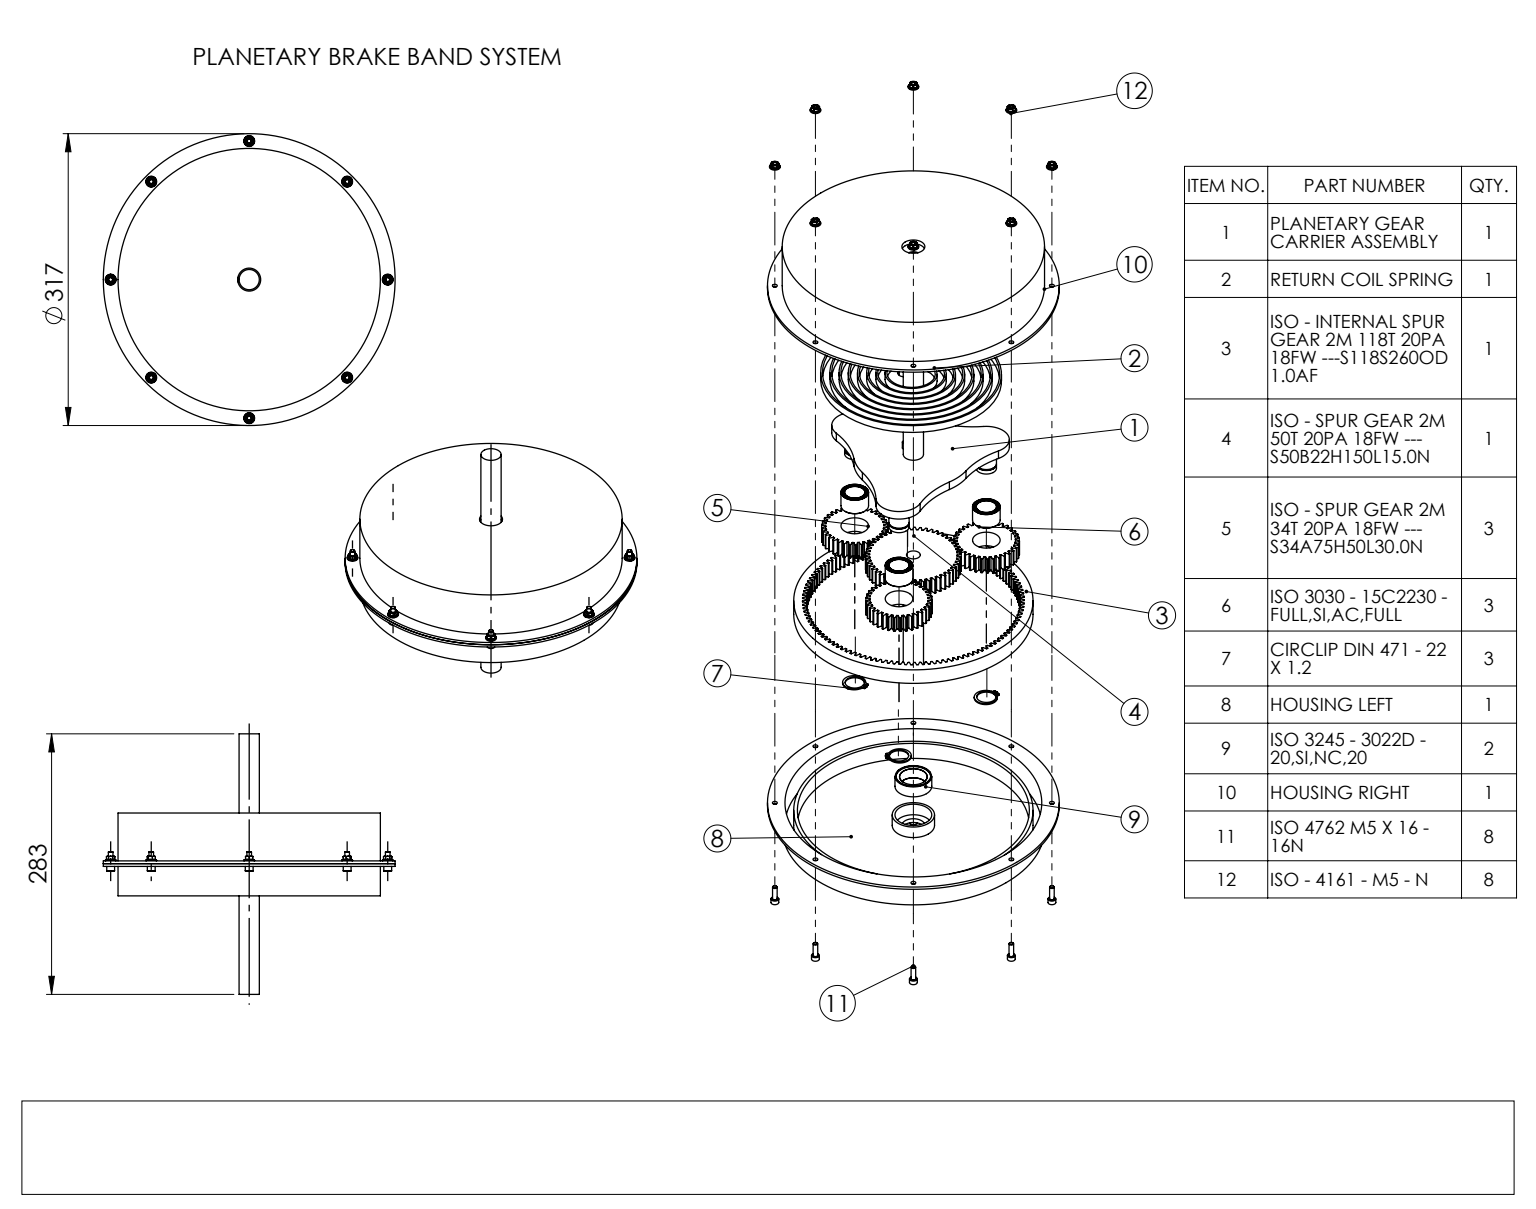
ISO-10303-21;
HEADER;
FILE_DESCRIPTION (('STEP AP214'),
    '1' );
FILE_NAME ('BR-544',
    '2026-10-08T11:45:07',
    ( '' ),
    ( '' ),
    'SwSTEP 2.0',
    'SolidWorks 2026',
    '' );
FILE_SCHEMA (( 'AUTOMOTIVE_DESIGN' ));
ENDSEC;

DATA;
#1 = TOROIDAL_SURFACE ( 'NONE', #14678, 14.91999999999999815, 0.08000000000000020983 ) ;
#2 = EDGE_CURVE ( 'NONE', #17487, #8430, #16356, .T. ) ;
#3 = AXIS2_PLACEMENT_3D ( 'NONE', #17893, #37479, #17456 ) ;
#4 = CYLINDRICAL_SURFACE ( 'NONE', #27715, 12.55910585664918422 ) ;
#5 = ORIENTED_EDGE ( 'NONE', *, *, #3352, .T. ) ;
#6 = CIRCLE ( 'NONE', #19608, 51.99999999999999289 ) ;
#7 = DIRECTION ( 'NONE',  ( 0.000000000000000000, 0.000000000000000000, 1.000000000000000000 ) ) ;
#8 = CARTESIAN_POINT ( 'NONE',  ( -38.31599561464027914, 40.00000000000000000, 10.26995502114586678 ) ) ;
#9 = CARTESIAN_POINT ( 'NONE',  ( -48.87578956996785706, 40.00000000000000000, 16.50293044077288940 ) ) ;
#10 = ORIENTED_EDGE ( 'NONE', *, *, #28549, .F. ) ;
#11 = ORIENTED_EDGE ( 'NONE', *, *, #25156, .T. ) ;
#12 = CARTESIAN_POINT ( 'NONE',  ( 18.00000000000000355, 45.78515115856060191, -12.64416602183617577 ) ) ;
#13 = DIRECTION ( 'NONE',  ( -1.000000000000000000, -0.000000000000000000, 0.000000000000000000 ) ) ;
#14 = CARTESIAN_POINT ( 'NONE',  ( 0.000000000000000000, -47.32430374665948136, 21.55018039121509688 ) ) ;
#15 = DIRECTION ( 'NONE',  ( 0.000000000000000000, -0.8443279255020199603, 0.5358267949789887741 ) ) ;
#16 = VERTEX_POINT ( 'NONE', #31754 ) ;
#17 = DIRECTION ( 'NONE',  ( -1.000000000000000000, -0.000000000000000000, -0.000000000000000000 ) ) ;
#18 = VERTEX_POINT ( 'NONE', #18483 ) ;
#19 = CARTESIAN_POINT ( 'NONE',  ( -15.99999999999997691, 17.11489954122026447, -2.499999999999994671 ) ) ;
#20 = EDGE_CURVE ( 'NONE', #11424, #24676, #28236, .T. ) ;
#21 = CARTESIAN_POINT ( 'NONE',  ( 0.000000000000000000, -2.357898499370432166, 3.035766082959412415E-15 ) ) ;
#22 = AXIS2_PLACEMENT_3D ( 'NONE', #1481, #10457, #24659 ) ;
#23 = ORIENTED_EDGE ( 'NONE', *, *, #27542, .T. ) ;
#24 = CARTESIAN_POINT ( 'NONE',  ( 17.99999999999999645, 110.3490479609632615, -20.28201389785435182 ) ) ;
#25 = CARTESIAN_POINT ( 'NONE',  ( 0.000000000000000000, 87.74575819880270444, -75.87280091124384285 ) ) ;
#26 = ORIENTED_EDGE ( 'NONE', *, *, #36883, .F. ) ;
#27 = DIRECTION ( 'NONE',  ( 0.000000000000000000, 0.000000000000000000, 1.000000000000000000 ) ) ;
#28 = EDGE_LOOP ( 'NONE', ( #968, #9890, #25897, #21708 ) ) ;
#29 = AXIS2_PLACEMENT_3D ( 'NONE', #16710, #27155, #33463 ) ;
#30 = DIRECTION ( 'NONE',  ( -1.000000000000000000, 0.000000000000000000, 0.000000000000000000 ) ) ;
#31 = AXIS2_PLACEMENT_3D ( 'NONE', #21762, #8191, #21965 ) ;
#32 = ORIENTED_EDGE ( 'NONE', *, *, #36401, .F. ) ;
#34 = EDGE_LOOP ( 'NONE', ( #7797, #14411, #2119, #1925 ) ) ;
#33 = DIRECTION ( 'NONE',  ( -1.000000000000000000, -0.000000000000000000, -0.000000000000000000 ) ) ;
#35 = CIRCLE ( 'NONE', #41130, 12.49999999999993427 ) ;
#36 = CARTESIAN_POINT ( 'NONE',  ( -50.06114249714176623, 31.00000000000000355, -38.53249520213265811 ) ) ;
#37 = ORIENTED_EDGE ( 'NONE', *, *, #41403, .T. ) ;
#38 = DIRECTION ( 'NONE',  ( 0.000000000000000000, 0.6382441836448160544, 0.7698339834299096074 ) ) ;
#39 = AXIS2_PLACEMENT_3D ( 'NONE', #35001, #14966, #41543 ) ;
#40 = EDGE_CURVE ( 'NONE', #21663, #37965, #25471, .T. ) ;
#41 = EDGE_LOOP ( 'NONE', ( #1865, #17158, #11037, #34239 ) ) ;
#42 = CARTESIAN_POINT ( 'NONE',  ( 17.99999999999999645, 101.1249659627849269, 48.60055280209592610 ) ) ;
#43 = ORIENTED_EDGE ( 'NONE', *, *, #17545, .T. ) ;
#44 = CARTESIAN_POINT ( 'NONE',  ( 25.34170449640226508, 40.00000000000000000, 74.97748276543396173 ) ) ;
#45 = CIRCLE ( 'NONE', #32135, 59.00000000000000000 ) ;
#47 = DIRECTION ( 'NONE',  ( 0.000000000000000000, 0.8183027759081663577, 0.5747874102144109321 ) ) ;
#46 = DIRECTION ( 'NONE',  ( 0.000000000000000000, 0.000000000000000000, 1.000000000000000000 ) ) ;
#48 = DIRECTION ( 'NONE',  ( 3.892440008040322386E-16, -2.658563593772947863E-15, -1.000000000000000000 ) ) ;
#49 = EDGE_LOOP ( 'NONE', ( #22549, #9625, #3734, #25351, #25610, #29887 ) ) ;
#50 = DIRECTION ( 'NONE',  ( 0.000000000000000000, -0.4610925014493325591, 0.8873520750565681015 ) ) ;
#51 = VERTEX_POINT ( 'NONE', #28063 ) ;
#52 = EDGE_CURVE ( 'NONE', #2224, #13079, #24812, .T. ) ;
#53 = SURFACE_SIDE_STYLE ('',( #30002 ) ) ;
#54 = VECTOR ( 'NONE', #12478, 1000.000000000000000 ) ;
#55 = DIRECTION ( 'NONE',  ( 1.000000000000000000, -0.000000000000000000, -0.000000000000000000 ) ) ;
#56 = CARTESIAN_POINT ( 'NONE',  ( 73.00591898829820536, 31.00000000000000000, 19.54754034098114701 ) ) ;
#58 = CARTESIAN_POINT ( 'NONE',  ( -6.076000000000004952, 19.11697999999999809, 0.000000000000000000 ) ) ;
#57 = CARTESIAN_POINT ( 'NONE',  ( -10.00000000000000000, 0.000000000000000000, 0.000000000000000000 ) ) ;
#59 = EDGE_LOOP ( 'NONE', ( #27677, #9320, #7424, #19818 ) ) ;
#60 = DIRECTION ( 'NONE',  ( 1.000000000000000000, 0.000000000000000000, 0.000000000000000000 ) ) ;
#61 = AXIS2_PLACEMENT_3D ( 'NONE', #7256, #13853, #27356 ) ;
#62 = AXIS2_PLACEMENT_3D ( 'NONE', #40135, #23391, #36432 ) ;
#63 = ORIENTED_EDGE ( 'NONE', *, *, #22832, .T. ) ;
#64 = CARTESIAN_POINT ( 'NONE',  ( 17.99999999999999645, 52.88069566989454273, 103.2454939717370905 ) ) ;
#65 = LINE ( 'NONE', #43070, #7397 ) ;
#66 = FILL_AREA_STYLE ('',( #17591 ) ) ;
#67 = AXIS2_PLACEMENT_3D ( 'NONE', #34351, #28055, #11038 ) ;
#68 = DIRECTION ( 'NONE',  ( 0.000000000000000000, 0.000000000000000000, -1.000000000000000000 ) ) ;
#69 = VERTEX_POINT ( 'NONE', #8400 ) ;
#70 = DIRECTION ( 'NONE',  ( -1.000000000000000000, 0.000000000000000000, 0.000000000000000000 ) ) ;
#71 = ORIENTED_EDGE ( 'NONE', *, *, #29230, .F. ) ;
#72 = EDGE_CURVE ( 'NONE', #28961, #19587, #1411, .T. ) ;
#73 = CONICAL_SURFACE ( 'NONE', #24545, 4.000000000000000000, 0.8911886515913786111 ) ;
#74 = CARTESIAN_POINT ( 'NONE',  ( -3.996523416598931009E-15, 2.658563593772952281E-14, 10.00000000000000178 ) ) ;
#75 = EDGE_CURVE ( 'NONE', #34974, #23352, #8192, .T. ) ;
#76 = DIRECTION ( 'NONE',  ( 0.000000000000000000, 0.000000000000000000, -1.000000000000000000 ) ) ;
#77 = CARTESIAN_POINT ( 'NONE',  ( 17.99999999999999645, -107.2703412112692689, -32.88383143828572486 ) ) ;
#78 = ORIENTED_EDGE ( 'NONE', *, *, #40490, .F. ) ;
#79 = ORIENTED_EDGE ( 'NONE', *, *, #11091, .T. ) ;
#80 = DIRECTION ( 'NONE',  ( 1.000000000000000000, 0.000000000000000000, 0.000000000000000000 ) ) ;
#81 = DIRECTION ( 'NONE',  ( 0.000000000000000000, 1.000000000000000000, -1.060184893785364939E-15 ) ) ;
#82 = DIRECTION ( 'NONE',  ( 0.000000000000000000, -1.000000000000000000, 1.287488025362403787E-15 ) ) ;
#84 = ORIENTED_EDGE ( 'NONE', *, *, #2078, .T. ) ;
#83 = DIRECTION ( 'NONE',  ( -1.000000000000000000, 0.000000000000000000, 0.000000000000000000 ) ) ;
#85 = CARTESIAN_POINT ( 'NONE',  ( 15.66220904948440662, 31.00000000000000355, -31.63873590539992264 ) ) ;
#86 = FACE_OUTER_BOUND ( 'NONE', #37742, .T. ) ;
#87 = EDGE_CURVE ( 'NONE', #8500, #34172, #3097, .T. ) ;
#89 = ORIENTED_EDGE ( 'NONE', *, *, #24562, .T. ) ;
#88 = DIRECTION ( 'NONE',  ( 0.000000000000000000, -0.3641605752528294659, 0.9313361774523355452 ) ) ;
#90 = ORIENTED_EDGE ( 'NONE', *, *, #30632, .T. ) ;
#91 = LINE ( 'NONE', #6449, #40012 ) ;
#92 = CIRCLE ( 'NONE', #23863, 2.500000000000000888 ) ;
#93 = DIRECTION ( 'NONE',  ( 0.000000000000000000, -0.3681245526846853022, 0.9297764858882484607 ) ) ;
#94 = CARTESIAN_POINT ( 'NONE',  ( 55.55275676651330485, 40.00000000000000000, 14.97830846782891712 ) ) ;
#95 = B_SPLINE_CURVE_WITH_KNOTS ( 'NONE', 3,
 ( #42025, #12179, #25497, #38758, #5606, #41162, #34637, #4752 ),
 .UNSPECIFIED., .F., .F.,
 ( 4, 2, 2, 4 ),
 ( 2.465131517071352357E-07, 0.001183067374689843057, 0.001774477805458910071, 0.002365888236227977302 ),
 .UNSPECIFIED. ) ;
#96 = DIRECTION ( 'NONE',  ( -1.000000000000000000, -0.000000000000000000, -0.000000000000000000 ) ) ;
#97 = AXIS2_PLACEMENT_3D ( 'NONE', #25295, #22018, #38332 ) ;
#98 = CARTESIAN_POINT ( 'NONE',  ( 17.99999999999999645, -63.24564713401724703, -102.5693868539701299 ) ) ;
#99 = AXIS2_PLACEMENT_3D ( 'NONE', #5218, #41425, #18366 ) ;
#100 = CARTESIAN_POINT ( 'NONE',  ( 17.99999999999999645, 103.1672962317651496, 44.09967643725903486 ) ) ;
#101 = EDGE_LOOP ( 'NONE', ( #3389, #16998, #1175, #14979 ) ) ;
#102 = CARTESIAN_POINT ( 'NONE',  ( 17.99999999999999645, 83.49789599728782719, 86.88263557826796557 ) ) ;
#103 = ORIENTED_EDGE ( 'NONE', *, *, #29129, .T. ) ;
#104 = EDGE_CURVE ( 'NONE', #19737, #29429, #22699, .T. ) ;
#105 = AXIS2_PLACEMENT_3D ( 'NONE', #12289, #32756, #5713 ) ;
#106 = DIRECTION ( 'NONE',  ( -1.000000000000000000, -0.000000000000000000, -0.000000000000000000 ) ) ;
#107 = DIRECTION ( 'NONE',  ( 0.000000000000000000, 0.000000000000000000, 1.000000000000000000 ) ) ;
#108 = ADVANCED_FACE ( 'NONE', ( #34802 ), #31105, .T. ) ;
#109 = CARTESIAN_POINT ( 'NONE',  ( 33.03432996520027132, 31.00000000000000355, -28.98482729919588863 ) ) ;
#110 = FACE_OUTER_BOUND ( 'NONE', #19769, .T. ) ;
#111 = EDGE_LOOP ( 'NONE', ( #9631, #34860, #21695, #15312 ) ) ;
#112 = MANIFOLD_SOLID_BREP ( 'Hex', #10772 ) ;
#113 = PRODUCT ( 'needle roller bearing_nm_iso_ISO 3030 - 15C2230 - Full,SI,AC,Full', 'needle roller bearing_nm_iso_ISO 3030 - 15C2230 - Full,SI,AC,Full', '', ( #9801 ) ) ;
#114 = CARTESIAN_POINT ( 'NONE',  ( 0.000000000000000000, 0.000000000000000000, 0.000000000000000000 ) ) ;
#115 = ORIENTED_EDGE ( 'NONE', *, *, #13945, .F. ) ;
#116 = CARTESIAN_POINT ( 'NONE',  ( -78.67873774631718220, 31.00000000000000711, 60.36924185307643143 ) ) ;
#117 = EDGE_LOOP ( 'NONE', ( #1029, #31405, #36009, #13275 ) ) ;
#118 = LINE ( 'NONE', #13486, #30404 ) ;
#119 = CARTESIAN_POINT ( 'NONE',  ( -67.85934734803990409, 31.00000000000000711, 22.92939687791763248 ) ) ;
#120 = CARTESIAN_POINT ( 'NONE',  ( 33.43413415811954792, 40.00000000000000000, -67.56680175473154293 ) ) ;
#121 = DIRECTION ( 'NONE',  ( -1.000000000000000000, -0.000000000000000000, -0.000000000000000000 ) ) ;
#122 = ORIENTED_EDGE ( 'NONE', *, *, #28926, .T. ) ;
#123 = EDGE_LOOP ( 'NONE', ( #24537, #25112, #5248, #36147 ) ) ;
#124 = CARTESIAN_POINT ( 'NONE',  ( 0.000000000000000000, 0.000000000000000000, 0.000000000000000000 ) ) ;
#125 = AXIS2_PLACEMENT_3D ( 'NONE', #20168, #39735, #23218 ) ;
#126 = ADVANCED_FACE ( 'NONE', ( #11053 ), #35784, .T. ) ;
#127 = CARTESIAN_POINT ( 'NONE',  ( 17.99999999999999645, -69.90696807222417419, -98.15042952503588936 ) ) ;
#128 = DIRECTION ( 'NONE',  ( -0.8660254037844377084, -0.5000000000000015543, 0.000000000000000000 ) ) ;
#129 = EDGE_CURVE ( 'NONE', #6394, #7217, #14300, .T. ) ;
#130 = EDGE_CURVE ( 'NONE', #29194, #21952, #31734, .T. ) ;
#131 = ADVANCED_FACE ( 'NONE', ( #11260 ), #25041, .T. ) ;
#133 = EDGE_CURVE ( 'NONE', #32336, #24871, #39498, .T. ) ;
#132 = CIRCLE ( 'NONE', #17653, 142.4999999999992610 ) ;
#135 = ORIENTED_EDGE ( 'NONE', *, *, #35134, .T. ) ;
#134 = DIRECTION ( 'NONE',  ( 3.009274222672345096E-17, 1.000000000000000000, -2.455023325076455345E-18 ) ) ;
#136 = CARTESIAN_POINT ( 'NONE',  ( 17.99999999999999645, 41.60679253225764285, 108.2814610871947423 ) ) ;
#137 = EDGE_LOOP ( 'NONE', ( #388, #32106, #23613, #3341 ) ) ;
#138 = CARTESIAN_POINT ( 'NONE',  ( 17.99999999999999645, 107.2885202478266251, 54.86040852957351888 ) ) ;
#139 = CARTESIAN_POINT ( 'NONE',  ( -5.399612364985466151, 40.00000000000000000, -82.39583333413678190 ) ) ;
#140 = CARTESIAN_POINT ( 'NONE',  ( -2.688821387764050996E-14, -4.618802153517012954, -0.4999999999999995559 ) ) ;
#141 = ORIENTED_EDGE ( 'NONE', *, *, #25701, .T. ) ;
#142 = DIRECTION ( 'NONE',  ( 1.000000000000000000, 0.000000000000000000, -0.000000000000000000 ) ) ;
#143 = CARTESIAN_POINT ( 'NONE',  ( 0.000000000000000000, 101.1249659627849269, 48.60055280209592610 ) ) ;
#144 = ORIENTED_EDGE ( 'NONE', *, *, #10315, .T. ) ;
#145 = ORIENTED_EDGE ( 'NONE', *, *, #19754, .F. ) ;
#146 = FACE_OUTER_BOUND ( 'NONE', #5091, .T. ) ;
#147 = ORIENTED_EDGE ( 'NONE', *, *, #18446, .T. ) ;
#148 = FACE_OUTER_BOUND ( 'NONE', #24269, .T. ) ;
#149 = DIRECTION ( 'NONE',  ( 0.000000000000000000, 0.000000000000000000, 1.000000000000000000 ) ) ;
#150 = CARTESIAN_POINT ( 'NONE',  ( 17.99999999999999645, 69.90696807222620635, -98.15042952503443985 ) ) ;
#151 = DIRECTION ( 'NONE',  ( 0.000000000000000000, 0.000000000000000000, -1.000000000000000000 ) ) ;
#152 = CARTESIAN_POINT ( 'NONE',  ( 17.99999999999999645, -53.40478689619660457, -108.0204598100370816 ) ) ;
#153 = ORIENTED_EDGE ( 'NONE', *, *, #32598, .F. ) ;
#155 = DIRECTION ( 'NONE',  ( 1.000000000000000000, 0.000000000000000000, 0.000000000000000000 ) ) ;
#154 = CARTESIAN_POINT ( 'NONE',  ( 17.99999999999999645, 120.2856157092986678, 7.201503623197233139 ) ) ;
#156 = EDGE_LOOP ( 'NONE', ( #41702, #6494, #6185, #41274 ) ) ;
#157 = ADVANCED_FACE ( 'NONE', ( #19485 ), #6553, .F. ) ;
#158 = AXIS2_PLACEMENT_3D ( 'NONE', #4980, #24654, #21174 ) ;
#159 =( LENGTH_UNIT ( ) NAMED_UNIT ( * ) SI_UNIT ( .MILLI., .METRE. ) );
#160 = CARTESIAN_POINT ( 'NONE',  ( 9.000000000000001776, -13.00789606333550097, 115.2683592318614672 ) ) ;
#161 = ADVANCED_FACE ( 'NONE', ( #9836 ), #29711, .F. ) ;
#162 = DIRECTION ( 'NONE',  ( 0.000000000000000000, 0.1062934856473588541, 0.9943348002101377592 ) ) ;
#163 = ORIENTED_EDGE ( 'NONE', *, *, #20925, .F. ) ;
#164 = CARTESIAN_POINT ( 'NONE',  ( 17.99999999999999645, -97.89532456239533076, 54.81585448086167389 ) ) ;
#165 = CIRCLE ( 'NONE', #25315, 58.99999999999999289 ) ;
#166 = DIRECTION ( 'NONE',  ( 1.000000000000000000, 0.000000000000000000, 0.000000000000000000 ) ) ;
#167 = DIRECTION ( 'NONE',  ( 0.000000000000000000, 0.000000000000000000, 1.000000000000000000 ) ) ;
#168 = CARTESIAN_POINT ( 'NONE',  ( -23.19911330973958030, 31.00000000000000355, -68.30030121463531145 ) ) ;
#169 = AXIS2_PLACEMENT_3D ( 'NONE', #24006, #33787, #20520 ) ;
#170 = VERTEX_POINT ( 'NONE', #16346 ) ;
#171 = CARTESIAN_POINT ( 'NONE',  ( 32.80084743084299248, 31.00000000000000355, 19.01436317119123842 ) ) ;
#172 = CARTESIAN_POINT ( 'NONE',  ( -21.28946418274055929, 40.00000000000000000, -79.45670318283352174 ) ) ;
#173 = DIRECTION ( 'NONE',  ( 1.000000000000000000, 0.000000000000000000, 0.000000000000000000 ) ) ;
#174 = EDGE_CURVE ( 'NONE', #31622, #37862, #2414, .T. ) ;
#175 = EDGE_CURVE ( 'NONE', #28450, #28268, #33086, .T. ) ;
#176 = ADVANCED_FACE ( 'NONE', ( #26221 ), #23396, .F. ) ;
#177 = ORIENTED_EDGE ( 'NONE', *, *, #6345, .F. ) ;
#178 = CARTESIAN_POINT ( 'NONE',  ( 18.00000000000000355, 20.99948489194481738, -42.60488980472760545 ) ) ;
#179 = DIRECTION ( 'NONE',  ( -1.000000000000000000, 0.000000000000000000, 0.000000000000000000 ) ) ;
#180 = ADVANCED_FACE ( 'NONE', ( #36225 ), #26652, .F. ) ;
#181 = AXIS2_PLACEMENT_3D ( 'NONE', #33308, #3602, #40474 ) ;
#182 = ORIENTED_EDGE ( 'NONE', *, *, #35349, .F. ) ;
#183 = CARTESIAN_POINT ( 'NONE',  ( 50.09382087749727930, 40.00000000000000000, 24.69014870349942825 ) ) ;
#184 = DIRECTION ( 'NONE',  ( -0.2140725878556641593, -0.9768177553304296934, 0.000000000000000000 ) ) ;
#185 = CARTESIAN_POINT ( 'NONE',  ( 53.30287614962722387, -35.35525454449572180, 69.29271901957299917 ) ) ;
#186 = ORIENTED_EDGE ( 'NONE', *, *, #2030, .F. ) ;
#187 = CARTESIAN_POINT ( 'NONE',  ( 0.000000000000000000, 82.63181128086846172, -81.41243003646886223 ) ) ;
#188 = CARTESIAN_POINT ( 'NONE',  ( -36.79328511490363240, -2.055254544495723756, -55.66638716446937707 ) ) ;
#189 = VERTEX_POINT ( 'NONE', #6781 ) ;
#190 = CARTESIAN_POINT ( 'NONE',  ( 17.99999999999999645, -31.80866420683992857, 2.997093558041182160 ) ) ;
#191 = EDGE_CURVE ( 'NONE', #37998, #17546, #11534, .T. ) ;
#192 = VERTEX_POINT ( 'NONE', #36012 ) ;
#193 = COLOUR_RGB ( '', 0.72549020, 0.75294118, 0.79215686) ;
#194 = AXIS2_PLACEMENT_3D ( 'NONE', #18783, #32450, #2540 ) ;
#195 = ORIENTED_EDGE ( 'NONE', *, *, #39418, .T. ) ;
#196 = DIRECTION ( 'NONE',  ( -3.996523416598930318E-16, 2.658563593772947863E-15, 1.000000000000000000 ) ) ;
#197 = CARTESIAN_POINT ( 'NONE',  ( 96.56285295106283684, 31.00000000000000000, 12.84127866191736977 ) ) ;
#198 = ORIENTED_EDGE ( 'NONE', *, *, #13590, .F. ) ;
#199 = CARTESIAN_POINT ( 'NONE',  ( 9.000000000000001776, -30.03615769709704608, -42.44795908869020451 ) ) ;
#200 = DIRECTION ( 'NONE',  ( -0.000000000000000000, -0.000000000000000000, 1.000000000000000000 ) ) ;
#201 = DIRECTION ( 'NONE',  ( 1.000000000000000000, -0.000000000000000000, 0.000000000000000000 ) ) ;
#202 = ORIENTED_EDGE ( 'NONE', *, *, #13580, .T. ) ;
#203 = CARTESIAN_POINT ( 'NONE',  ( 0.000000000000000000, -112.8457601792517124, 26.86697618949339272 ) ) ;
#204 = LINE ( 'NONE', #34053, #4600 ) ;
#205 = AXIS2_PLACEMENT_3D ( 'NONE', #38248, #21520, #38029 ) ;
#207 = CYLINDRICAL_SURFACE ( 'NONE', #17131, 20.00000000000000355 ) ;
#206 = DIRECTION ( 'NONE',  ( 0.000000000000000000, -0.9407002666710364558, 0.3392388661180213427 ) ) ;
#208 = AXIS2_PLACEMENT_3D ( 'NONE', #11929, #8841, #8617 ) ;
#209 = CARTESIAN_POINT ( 'NONE',  ( 17.99999999999999645, -110.0562500189201955, 49.07252625220073838 ) ) ;
#210 = ORIENTED_EDGE ( 'NONE', *, *, #16995, .T. ) ;
#211 =( LENGTH_UNIT ( ) NAMED_UNIT ( * ) SI_UNIT ( .MILLI., .METRE. ) );
#212 = AXIS2_PLACEMENT_3D ( 'NONE', #31464, #8530, #17983 ) ;
#213 = CARTESIAN_POINT ( 'NONE',  ( -25.29482881991252086, 31.00000000000000355, -32.96004927633274662 ) ) ;
#214 = VERTEX_POINT ( 'NONE', #29493 ) ;
#215 = DIRECTION ( 'NONE',  ( 1.000000000000000000, 0.000000000000000000, -3.273063162220425331E-16 ) ) ;
#216 = DIRECTION ( 'NONE',  ( -1.000000000000000000, 0.000000000000000000, 0.000000000000000000 ) ) ;
#217 = ORIENTED_EDGE ( 'NONE', *, *, #22395, .F. ) ;
#218 = LINE ( 'NONE', #26245, #34087 ) ;
#219 = CARTESIAN_POINT ( 'NONE',  ( 32.11716166826300167, 40.00000000000000000, 15.82712457579038912 ) ) ;
#220 = STYLED_ITEM ( 'NONE', ( #39718 ), #29693 ) ;
#221 = CARTESIAN_POINT ( 'NONE',  ( 42.86166521172830102, 40.00000000000000000, 21.22462828019262204 ) ) ;
#222 = AXIS2_PLACEMENT_3D ( 'NONE', #57, #6628, #19990 ) ;
#223 = ORIENTED_EDGE ( 'NONE', *, *, #13346, .T. ) ;
#224 = CARTESIAN_POINT ( 'NONE',  ( 17.99999999999999645, -23.87611429743648017, -20.54551452399645939 ) ) ;
#225 = DIRECTION ( 'NONE',  ( -1.000000000000000000, 0.000000000000000000, 0.000000000000000000 ) ) ;
#226 = EDGE_CURVE ( 'NONE', #9576, #14223, #10277, .T. ) ;
#227 = AXIS2_PLACEMENT_3D ( 'NONE', #26910, #27140, #24089 ) ;
#228 = CARTESIAN_POINT ( 'NONE',  ( -102.9608013043458072, -35.35525454449571470, 14.45886780445738218 ) ) ;
#229 = ORIENTED_EDGE ( 'NONE', *, *, #13847, .F. ) ;
#230 = CARTESIAN_POINT ( 'NONE',  ( 7.028922914820973311, 40.00000000000000000, 26.21578750688660264 ) ) ;
#231 = ORIENTED_EDGE ( 'NONE', *, *, #17154, .T. ) ;
#232 = LINE ( 'NONE', #33434, #6211 ) ;
#233 = CARTESIAN_POINT ( 'NONE',  ( 0.000000000000000000, 12.42760411676038146, 33.78690065568429191 ) ) ;
#234 =( REPRESENTATION_RELATIONSHIP ('NONE','NONE', #330, #37437 ) REPRESENTATION_RELATIONSHIP_WITH_TRANSFORMATION ( #8267 )SHAPE_REPRESENTATION_RELATIONSHIP( ) );
#235 = VERTEX_POINT ( 'NONE', #20345 ) ;
#236 = DIRECTION ( 'NONE',  ( 0.000000000000000000, 0.3140767120219495334, -0.9493976084683810601 ) ) ;
#237 = VECTOR ( 'NONE', #15107, 1000.000000000000000 ) ;
#238 = FACE_OUTER_BOUND ( 'NONE', #26879, .T. ) ;
#239 = VERTEX_POINT ( 'NONE', #9633 ) ;
#240 = CYLINDRICAL_SURFACE ( 'NONE', #4769, 20.00000000000000355 ) ;
#241 = EDGE_LOOP ( 'NONE', ( #31770, #30351, #32768, #20385 ) ) ;
#242 = DIRECTION ( 'NONE',  ( -1.000000000000000000, -0.000000000000000000, -0.000000000000000000 ) ) ;
#243 = EDGE_CURVE ( 'NONE', #7044, #26460, #16384, .T. ) ;
#244 = CIRCLE ( 'NONE', #9337, 59.00000000000001421 ) ;
#245 = ORIENTED_EDGE ( 'NONE', *, *, #22971, .F. ) ;
#247 = ORIENTED_EDGE ( 'NONE', *, *, #11286, .T. ) ;
#246 = CARTESIAN_POINT ( 'NONE',  ( 150.4999999999986926, 1.388241670201576064E-12, 6.999999999999959144 ) ) ;
#248 = EDGE_CURVE ( 'NONE', #1617, #22493, #17123, .T. ) ;
#249 = CARTESIAN_POINT ( 'NONE',  ( -20.51812799676685373, 31.00000000000000355, -60.74091093256831897 ) ) ;
#250 = EDGE_LOOP ( 'NONE', ( #8958, #20095, #42612, #31165 ) ) ;
#251 = DIRECTION ( 'NONE',  ( -1.000000000000000000, -0.000000000000000000, 0.000000000000000000 ) ) ;
#252 = VERTEX_POINT ( 'NONE', #20289 ) ;
#253 = ORIENTED_EDGE ( 'NONE', *, *, #22562, .T. ) ;
#254 = DIRECTION ( 'NONE',  ( 0.000000000000000000, -6.938893903907226011E-15, 1.000000000000000000 ) ) ;
#255 = VERTEX_POINT ( 'NONE', #36433 ) ;
#257 = CARTESIAN_POINT ( 'NONE',  ( -10.54315780146311532, 40.00000000000000000, 79.17709703063971460 ) ) ;
#256 = MECHANICAL_DESIGN_GEOMETRIC_PRESENTATION_REPRESENTATION (  '', ( #37909 ), #12862 ) ;
#259 = LINE ( 'NONE', #7052, #31169 ) ;
#258 = DIRECTION ( 'NONE',  ( 1.000000000000000000, 0.000000000000000000, 0.000000000000000000 ) ) ;
#260 = FACE_OUTER_BOUND ( 'NONE', #10790, .T. ) ;
#261 = ORIENTED_EDGE ( 'NONE', *, *, #7947, .F. ) ;
#262 = DIRECTION ( 'NONE',  ( 0.000000000000000000, -0.9980267284282708928, -0.06279051952932436509 ) ) ;
#263 = AXIS2_PLACEMENT_3D ( 'NONE', #41212, #8072, #27508 ) ;
#264 = ORIENTED_EDGE ( 'NONE', *, *, #41206, .T. ) ;
#265 = FILL_AREA_STYLE_COLOUR ( '', #39229 ) ;
#266 = CIRCLE ( 'NONE', #34432, 20.00000000000000711 ) ;
#267 = VERTEX_POINT ( 'NONE', #42555 ) ;
#268 = VECTOR ( 'NONE', #36102, 1000.000000000000000 ) ;
#269 = DIRECTION ( 'NONE',  ( 0.000000000000000000, 0.000000000000000000, 1.000000000000000000 ) ) ;
#270 = CARTESIAN_POINT ( 'NONE',  ( -45.94448050778635917, 31.00000000000000355, -79.54744219826071117 ) ) ;
#271 = CARTESIAN_POINT ( 'NONE',  ( 3.453038570460273071, 2.625189405340834448, -3.535263753543585352 ) ) ;
#272 = EDGE_LOOP ( 'NONE', ( #37199, #32601, #38048, #42708 ) ) ;
#273 = AXIS2_PLACEMENT_3D ( 'NONE', #24892, #15283, #24662 ) ;
#274 = CARTESIAN_POINT ( 'NONE',  ( 0.000000000000000000, -47.58001226230612701, 110.7096808509482031 ) ) ;
#275 = AXIS2_PLACEMENT_3D ( 'NONE', #8438, #38320, #31571 ) ;
#276 = VERTEX_POINT ( 'NONE', #12704 ) ;
#277 = FACE_OUTER_BOUND ( 'NONE', #26968, .T. ) ;
#278 = DIRECTION ( 'NONE',  ( 1.000000000000000000, 0.000000000000000000, 0.000000000000000000 ) ) ;
#279 = DIRECTION ( 'NONE',  ( 0.000000000000000000, 2.587384167558627638E-15, -1.000000000000000000 ) ) ;
#280 = EDGE_CURVE ( 'NONE', #25913, #26598, #17814, .T. ) ;
#281 = CARTESIAN_POINT ( 'NONE',  ( 106.9999999999993179, -2.318365118890836037E-13, -32.00000000000000000 ) ) ;
#282 = AXIS2_PLACEMENT_3D ( 'NONE', #26118, #29184, #16298 ) ;
#283 = ADVANCED_FACE ( 'NONE', ( #13571 ), #32962, .T. ) ;
#284 = AXIS2_PLACEMENT_3D ( 'NONE', #17141, #30851, #4209 ) ;
#285 = EDGE_LOOP ( 'NONE', ( #5183, #4420, #32510, #24970 ) ) ;
#286 = CARTESIAN_POINT ( 'NONE',  ( -10.00000000000000000, 0.000000000000000000, 0.000000000000000000 ) ) ;
#287 = VERTEX_POINT ( 'NONE', #19913 ) ;
#288 = DIRECTION ( 'NONE',  ( 1.000000000000000000, -0.000000000000000000, 0.000000000000000000 ) ) ;
#289 = DIRECTION ( 'NONE',  ( -1.000000000000000000, -0.000000000000000000, -0.000000000000000000 ) ) ;
#290 = DIRECTION ( 'NONE',  ( -1.000000000000000000, -0.000000000000000000, 0.000000000000000000 ) ) ;
#291 = VERTEX_POINT ( 'NONE', #33181 ) ;
#292 = ORIENTED_EDGE ( 'NONE', *, *, #9832, .T. ) ;
#293 = DIRECTION ( 'NONE',  ( -1.000000000000000000, -0.000000000000000000, -0.000000000000000000 ) ) ;
#294 = VECTOR ( 'NONE', #25496, 1000.000000000000000 ) ;
#295 = CARTESIAN_POINT ( 'NONE',  ( 0.000000000000000000, -58.30069736313732420, 100.2847380560565256 ) ) ;
#296 = EDGE_CURVE ( 'NONE', #640, #8463, #3270, .T. ) ;
#297 = CARTESIAN_POINT ( 'NONE',  ( 4.197478902586992966, -0.8524102783748346290, -3.505063281295504041 ) ) ;
#298 = AXIS2_PLACEMENT_3D ( 'NONE', #37715, #19724, #6582 ) ;
#300 = VERTEX_POINT ( 'NONE', #27299 ) ;
#299 = DIRECTION ( 'NONE',  ( 0.000000000000000000, 0.000000000000000000, 1.000000000000000000 ) ) ;
#301 = EDGE_CURVE ( 'NONE', #6489, #17266, #7326, .T. ) ;
#302 = CARTESIAN_POINT ( 'NONE',  ( -29.39530816626169241, 31.00000000000000355, -14.54745122861254814 ) ) ;
#303 = CIRCLE ( 'NONE', #42788, 24.99999999999998934 ) ;
#304 = CYLINDRICAL_SURFACE ( 'NONE', #9787, 116.0000000000000000 ) ;
#305 = AXIS2_PLACEMENT_3D ( 'NONE', #35239, #21983, #28308 ) ;
#306 = ADVANCED_FACE ( 'NONE', ( #37955 ), #862, .F. ) ;
#308 = ORIENTED_EDGE ( 'NONE', *, *, #23205, .T. ) ;
#307 = CARTESIAN_POINT ( 'NONE',  ( 0.000000000000000000, -18.53613841426822972, 48.58406706613896375 ) ) ;
#309 = UNCERTAINTY_MEASURE_WITH_UNIT (LENGTH_MEASURE( 1.000000000000000082E-05 ), #5379, 'distance_accuracy_value', 'NONE');
#310 = AXIS2_PLACEMENT_3D ( 'NONE', #8177, #1395, #28267 ) ;
#311 = ORIENTED_EDGE ( 'NONE', *, *, #38978, .F. ) ;
#312 = CARTESIAN_POINT ( 'NONE',  ( -130.0000000000000284, 4.615443851143735910E-16, -20.00000000000000000 ) ) ;
#313 = CARTESIAN_POINT ( 'NONE',  ( 0.000000000000000000, -69.72480978690109055, 92.70626138605992139 ) ) ;
#314 = CARTESIAN_POINT ( 'NONE',  ( -17.30549157494238344, 40.00000000000000000, -51.24895740946764988 ) ) ;
#315 = DIRECTION ( 'NONE',  ( -1.000000000000000000, 0.000000000000000000, -0.000000000000000000 ) ) ;
#316 = DIRECTION ( 'NONE',  ( 0.000000000000000000, 0.000000000000000000, -1.000000000000000000 ) ) ;
#317 = EDGE_LOOP ( 'NONE', ( #16591, #23774, #39955, #12184 ) ) ;
#318 = CARTESIAN_POINT ( 'NONE',  ( -6.004904395537136175, 0.000000000000000000, 0.000000000000000000 ) ) ;
#319 = EDGE_CURVE ( 'NONE', #36754, #15839, #12891, .T. ) ;
#320 = CIRCLE ( 'NONE', #19206, 15.08402000000000065 ) ;
#321 = ORIENTED_EDGE ( 'NONE', *, *, #37167, .T. ) ;
#322 = EDGE_CURVE ( 'NONE', #29751, #6854, #14213, .T. ) ;
#323 = LINE ( 'NONE', #26764, #22557 ) ;
#324 = CARTESIAN_POINT ( 'NONE',  ( -105.9879088449591933, 17.11489954122026447, -4.880719929157669945 ) ) ;
#326 = EDGE_CURVE ( 'NONE', #40378, #9051, #40786, .T. ) ;
#325 = CARTESIAN_POINT ( 'NONE',  ( 3.108867721649529958, 31.00000000000000355, 47.39583333474234905 ) ) ;
#327 = DIRECTION ( 'NONE',  ( 0.000000000000000000, 0.7980172272802363853, 0.6026346363792605132 ) ) ;
#328 = ORIENTED_EDGE ( 'NONE', *, *, #42015, .T. ) ;
#329 = AXIS2_PLACEMENT_3D ( 'NONE', #17951, #33827, #8078 ) ;
#330 = SHAPE_REPRESENTATION ( 'BR-544', ( #39970, #29548, #18472, #10727, #11463, #9346, #30946, #39281, #26770, #15640, #19143, #4447, #33013, #7253, #17047, #35107, #30261, #40659, #33731, #14235, #3017, #6528, #42769, #10026, #3741, #24722, #13548, #28191, #14967, #38586, #22632, #19820, #27462, #32334 ), #21922 ) ;
#331 = AXIS2_PLACEMENT_3D ( 'NONE', #35354, #42727, #6106 ) ;
#332 = AXIS2_PLACEMENT_3D ( 'NONE', #8992, #29286, #42557 ) ;
#333 = CARTESIAN_POINT ( 'NONE',  ( -20.64238946400878305, 31.00000000000000355, 3.177240882809045708 ) ) ;
#334 = ORIENTED_EDGE ( 'NONE', *, *, #29415, .T. ) ;
#335 = CARTESIAN_POINT ( 'NONE',  ( 58.84426737335365232, 31.00000000000000355, 76.69096868241209108 ) ) ;
#336 = VECTOR ( 'NONE', #7785, 1000.000000000000000 ) ;
#337 = ORIENTED_EDGE ( 'NONE', *, *, #41838, .F. ) ;
#338 = AXIS2_PLACEMENT_3D ( 'NONE', #11324, #23403, #24655 ) ;
#339 = CARTESIAN_POINT ( 'NONE',  ( 17.99999999999999645, -10.40101730206447961, 120.0512800434970728 ) ) ;
#340 = CARTESIAN_POINT ( 'NONE',  ( -25.88810397299713628, 31.00000000000000355, 75.89534075019484760 ) ) ;
#342 = AXIS2_PLACEMENT_3D ( 'NONE', #2271, #15629, #28936 ) ;
#341 = CARTESIAN_POINT ( 'NONE',  ( -79.00001692107187523, 40.00000000000000711, 21.04436337234429999 ) ) ;
#343 = FACE_OUTER_BOUND ( 'NONE', #19727, .T. ) ;
#344 = EDGE_CURVE ( 'NONE', #2343, #1360, #19212, .T. ) ;
#345 = AXIS2_PLACEMENT_3D ( 'NONE', #9675, #6388, #43032 ) ;
#346 = ORIENTED_EDGE ( 'NONE', *, *, #31412, .T. ) ;
#347 = DIRECTION ( 'NONE',  ( -1.000000000000000000, -0.000000000000000000, -0.000000000000000000 ) ) ;
#348 = ORIENTED_EDGE ( 'NONE', *, *, #42438, .F. ) ;
#349 = DIRECTION ( 'NONE',  ( -1.000000000000000000, -0.000000000000000000, -0.000000000000000000 ) ) ;
#350 = FACE_OUTER_BOUND ( 'NONE', #25908, .T. ) ;
#352 = ORIENTED_EDGE ( 'NONE', *, *, #296, .F. ) ;
#351 = CYLINDRICAL_SURFACE ( 'NONE', #6056, 18.77999999999999403 ) ;
#353 = LINE ( 'NONE', #36584, #16374 ) ;
#354 = ORIENTED_EDGE ( 'NONE', *, *, #6008, .F. ) ;
#355 = DIRECTION ( 'NONE',  ( 0.000000000000000000, 0.7705132427757904745, -0.6374239897486881912 ) ) ;
#356 = EDGE_CURVE ( 'NONE', #26178, #21757, #8740, .T. ) ;
#357 = CARTESIAN_POINT ( 'NONE',  ( 36.87680687886029318, 40.00000000000000000, -74.81172728975037955 ) ) ;
#358 = DIRECTION ( 'NONE',  ( -1.000000000000000000, -0.000000000000000000, -0.000000000000000000 ) ) ;
#359 = ORIENTED_EDGE ( 'NONE', *, *, #32192, .T. ) ;
#360 = CARTESIAN_POINT ( 'NONE',  ( 17.99999999999999645, -103.5682682299991342, 43.14958040911493242 ) ) ;
#361 = EDGE_CURVE ( 'NONE', #10268, #41981, #3126, .T. ) ;
#362 = DIRECTION ( 'NONE',  ( 0.000000000000000000, 0.000000000000000000, 1.000000000000000000 ) ) ;
#363 = VECTOR ( 'NONE', #4205, 1000.000000000000000 ) ;
#364 = ADVANCED_FACE ( 'NONE', ( #3690, #17069 ), #21009, .F. ) ;
#365 = EDGE_LOOP ( 'NONE', ( #40363, #21648, #12484, #22363 ) ) ;
#366 = AXIS2_PLACEMENT_3D ( 'NONE', #25494, #18321, #32020 ) ;
#367 = VECTOR ( 'NONE', #17531, 1000.000000000000000 ) ;
#368 = ORIENTED_EDGE ( 'NONE', *, *, #3508, .T. ) ;
#369 = LINE ( 'NONE', #17453, #16327 ) ;
#370 = ORIENTED_EDGE ( 'NONE', *, *, #15483, .F. ) ;
#371 = CARTESIAN_POINT ( 'NONE',  ( -4.000000000000000000, -2.309401076758512694, -5.000000000000000000 ) ) ;
#372 = CIRCLE ( 'NONE', #37296, 58.99999999999999289 ) ;
#373 = CARTESIAN_POINT ( 'NONE',  ( 18.00000000000000355, -36.34385289850569478, -29.77717097092114429 ) ) ;
#374 = DIRECTION ( 'NONE',  ( 0.000000000000000000, 0.000000000000000000, -1.000000000000000000 ) ) ;
#375 = AXIS2_PLACEMENT_3D ( 'NONE', #42673, #13475, #23302 ) ;
#376 = AXIS2_PLACEMENT_3D ( 'NONE', #13765, #3889, #24670 ) ;
#377 = FACE_OUTER_BOUND ( 'NONE', #25940, .T. ) ;
#378 = AXIS2_PLACEMENT_3D ( 'NONE', #10736, #14239, #7672 ) ;
#379 = CARTESIAN_POINT ( 'NONE',  ( 17.99999999999999645, 0.000000000000000000, 0.000000000000000000 ) ) ;
#380 = ORIENTED_EDGE ( 'NONE', *, *, #4869, .F. ) ;
#382 = DIRECTION ( 'NONE',  ( 1.000000000000000000, -0.000000000000000000, -0.000000000000000000 ) ) ;
#381 = DIRECTION ( 'NONE',  ( 0.000000000000000000, 0.000000000000000000, 1.000000000000000000 ) ) ;
#384 = VERTEX_POINT ( 'NONE', #3914 ) ;
#383 = AXIS2_PLACEMENT_3D ( 'NONE', #12644, #12853, #30723 ) ;
#385 = DIRECTION ( 'NONE',  ( 1.000000000000000000, 0.000000000000000000, 0.000000000000000000 ) ) ;
#387 = ADVANCED_FACE ( 'NONE', ( #37740 ), #10941, .T. ) ;
#386 = CARTESIAN_POINT ( 'NONE',  ( -20.07939870814534089, 31.00000000000000355, -2.638545259751242877 ) ) ;
#388 = ORIENTED_EDGE ( 'NONE', *, *, #3051, .T. ) ;
#389 = DIRECTION ( 'NONE',  ( -1.000000000000000000, 0.000000000000000000, 0.000000000000000000 ) ) ;
#390 = ADVANCED_FACE ( 'NONE', ( #24276 ), #4353, .F. ) ;
#391 = CARTESIAN_POINT ( 'NONE',  ( 0.000000000000000000, 0.7408941433508176022, -1.199999999999999956 ) ) ;
#392 = CARTESIAN_POINT ( 'NONE',  ( 17.99999999999999645, 0.000000000000000000, 0.000000000000000000 ) ) ;
#393 = CARTESIAN_POINT ( 'NONE',  ( -9.469526743414824921, 31.00000000000000355, -71.82433816204535049 ) ) ;
#395 = ORIENTED_EDGE ( 'NONE', *, *, #18780, .F. ) ;
#394 = AXIS2_PLACEMENT_3D ( 'NONE', #20858, #497, #13633 ) ;
#396 = CARTESIAN_POINT ( 'NONE',  ( 31.88898475263450649, 31.00000000000000355, 36.48290236124523744 ) ) ;
#397 = CARTESIAN_POINT ( 'NONE',  ( 63.16980243745005907, 39.99999999999999289, -55.41789732285823078 ) ) ;
#398 = AXIS2_PLACEMENT_3D ( 'NONE', #38815, #39023, #34911 ) ;
#399 = CIRCLE ( 'NONE', #24866, 2.649999999999985700 ) ;
#400 = EDGE_CURVE ( 'NONE', #17108, #12372, #25504, .T. ) ;
#401 = EDGE_CURVE ( 'NONE', #35963, #19047, #6638, .T. ) ;
#402 = CARTESIAN_POINT ( 'NONE',  ( 0.000000000000000000, 0.000000000000000000, 0.000000000000000000 ) ) ;
#403 = AXIS2_PLACEMENT_3D ( 'NONE', #31124, #18726, #31983 ) ;
#404 = DIRECTION ( 'NONE',  ( 0.000000000000000000, 0.9911528310040075285, -0.1327255272837188915 ) ) ;
#405 = AXIS2_PLACEMENT_3D ( 'NONE', #124, #9763, #3187 ) ;
#406 = CIRCLE ( 'NONE', #17897, 20.00000000000001066 ) ;
#407 = EDGE_LOOP ( 'NONE', ( #6794, #8753, #34477, #34634 ) ) ;
#408 = CARTESIAN_POINT ( 'NONE',  ( 0.000000000000000000, 31.80866420683990725, 16.59709355804141495 ) ) ;
#409 = CYLINDRICAL_SURFACE ( 'NONE', #39727, 116.0000000000000000 ) ;
#410 = CIRCLE ( 'NONE', #16542, 120.5010000000000474 ) ;
#411 = EDGE_CURVE ( 'NONE', #1566, #6181, #12925, .T. ) ;
#412 = ORIENTED_EDGE ( 'NONE', *, *, #27431, .T. ) ;
#413 = CARTESIAN_POINT ( 'NONE',  ( 51.69409438402072965, 40.00000000000000000, -17.56033928829605273 ) ) ;
#414 = DIRECTION ( 'NONE',  ( 0.000000000000000000, 0.000000000000000000, -1.000000000000000000 ) ) ;
#415 = CARTESIAN_POINT ( 'NONE',  ( 17.99999999999999645, 92.25992191227497585, -77.51514567967304004 ) ) ;
#416 = VERTEX_POINT ( 'NONE', #20792 ) ;
#417 = ADVANCED_FACE ( 'NONE', ( #17508 ), #30784, .F. ) ;
#418 = DIRECTION ( 'NONE',  ( 1.000000000000000000, 0.000000000000000000, 0.000000000000000000 ) ) ;
#419 = DIRECTION ( 'NONE',  ( 0.000000000000000000, 0.000000000000000000, 1.000000000000000000 ) ) ;
#420 = ORIENTED_EDGE ( 'NONE', *, *, #41596, .F. ) ;
#421 = DIRECTION ( 'NONE',  ( -1.000000000000000000, -0.000000000000000000, 0.000000000000000000 ) ) ;
#422 = ORIENTED_EDGE ( 'NONE', *, *, #41036, .F. ) ;
#423 = CARTESIAN_POINT ( 'NONE',  ( 9.000000000000001776, -112.5220807139882311, -28.19186676675956704 ) ) ;
#424 = ORIENTED_EDGE ( 'NONE', *, *, #31392, .T. ) ;
#425 = DIRECTION ( 'NONE',  ( 0.000000000000000000, 0.000000000000000000, 1.000000000000000000 ) ) ;
#426 = CARTESIAN_POINT ( 'NONE',  ( -73.90312034494817794, 31.00000000000000711, -56.84521418461152109 ) ) ;
#427 = ORIENTED_EDGE ( 'NONE', *, *, #25866, .T. ) ;
#428 = DIRECTION ( 'NONE',  ( 0.000000000000000000, 0.000000000000000000, 1.000000000000000000 ) ) ;
#429 = AXIS2_PLACEMENT_3D ( 'NONE', #36616, #10454, #9000 ) ;
#430 = DIRECTION ( 'NONE',  ( -1.000000000000000000, -0.000000000000000000, 0.000000000000000000 ) ) ;
#431 = AXIS2_PLACEMENT_3D ( 'NONE', #12045, #31659, #11830 ) ;
#432 = CARTESIAN_POINT ( 'NONE',  ( 17.99999999999999645, 104.2166695095712470, 60.49278301857841456 ) ) ;
#433 = VERTEX_POINT ( 'NONE', #7858 ) ;
#434 = VECTOR ( 'NONE', #34383, 1000.000000000000000 ) ;
#435 = CARTESIAN_POINT ( 'NONE',  ( 17.99999999999999645, 105.3681574666269256, -38.54638589714782881 ) ) ;
#436 = CIRCLE ( 'NONE', #24900, 59.00000000000000000 ) ;
#437 = DIRECTION ( 'NONE',  ( 0.000000000000000000, -0.9822872507286903865, 0.1873813145857150253 ) ) ;
#438 = ADVANCED_FACE ( 'NONE', ( #21215 ), #30995, .F. ) ;
#439 = ADVANCED_FACE ( 'NONE', ( #21867 ), #29028, .F. ) ;
#441 = CARTESIAN_POINT ( 'NONE',  ( 18.00000000000000355, 46.19362259308835661, 8.585149169758654608 ) ) ;
#440 = CARTESIAN_POINT ( 'NONE',  ( -101.9145453900124068, 31.00000000000000355, -1.407535261550473704 ) ) ;
#442 = STYLED_ITEM ( 'NONE', ( #20930 ), #28802 ) ;
#443 = ADVANCED_FACE ( 'NONE', ( #12453 ), #25139, .F. ) ;
#444 = EDGE_CURVE ( 'NONE', #11655, #6621, #32347, .T. ) ;
#445 = CARTESIAN_POINT ( 'NONE',  ( 0.000000000000000000, 69.90696807222620635, -98.15042952503443985 ) ) ;
#446 = ORIENTED_EDGE ( 'NONE', *, *, #31372, .T. ) ;
#447 = DIRECTION ( 'NONE',  ( 0.1004768330516124658, 1.354163300868569232E-16, -0.9949393981644903961 ) ) ;
#448 = AXIS2_PLACEMENT_3D ( 'NONE', #41556, #21331, #31328 ) ;
#449 = CARTESIAN_POINT ( 'NONE',  ( -10.00000000000000000, 0.000000000000000000, 0.000000000000000000 ) ) ;
#450 = CARTESIAN_POINT ( 'NONE',  ( -39.89583333501392559, 31.00000000000000355, 2.617993869485681468 ) ) ;
#451 = ORIENTED_EDGE ( 'NONE', *, *, #9647, .F. ) ;
#452 = CARTESIAN_POINT ( 'NONE',  ( 17.99999999999999645, 0.000000000000000000, 0.000000000000000000 ) ) ;
#453 = AXIS2_PLACEMENT_3D ( 'NONE', #35646, #23040, #19334 ) ;
#454 = CARTESIAN_POINT ( 'NONE',  ( 17.99999999999999645, -46.12538073176424547, 111.3235835452210267 ) ) ;
#455 = ORIENTED_EDGE ( 'NONE', *, *, #22771, .T. ) ;
#456 = CARTESIAN_POINT ( 'NONE',  ( 17.99999999999999645, 0.000000000000000000, 0.000000000000000000 ) ) ;
#457 = CARTESIAN_POINT ( 'NONE',  ( -16.75480014238754478, 40.00000000000000000, -49.32177912249007790 ) ) ;
#458 = CARTESIAN_POINT ( 'NONE',  ( -37.13421060599359436, 40.00000000000000000, -21.52932707635456211 ) ) ;
#459 = EDGE_LOOP ( 'NONE', ( #38424, #13249, #34753, #39465 ) ) ;
#460 = FACE_OUTER_BOUND ( 'NONE', #18537, .T. ) ;
#461 = DIRECTION ( 'NONE',  ( -1.000000000000000000, -0.000000000000000000, -0.000000000000000000 ) ) ;
#462 = CIRCLE ( 'NONE', #22115, 13.60000000000000142 ) ;
#463 = CYLINDRICAL_SURFACE ( 'NONE', #7099, 20.00000000000000711 ) ;
#464 = CIRCLE ( 'NONE', #39460, 59.00000000000000000 ) ;
#465 = ORIENTED_EDGE ( 'NONE', *, *, #10281, .F. ) ;
#466 = CARTESIAN_POINT ( 'NONE',  ( -12.50349052776452297, 40.00000000000000000, 25.37591446456323041 ) ) ;
#467 = ORIENTED_EDGE ( 'NONE', *, *, #36751, .F. ) ;
#468 = DIRECTION ( 'NONE',  ( 0.000000000000000000, 1.000000000000000000, 0.000000000000000000 ) ) ;
#469 = CARTESIAN_POINT ( 'NONE',  ( 4.121423858225410797, -12.61643262889541006, -1.199999999999999956 ) ) ;
#470 = CIRCLE ( 'NONE', #10341, 20.00000000000001421 ) ;
#471 = ORIENTED_EDGE ( 'NONE', *, *, #11051, .F. ) ;
#472 = DIRECTION ( 'NONE',  ( 0.000000000000000000, 0.000000000000000000, 1.000000000000000000 ) ) ;
#473 = LINE ( 'NONE', #3521, #19907 ) ;
#474 = ORIENTED_EDGE ( 'NONE', *, *, #37927, .T. ) ;
#475 = DIRECTION ( 'NONE',  ( -1.000000000000000000, -0.000000000000000000, 0.000000000000000000 ) ) ;
#476 = CIRCLE ( 'NONE', #10987, 20.00000000000000355 ) ;
#477 = ORIENTED_EDGE ( 'NONE', *, *, #12046, .F. ) ;
#478 = DIRECTION ( 'NONE',  ( -1.000000000000000000, -0.000000000000000000, -0.000000000000000000 ) ) ;
#479 = AXIS2_PLACEMENT_3D ( 'NONE', #32329, #9842, #19919 ) ;
#480 = ORIENTED_EDGE ( 'NONE', *, *, #30811, .T. ) ;
#482 = EDGE_LOOP ( 'NONE', ( #35569, #28830, #27446, #17028 ) ) ;
#481 = DIRECTION ( 'NONE',  ( 1.000000000000000000, 0.000000000000000000, 0.000000000000000000 ) ) ;
#483 = CIRCLE ( 'NONE', #29083, 47.49899999999998812 ) ;
#484 = CARTESIAN_POINT ( 'NONE',  ( -59.63693792270941429, 31.00000000000000711, 15.87187584493272929 ) ) ;
#485 = ORIENTED_EDGE ( 'NONE', *, *, #20784, .T. ) ;
#486 = DIRECTION ( 'NONE',  ( 1.000000000000000000, 0.000000000000000000, 0.000000000000000000 ) ) ;
#487 = ORIENTED_EDGE ( 'NONE', *, *, #21055, .T. ) ;
#488 = FACE_OUTER_BOUND ( 'NONE', #34162, .T. ) ;
#489 = PRODUCT_DEFINITION_SHAPE ( 'NONE', 'NONE',  #43188 ) ;
#490 = ORIENTED_EDGE ( 'NONE', *, *, #30914, .T. ) ;
#491 = CARTESIAN_POINT ( 'NONE',  ( -82.09281090897877675, 40.00000000000000711, -5.486092462564050365 ) ) ;
#492 = CIRCLE ( 'NONE', #22825, 59.00000000000000000 ) ;
#494 = CARTESIAN_POINT ( 'NONE',  ( 9.000000000000001776, 47.32430374665931794, 21.55018039121544504 ) ) ;
#493 = DIRECTION ( 'NONE',  ( 0.000000000000000000, -0.1062934856473723849, 0.9943348002101364269 ) ) ;
#495 = ADVANCED_FACE ( 'NONE', ( #34696 ), #4808, .T. ) ;
#496 = EDGE_CURVE ( 'NONE', #16818, #9730, #22290, .T. ) ;
#497 = DIRECTION ( 'NONE',  ( -1.000000000000000000, -0.000000000000000000, -0.000000000000000000 ) ) ;
#498 = EDGE_LOOP ( 'NONE', ( #22590, #14533, #15559, #34141 ) ) ;
#499 = DIRECTION ( 'NONE',  ( 1.000000000000000000, 0.000000000000000000, 0.000000000000000000 ) ) ;
#500 = AXIS2_PLACEMENT_3D ( 'NONE', #1335, #20821, #14680 ) ;
#501 = VERTEX_POINT ( 'NONE', #18171 ) ;
#502 = AXIS2_PLACEMENT_3D ( 'NONE', #28642, #35156, #28215 ) ;
#503 = PRESENTATION_STYLE_ASSIGNMENT (( #8148 ) ) ;
#504 = ADVANCED_FACE ( 'NONE', ( #22074 ), #11814, .F. ) ;
#505 = VECTOR ( 'NONE', #4362, 1000.000000000000000 ) ;
#506 = CARTESIAN_POINT ( 'NONE',  ( 8.999999999999998224, -97.97378550988267421, 62.10585602713726416 ) ) ;
#507 = AXIS2_PLACEMENT_3D ( 'NONE', #19360, #40003, #6868 ) ;
#508 = VERTEX_POINT ( 'NONE', #34910 ) ;
#509 = CARTESIAN_POINT ( 'NONE',  ( 17.99999999999999645, 21.55123232222474172, 118.5581519187672654 ) ) ;
#510 = VECTOR ( 'NONE', #27183, 1000.000000000000000 ) ;
#511 = CARTESIAN_POINT ( 'NONE',  ( -60.37409795221152109, 31.00000000000000711, -68.82020352599361956 ) ) ;
#512 = CARTESIAN_POINT ( 'NONE',  ( -0.1756481739660520902, 4.720212674038980261, -3.469390959564065291 ) ) ;
#513 = ORIENTED_EDGE ( 'NONE', *, *, #20207, .F. ) ;
#514 = CARTESIAN_POINT ( 'NONE',  ( 17.99999999999999645, 51.98489025774451733, -108.7109110710156159 ) ) ;
#515 =( REPRESENTATION_RELATIONSHIP ('NONE','NONE', #330, #40225 ) REPRESENTATION_RELATIONSHIP_WITH_TRANSFORMATION ( #6103 )SHAPE_REPRESENTATION_RELATIONSHIP( ) );
#516 = AXIS2_PLACEMENT_3D ( 'NONE', #26547, #20038, #33303 ) ;
#517 = EDGE_CURVE ( 'NONE', #5078, #15357, #24037, .T. ) ;
#518 = ORIENTED_EDGE ( 'NONE', *, *, #39998, .F. ) ;
#519 = FACE_OUTER_BOUND ( 'NONE', #1708, .T. ) ;
#520 = DIRECTION ( 'NONE',  ( -1.000000000000000000, 0.000000000000000000, 0.000000000000000000 ) ) ;
#521 = SURFACE_STYLE_USAGE ( .BOTH. , #20426 ) ;
#522 = CARTESIAN_POINT ( 'NONE',  ( 0.000000000000000000, -11.90021268425586953, 45.45261810511210143 ) ) ;
#523 = ORIENTED_EDGE ( 'NONE', *, *, #10844, .T. ) ;
#524 = CARTESIAN_POINT ( 'NONE',  ( 8.999999999999998224, -86.84764344322910290, -76.89919913989835720 ) ) ;
#525 = ORIENTED_EDGE ( 'NONE', *, *, #4876, .F. ) ;
#526 = DIRECTION ( 'NONE',  ( 0.000000000000000000, 0.000000000000000000, 1.000000000000000000 ) ) ;
#527 = AXIS2_PLACEMENT_3D ( 'NONE', #22171, #5544, #35427 ) ;
#528 = DIRECTION ( 'NONE',  ( 0.000000000000000000, -0.9996456111234528485, 0.02662052143776447166 ) ) ;
#529 = DIRECTION ( 'NONE',  ( 1.000000000000000000, 0.000000000000000000, 0.000000000000000000 ) ) ;
#530 = ORIENTED_EDGE ( 'NONE', *, *, #40112, .T. ) ;
#531 = ADVANCED_FACE ( 'NONE', ( #5457 ), #18378, .T. ) ;
#532 = EDGE_LOOP ( 'NONE', ( #15360, #37430, #26856, #20407 ) ) ;
#533 = CARTESIAN_POINT ( 'NONE',  ( 18.00000000000000355, -46.77034588191318676, 22.72740077717213580 ) ) ;
#534 = LINE ( 'NONE', #37619, #35342 ) ;
#535 = VECTOR ( 'NONE', #20780, 1000.000000000000000 ) ;
#536 = DIRECTION ( 'NONE',  ( 0.000000000000000000, 0.000000000000000000, 1.000000000000000000 ) ) ;
#537 = CIRCLE ( 'NONE', #20124, 58.99999999999999289 ) ;
#538 = AXIS2_PLACEMENT_3D ( 'NONE', #40650, #40443, #37179 ) ;
#540 = ORIENTED_EDGE ( 'NONE', *, *, #2625, .F. ) ;
#539 = DIRECTION ( 'NONE',  ( 0.000000000000000000, 0.000000000000000000, -1.000000000000000000 ) ) ;
#541 = CARTESIAN_POINT ( 'NONE',  ( 2.319640971205256363, 31.00000000000000355, -34.59922639972668179 ) ) ;
#542 = CARTESIAN_POINT ( 'NONE',  ( 0.000000000000000000, -119.7318547011702634, 13.59315897125686057 ) ) ;
#543 = AXIS2_PLACEMENT_3D ( 'NONE', #13775, #29697, #16847 ) ;
#545 = EDGE_LOOP ( 'NONE', ( #30373, #28462, #5069, #8099 ) ) ;
#544 = DIRECTION ( 'NONE',  ( -1.000000000000000000, 0.000000000000000000, -0.000000000000000000 ) ) ;
#546 = ORIENTED_EDGE ( 'NONE', *, *, #32103, .F. ) ;
#547 = FACE_BOUND ( 'NONE', #22047, .T. ) ;
#548 = CARTESIAN_POINT ( 'NONE',  ( -6.590854309045714565, 40.00000000000000000, 49.37518673228670707 ) ) ;
#549 = CIRCLE ( 'NONE', #35355, 47.49900000000000944 ) ;
#550 = CARTESIAN_POINT ( 'NONE',  ( 9.000000000000001776, 37.07968990261626629, -109.9140418541953750 ) ) ;
#551 = EDGE_CURVE ( 'NONE', #38409, #5751, #33026, .T. ) ;
#552 = CARTESIAN_POINT ( 'NONE',  ( 8.999999999999998224, -91.65951123222531294, 71.09524597798055368 ) ) ;
#553 = VERTEX_POINT ( 'NONE', #42298 ) ;
#554 = CARTESIAN_POINT ( 'NONE',  ( 0.000000000000000000, -42.03146605346771025, -22.12489237027361000 ) ) ;
#555 = ORIENTED_EDGE ( 'NONE', *, *, #25691, .F. ) ;
#556 = DIRECTION ( 'NONE',  ( 0.000000000000000000, 0.000000000000000000, 1.000000000000000000 ) ) ;
#557 = CARTESIAN_POINT ( 'NONE',  ( 0.000000000000000000, 104.0201923570382405, -51.34003878070953419 ) ) ;
#558 = CARTESIAN_POINT ( 'NONE',  ( 40.56819808336118882, 31.00000000000000355, -35.59309480518532354 ) ) ;
#559 = VECTOR ( 'NONE', #25999, 1000.000000000000000 ) ;
#560 = CARTESIAN_POINT ( 'NONE',  ( -10.00000000000000000, 0.000000000000000000, 0.000000000000000000 ) ) ;
#561 = CIRCLE ( 'NONE', #25023, 12.49999999999993427 ) ;
#562 = ORIENTED_EDGE ( 'NONE', *, *, #6863, .F. ) ;
#563 = ADVANCED_FACE ( 'NONE', ( #31437 ), #1736, .T. ) ;
#564 = EDGE_CURVE ( 'NONE', #21757, #23443, #22642, .T. ) ;
#565 = CARTESIAN_POINT ( 'NONE',  ( 8.999999999999998224, 104.0201923570375300, 51.34003878071097660 ) ) ;
#566 = VERTEX_POINT ( 'NONE', #8945 ) ;
#567 = CARTESIAN_POINT ( 'NONE',  ( 5.935205493550105516, 40.00000000000000000, -22.18504493031268865 ) ) ;
#568 = CIRCLE ( 'NONE', #31967, 59.00000000000000711 ) ;
#569 = EDGE_CURVE ( 'NONE', #10925, #32031, #2158, .T. ) ;
#570 = ORIENTED_EDGE ( 'NONE', *, *, #29147, .T. ) ;
#571 = LINE ( 'NONE', #20474, #42329 ) ;
#572 = DIRECTION ( 'NONE',  ( 1.000000000000000000, 0.000000000000000000, 0.000000000000000000 ) ) ;
#573 = CARTESIAN_POINT ( 'NONE',  ( 61.98103557012429121, 31.00000000000000000, 47.69015029125303329 ) ) ;
#574 = CARTESIAN_POINT ( 'NONE',  ( 73.52353481979008620, 39.99999999999999289, 25.08131146963209090 ) ) ;
#575 = DIRECTION ( 'NONE',  ( -1.000000000000000000, 0.000000000000000000, -0.000000000000000000 ) ) ;
#576 = ORIENTED_EDGE ( 'NONE', *, *, #13519, .F. ) ;
#577 = DIRECTION ( 'NONE',  ( 0.000000000000000000, 0.000000000000000000, 1.000000000000000000 ) ) ;
#578 = ORIENTED_EDGE ( 'NONE', *, *, #683, .T. ) ;
#579 = CYLINDRICAL_SURFACE ( 'NONE', #23483, 58.99999999999999289 ) ;
#580 = CARTESIAN_POINT ( 'NONE',  ( 0.000000000000000000, -71.21168426767167148, 86.70160608319299911 ) ) ;
#582 = ORIENTED_EDGE ( 'NONE', *, *, #18176, .T. ) ;
#581 = DIRECTION ( 'NONE',  ( 0.000000000000000000, 1.000000000000000000, 0.000000000000000000 ) ) ;
#583 = CYLINDRICAL_SURFACE ( 'NONE', #5170, 120.5010000000000190 ) ;
#584 = ORIENTED_EDGE ( 'NONE', *, *, #31908, .F. ) ;
#585 = FACE_OUTER_BOUND ( 'NONE', #22797, .T. ) ;
#586 = CARTESIAN_POINT ( 'NONE',  ( 84.89583333414414312, 39.99999999999999289, -5.563236982362012029 ) ) ;
#587 = DIRECTION ( 'NONE',  ( -1.000000000000000000, 0.000000000000000000, 0.000000000000000000 ) ) ;
#588 = EDGE_CURVE ( 'NONE', #36837, #2925, #6541, .T. ) ;
#589 = ORIENTED_EDGE ( 'NONE', *, *, #18866, .T. ) ;
#590 = DIRECTION ( 'NONE',  ( 1.000000000000000000, 1.836909530733573776E-16, 0.000000000000000000 ) ) ;
#591 = CARTESIAN_POINT ( 'NONE',  ( -105.9879088449591933, 31.00000000000000355, -0.3807199291576673361 ) ) ;
#592 = ORIENTED_EDGE ( 'NONE', *, *, #38847, .F. ) ;
#593 = AXIS2_PLACEMENT_3D ( 'NONE', #42590, #9443, #2867 ) ;
#594 = EDGE_LOOP ( 'NONE', ( #9108, #20591, #34334, #3466 ) ) ;
#595 = DIRECTION ( 'NONE',  ( -1.000000000000000000, 0.000000000000000000, -0.000000000000000000 ) ) ;
#596 = VERTEX_POINT ( 'NONE', #38814 ) ;
#597 = CYLINDRICAL_SURFACE ( 'NONE', #2515, 51.99999999999999289 ) ;
#598 = LINE ( 'NONE', #13951, #7008 ) ;
#599 = DIRECTION ( 'NONE',  ( -1.000000000000000000, 0.000000000000000000, 0.000000000000000000 ) ) ;
#600 = DIRECTION ( 'NONE',  ( 0.000000000000000000, 1.000000000000000000, -1.060184893785364939E-15 ) ) ;
#601 = CARTESIAN_POINT ( 'NONE',  ( 0.000000000000000000, 0.000000000000000000, 0.000000000000000000 ) ) ;
#602 = ORIENTED_EDGE ( 'NONE', *, *, #42111, .T. ) ;
#604 = DIRECTION ( 'NONE',  ( -0.000000000000000000, -0.000000000000000000, -1.000000000000000000 ) ) ;
#603 = CARTESIAN_POINT ( 'NONE',  ( -10.00000000000000000, 0.000000000000000000, 0.000000000000000000 ) ) ;
#605 = EDGE_CURVE ( 'NONE', #28014, #24263, #266, .T. ) ;
#606 = VERTEX_POINT ( 'NONE', #25767 ) ;
#607 = CARTESIAN_POINT ( 'NONE',  ( 17.99999999999999645, 110.3490479609632615, 38.71798610214565173 ) ) ;
#608 = CARTESIAN_POINT ( 'NONE',  ( -10.31048697494744815, 31.00000000000000355, -30.34325702988586215 ) ) ;
#609 = ORIENTED_EDGE ( 'NONE', *, *, #444, .T. ) ;
#610 = PLANE ( 'NONE',  #16963 ) ;
#611 = CARTESIAN_POINT ( 'NONE',  ( 0.000000000000000000, 62.45178862086345362, -93.20969140437443912 ) ) ;
#612 = EDGE_CURVE ( 'NONE', #31034, #38131, #30956, .T. ) ;
#613 = CARTESIAN_POINT ( 'NONE',  ( 0.000000000000000000, 0.000000000000000000, 0.000000000000000000 ) ) ;
#614 = CARTESIAN_POINT ( 'NONE',  ( -68.16583574478268304, 31.00000000000000711, -18.25112749842637427 ) ) ;
#615 = ORIENTED_EDGE ( 'NONE', *, *, #5876, .F. ) ;
#616 = AXIS2_PLACEMENT_3D ( 'NONE', #33760, #3842, #17229 ) ;
#617 = CARTESIAN_POINT ( 'NONE',  ( -13.02511903071888355, 31.00000000000000355, 48.29538318457647961 ) ) ;
#618 = CARTESIAN_POINT ( 'NONE',  ( -79.89583333417640176, 40.00000000000000711, 5.235987747608064957 ) ) ;
#619 = FACE_OUTER_BOUND ( 'NONE', #3367, .T. ) ;
#620 = DIRECTION ( 'NONE',  ( -1.000000000000000000, -0.000000000000000000, 0.000000000000000000 ) ) ;
#621 = CYLINDRICAL_SURFACE ( 'NONE', #22645, 25.00000000000000000 ) ;
#623 = ORIENTED_EDGE ( 'NONE', *, *, #22304, .T. ) ;
#622 = B_SPLINE_CURVE_WITH_KNOTS ( 'NONE', 3,
 ( #39665, #43157, #13743, #26398, #40087 ),
 .UNSPECIFIED., .F., .F.,
 ( 4, 1, 4 ),
 ( 0.000000000000000000, 0.002309401076758505790, 0.004618802153517011580 ),
 .UNSPECIFIED. ) ;
#624 = DIRECTION ( 'NONE',  ( 1.000000000000000000, 0.000000000000000000, 0.000000000000000000 ) ) ;
#625 = CARTESIAN_POINT ( 'NONE',  ( -10.00000000000000000, 0.000000000000000000, 0.000000000000000000 ) ) ;
#626 = ORIENTED_EDGE ( 'NONE', *, *, #10787, .F. ) ;
#627 = CARTESIAN_POINT ( 'NONE',  ( 35.44578089419255917, 40.00000000000000000, -40.42088417236866604 ) ) ;
#628 = DIRECTION ( 'NONE',  ( -1.000000000000000000, 0.000000000000000000, 0.000000000000000000 ) ) ;
#630 = EDGE_CURVE ( 'NONE', #32233, #22705, #22711, .T. ) ;
#629 = CARTESIAN_POINT ( 'NONE',  ( 17.99999999999999645, 3.996885678774600326, -120.4346956066681713 ) ) ;
#631 = VERTEX_POINT ( 'NONE', #9583 ) ;
#632 = EDGE_CURVE ( 'NONE', #15962, #12068, #5869, .T. ) ;
#633 = CARTESIAN_POINT ( 'NONE',  ( 17.99999999999999645, 0.000000000000000000, 0.000000000000000000 ) ) ;
#634 = DIRECTION ( 'NONE',  ( 0.000000000000000000, 0.000000000000000000, 1.000000000000000000 ) ) ;
#635 = ORIENTED_EDGE ( 'NONE', *, *, #17742, .T. ) ;
#636 = CARTESIAN_POINT ( 'NONE',  ( 0.000000000000000000, -53.40478689619801145, 108.0204598100363711 ) ) ;
#637 = VERTEX_POINT ( 'NONE', #6729 ) ;
#638 = DIRECTION ( 'NONE',  ( 0.000000000000000000, 0.000000000000000000, 1.000000000000000000 ) ) ;
#640 = VERTEX_POINT ( 'NONE', #32493 ) ;
#639 = CIRCLE ( 'NONE', #2719, 36.00000000000000000 ) ;
#641 = FACE_OUTER_BOUND ( 'NONE', #29128, .T. ) ;
#642 = LINE ( 'NONE', #17948, #38766 ) ;
#643 = ORIENTED_EDGE ( 'NONE', *, *, #1416, .F. ) ;
#644 = VECTOR ( 'NONE', #35434, 1000.000000000000000 ) ;
#645 = DIRECTION ( 'NONE',  ( -1.000000000000000000, 0.000000000000000000, -0.000000000000000000 ) ) ;
#646 = DIRECTION ( 'NONE',  ( 1.000000000000000000, -3.009274222672345096E-17, 0.000000000000000000 ) ) ;
#647 = CIRCLE ( 'NONE', #38965, 59.00000000000000711 ) ;
#648 = ORIENTED_EDGE ( 'NONE', *, *, #24910, .T. ) ;
#649 = DIRECTION ( 'NONE',  ( 0.000000000000000000, 0.000000000000000000, 1.000000000000000000 ) ) ;
#650 = EDGE_CURVE ( 'NONE', #9771, #35135, #17755, .T. ) ;
#651 = ADVANCED_FACE ( 'NONE', ( #42509 ), #30274, .T. ) ;
#652 = CARTESIAN_POINT ( 'NONE',  ( 17.99999999999999645, -2.007101075700182591, 31.43498920425968279 ) ) ;
#653 = CYLINDRICAL_SURFACE ( 'NONE', #7831, 20.00000000000000355 ) ;
#654 = DIRECTION ( 'NONE',  ( -1.000000000000000000, 0.000000000000000000, 0.000000000000000000 ) ) ;
#655 = ORIENTED_EDGE ( 'NONE', *, *, #12968, .T. ) ;
#656 = CARTESIAN_POINT ( 'NONE',  ( -2.250288493433258742E-15, 1.999999999999996669, -150.5000000000000284 ) ) ;
#657 = EDGE_CURVE ( 'NONE', #1834, #41377, #28882, .T. ) ;
#658 = DIRECTION ( 'NONE',  ( 1.000000000000000000, -0.000000000000000000, -0.000000000000000000 ) ) ;
#659 = CARTESIAN_POINT ( 'NONE',  ( -19.20510714644778361, 31.00000000000000355, 33.27066566623395261 ) ) ;
#660 = ORIENTED_EDGE ( 'NONE', *, *, #6365, .T. ) ;
#661 = CARTESIAN_POINT ( 'NONE',  ( 17.99999999999999645, 110.3490479609632615, -20.28201389785435182 ) ) ;
#662 = EDGE_CURVE ( 'NONE', #4953, #16239, #15652, .T. ) ;
#663 = DIRECTION ( 'NONE',  ( -1.000000000000000000, -0.000000000000000000, -0.000000000000000000 ) ) ;
#664 = ORIENTED_EDGE ( 'NONE', *, *, #26225, .F. ) ;
#665 = CARTESIAN_POINT ( 'NONE',  ( 0.000000000000000000, 112.5220807139887853, -28.19186676675730752 ) ) ;
#666 = CARTESIAN_POINT ( 'NONE',  ( -29.60425243605831724, 40.00000000000000000, 38.59963703562669934 ) ) ;
#667 = CARTESIAN_POINT ( 'NONE',  ( 40.10317558969867946, 40.00000000000000000, -23.06553963618951286 ) ) ;
#668 = AXIS2_PLACEMENT_3D ( 'NONE', #2033, #36049, #15804 ) ;
#669 = AXIS2_PLACEMENT_3D ( 'NONE', #24618, #14789, #11734 ) ;
#670 = ORIENTED_EDGE ( 'NONE', *, *, #7404, .F. ) ;
#671 = DIRECTION ( 'NONE',  ( 3.009274222672345096E-17, 1.000000000000000000, -2.455023325076455345E-18 ) ) ;
#672 = DIRECTION ( 'NONE',  ( -1.000000000000000000, 0.000000000000000000, 0.000000000000000000 ) ) ;
#673 = AXIS2_PLACEMENT_3D ( 'NONE', #23183, #40131, #40354 ) ;
#674 = CARTESIAN_POINT ( 'NONE',  ( -132.0000507999999968, 0.000000000000000000, 0.000000000000000000 ) ) ;
#675 = DIRECTION ( 'NONE',  ( 0.000000000000000000, 0.000000000000000000, 1.000000000000000000 ) ) ;
#676 = ORIENTED_EDGE ( 'NONE', *, *, #42452, .F. ) ;
#677 = CARTESIAN_POINT ( 'NONE',  ( 15.62097837807030842, 40.00000000000000000, -17.81927981957692353 ) ) ;
#678 = ORIENTED_EDGE ( 'NONE', *, *, #20185, .T. ) ;
#679 = DIRECTION ( 'NONE',  ( 0.000000000000000000, 0.000000000000000000, -1.000000000000000000 ) ) ;
#680 = CARTESIAN_POINT ( 'NONE',  ( 18.00000000000000355, 46.87740477351712798, 3.172455868806036694 ) ) ;
#681 = EDGE_CURVE ( 'NONE', #10180, #38227, #28202, .T. ) ;
#682 = ORIENTED_EDGE ( 'NONE', *, *, #5364, .T. ) ;
#683 = EDGE_CURVE ( 'NONE', #23201, #41689, #21250, .T. ) ;
#684 = DIRECTION ( 'NONE',  ( 0.000000000000000000, -0.8993121301712229121, 0.4373073204588476259 ) ) ;
#685 = EDGE_CURVE ( 'NONE', #596, #26693, #23143, .T. ) ;
#686 = EDGE_CURVE ( 'NONE', #51, #7956, #33742, .T. ) ;
#687 = DIRECTION ( 'NONE',  ( -3.009274222672345096E-17, -1.000000000000000000, 2.455023325076454960E-18 ) ) ;
#688 = EDGE_LOOP ( 'NONE', ( #1604, #9388, #4620, #28390 ) ) ;
#689 = CARTESIAN_POINT ( 'NONE',  ( 6.199999999999997513, 18.78000000000008285, 0.000000000000000000 ) ) ;
#690 = ORIENTED_EDGE ( 'NONE', *, *, #18292, .T. ) ;
#691 = DIRECTION ( 'NONE',  ( 0.000000000000000000, 0.000000000000000000, 1.000000000000000000 ) ) ;
#692 = ORIENTED_EDGE ( 'NONE', *, *, #322, .F. ) ;
#694 = ORIENTED_EDGE ( 'NONE', *, *, #24852, .F. ) ;
#693 = FACE_OUTER_BOUND ( 'NONE', #20264, .T. ) ;
#696 = CIRCLE ( 'NONE', #4186, 58.99999999999999289 ) ;
#695 = CARTESIAN_POINT ( 'NONE',  ( 4.437437895627577511, 31.00000000000000355, 69.40004907510417809 ) ) ;
#697 = ORIENTED_EDGE ( 'NONE', *, *, #24466, .T. ) ;
#698 = CARTESIAN_POINT ( 'NONE',  ( 17.99999999999999645, 87.92975456462900752, 69.68953103478187927 ) ) ;
#699 = ORIENTED_EDGE ( 'NONE', *, *, #10056, .T. ) ;
#700 = DIRECTION ( 'NONE',  ( 0.000000000000000000, 0.000000000000000000, 1.000000000000000000 ) ) ;
#701 = ORIENTED_EDGE ( 'NONE', *, *, #14583, .F. ) ;
#702 = CARTESIAN_POINT ( 'NONE',  ( -6.060882879309179572, 40.00000000000000000, -94.40013096063921694 ) ) ;
#703 = CIRCLE ( 'NONE', #5586, 120.5010000000000332 ) ;
#704 = AXIS2_PLACEMENT_3D ( 'NONE', #17398, #27400, #24586 ) ;
#705 = TOROIDAL_SURFACE ( 'NONE', #25164, 11.08000000000000007, 0.07999999999999934941 ) ;
#707 = DIRECTION ( 'NONE',  ( 0.000000000000000000, 0.000000000000000000, -1.000000000000000000 ) ) ;
#706 = DIRECTION ( 'NONE',  ( -1.000000000000000000, -0.000000000000000000, -0.000000000000000000 ) ) ;
#708 = DIRECTION ( 'NONE',  ( -1.000000000000000000, -0.000000000000000000, -0.000000000000000000 ) ) ;
#709 = CARTESIAN_POINT ( 'NONE',  ( 17.99999999999999645, 0.000000000000000000, 0.000000000000000000 ) ) ;
#710 = VERTEX_POINT ( 'NONE', #16148 ) ;
#711 =( NAMED_UNIT ( * ) SI_UNIT ( $, .STERADIAN. ) SOLID_ANGLE_UNIT ( ) );
#712 = EDGE_CURVE ( 'NONE', #40198, #14972, #29447, .T. ) ;
#713 = DIRECTION ( 'NONE',  ( 1.000000000000000000, 0.000000000000000000, 0.000000000000000000 ) ) ;
#714 = VERTEX_POINT ( 'NONE', #33356 ) ;
#715 = CARTESIAN_POINT ( 'NONE',  ( 17.99999999999999645, -98.39501399267994941, 53.91376164787647696 ) ) ;
#716 = CARTESIAN_POINT ( 'NONE',  ( -72.39171112334068425, 31.00000000000000711, -55.52881859171880308 ) ) ;
#717 = EDGE_CURVE ( 'NONE', #31117, #17266, #28240, .T. ) ;
#718 = CARTESIAN_POINT ( 'NONE',  ( 17.99999999999999645, -96.25468616236712194, 72.49500943364458294 ) ) ;
#719 = VERTEX_POINT ( 'NONE', #32704 ) ;
#720 = FACE_OUTER_BOUND ( 'NONE', #18484, .T. ) ;
#721 = ORIENTED_EDGE ( 'NONE', *, *, #30636, .F. ) ;
#722 = CIRCLE ( 'NONE', #25184, 59.00000000000000000 ) ;
#723 = ORIENTED_EDGE ( 'NONE', *, *, #248, .T. ) ;
#724 = DIRECTION ( 'NONE',  ( -1.000000000000000000, 0.000000000000000000, 0.000000000000000000 ) ) ;
#725 = CARTESIAN_POINT ( 'NONE',  ( 17.99999999999999645, -111.2721026680459602, -14.38025178762732104 ) ) ;
#726 = SURFACE_STYLE_FILL_AREA ( #66 ) ;
#727 = CARTESIAN_POINT ( 'NONE',  ( 17.99999999999999645, 106.5605152861902951, 56.26142179985861702 ) ) ;
#728 = CIRCLE ( 'NONE', #30018, 116.0000000000000000 ) ;
#729 = ORIENTED_EDGE ( 'NONE', *, *, #41298, .T. ) ;
#730 = LINE ( 'NONE', #25424, #7530 ) ;
#731 = ORIENTED_EDGE ( 'NONE', *, *, #31759, .T. ) ;
#732 = VECTOR ( 'NONE', #15027, 1000.000000000000000 ) ;
#733 = DIRECTION ( 'NONE',  ( -0.9470131699890044219, 0.000000000000000000, 0.3211947320043981868 ) ) ;
#734 = AXIS2_PLACEMENT_3D ( 'NONE', #32595, #16248, #28912 ) ;
#735 = CYLINDRICAL_SURFACE ( 'NONE', #36721, 59.00000000000000711 ) ;
#736 = EDGE_CURVE ( 'NONE', #17655, #25229, #13311, .T. ) ;
#737 = EDGE_CURVE ( 'NONE', #1458, #13372, #15945, .T. ) ;
#738 = DIRECTION ( 'NONE',  ( 0.000000000000000000, 0.000000000000000000, -1.000000000000000000 ) ) ;
#739 = ORIENTED_EDGE ( 'NONE', *, *, #1316, .F. ) ;
#740 = ORIENTED_EDGE ( 'NONE', *, *, #38677, .F. ) ;
#741 = CARTESIAN_POINT ( 'NONE',  ( 18.00000000000000355, -39.55064067543046491, -25.36340625197400200 ) ) ;
#742 = CARTESIAN_POINT ( 'NONE',  ( 0.000000000000000000, -49.25004636492399612, 16.68630974939742018 ) ) ;
#743 = EDGE_CURVE ( 'NONE', #6489, #1587, #4491, .T. ) ;
#744 = CARTESIAN_POINT ( 'NONE',  ( 4.204115023516791005, -1.660442669500199919, -3.602151381774560068 ) ) ;
#745 = VECTOR ( 'NONE', #33359, 1000.000000000000000 ) ;
#746 = ORIENTED_EDGE ( 'NONE', *, *, #4004, .T. ) ;
#748 = ORIENTED_EDGE ( 'NONE', *, *, #42765, .F. ) ;
#747 = DIRECTION ( 'NONE',  ( 0.000000000000000000, 0.000000000000000000, 1.000000000000000000 ) ) ;
#749 = CARTESIAN_POINT ( 'NONE',  ( -8.786317949316114095, 31.00000000000000355, -33.00646673688142840 ) ) ;
#750 = CYLINDRICAL_SURFACE ( 'NONE', #21678, 51.99999999999999289 ) ;
#751 = EDGE_CURVE ( 'NONE', #27172, #14763, #37265, .T. ) ;
#753 = EDGE_LOOP ( 'NONE', ( #6646, #13684, #10, #35379 ) ) ;
#752 = DIRECTION ( 'NONE',  ( 1.000000000000000000, 0.000000000000000000, 0.000000000000000000 ) ) ;
#754 = UNCERTAINTY_MEASURE_WITH_UNIT (LENGTH_MEASURE( 1.000000000000000082E-05 ), #18890, 'distance_accuracy_value', 'NONE');
#755 = VERTEX_POINT ( 'NONE', #6502 ) ;
#756 = DIRECTION ( 'NONE',  ( -1.000000000000000000, -0.000000000000000000, -0.000000000000000000 ) ) ;
#757 = CARTESIAN_POINT ( 'NONE',  ( 15.22596115864829969, 40.00000000000000000, 57.21640888977480444 ) ) ;
#758 = EDGE_CURVE ( 'NONE', #33221, #42002, #39448, .T. ) ;
#759 = DIRECTION ( 'NONE',  ( 0.000000000000000000, 0.000000000000000000, 1.000000000000000000 ) ) ;
#760 = PRODUCT_DEFINITION_CONTEXT ( 'detailed design', #10016, 'design' ) ;
#761 = FACE_OUTER_BOUND ( 'NONE', #34017, .T. ) ;
#762 = AXIS2_PLACEMENT_3D ( 'NONE', #975, #19125, #22610 ) ;
#763 = ORIENTED_EDGE ( 'NONE', *, *, #22251, .F. ) ;
#764 = DIRECTION ( 'NONE',  ( 0.000000000000000000, 0.000000000000000000, 1.000000000000000000 ) ) ;
#765 = ORIENTED_EDGE ( 'NONE', *, *, #22439, .T. ) ;
#766 = AXIS2_PLACEMENT_3D ( 'NONE', #15610, #16042, #9468 ) ;
#767 = APPLICATION_CONTEXT ( 'automotive_design' ) ;
#768 = DIRECTION ( 'NONE',  ( -1.000000000000000000, -0.000000000000000000, -0.000000000000000000 ) ) ;
#769 = CARTESIAN_POINT ( 'NONE',  ( 17.99999999999999645, 0.000000000000000000, 0.000000000000000000 ) ) ;
#770 = VECTOR ( 'NONE', #18859, 1000.000000000000000 ) ;
#771 = CARTESIAN_POINT ( 'NONE',  ( 52.68777711438346500, 31.00000000000000355, 17.88338314711659294 ) ) ;
#772 = DIRECTION ( 'NONE',  ( 1.000000000000000000, 0.000000000000000000, 0.000000000000000000 ) ) ;
#773 = ORIENTED_EDGE ( 'NONE', *, *, #5473, .F. ) ;
#774 = DIRECTION ( 'NONE',  ( 0.000000000000000000, 0.6382441836448161654, 0.7698339834299096074 ) ) ;
#775 = EDGE_LOOP ( 'NONE', ( #28851, #2876, #36408, #17562 ) ) ;
#776 = CARTESIAN_POINT ( 'NONE',  ( -16.73417733071809721, 40.00000000000000000, -12.82953315787133519 ) ) ;
#777 = VECTOR ( 'NONE', #3980, 1000.000000000000000 ) ;
#778 = ORIENTED_EDGE ( 'NONE', *, *, #36013, .T. ) ;
#779 = CARTESIAN_POINT ( 'NONE',  ( 17.99999999999999645, 17.33727698085324320, -110.8498592715971967 ) ) ;
#780 = CARTESIAN_POINT ( 'NONE',  ( 8.999999999999998224, -82.63181128086789329, 81.41243003646944487 ) ) ;
#781 = CARTESIAN_POINT ( 'NONE',  ( 68.60033760563639760, 31.00000000000000000, -33.70054013428169526 ) ) ;
#782 = CARTESIAN_POINT ( 'NONE',  ( 57.21690105882998267, 39.99999999999999289, -50.04162206025958426 ) ) ;
#783 = CARTESIAN_POINT ( 'NONE',  ( 0.000000000000000000, 44.75336757549799671, -14.30704879393557150 ) ) ;
#784 = ORIENTED_EDGE ( 'NONE', *, *, #32544, .F. ) ;
#785 = CARTESIAN_POINT ( 'NONE',  ( 17.99999999999999645, 0.000000000000000000, 0.000000000000000000 ) ) ;
#786 = ORIENTED_EDGE ( 'NONE', *, *, #29435, .T. ) ;
#787 = CARTESIAN_POINT ( 'NONE',  ( 17.99999999999999645, 95.31344542257821217, -66.11616384574354299 ) ) ;
#788 = EDGE_CURVE ( 'NONE', #6621, #11655, #5224, .T. ) ;
#789 = DIRECTION ( 'NONE',  ( 0.000000000000000000, 0.9213119778704139673, -0.3888241754733182676 ) ) ;
#791 = ORIENTED_EDGE ( 'NONE', *, *, #42785, .T. ) ;
#790 = FACE_OUTER_BOUND ( 'NONE', #38920, .T. ) ;
#792 = EDGE_CURVE ( 'NONE', #22999, #28679, #30309, .T. ) ;
#793 = DIRECTION ( 'NONE',  ( 0.000000000000000000, 0.8183027759081702435, -0.5747874102144051589 ) ) ;
#794 = ORIENTED_EDGE ( 'NONE', *, *, #5997, .T. ) ;
#795 = CARTESIAN_POINT ( 'NONE',  ( 0.000000000000000000, 0.6819280456829140968, 115.9979955608738749 ) ) ;
#796 = CARTESIAN_POINT ( 'NONE',  ( 21.49215960483416410, 40.00000000000000000, -80.26604385357094884 ) ) ;
#797 = DIRECTION ( 'NONE',  ( 0.000000000000000000, 0.000000000000000000, -1.000000000000000000 ) ) ;
#798 = CIRCLE ( 'NONE', #6381, 58.99999999999998579 ) ;
#799 = EDGE_LOOP ( 'NONE', ( #7058, #14371, #34397, #3950 ) ) ;
#800 = DIRECTION ( 'NONE',  ( 0.000000000000000000, 0.000000000000000000, 1.000000000000000000 ) ) ;
#801 = DIRECTION ( 'NONE',  ( -1.000000000000000000, -0.000000000000000000, -0.000000000000000000 ) ) ;
#802 = AXIS2_PLACEMENT_3D ( 'NONE', #24031, #418, #849 ) ;
#803 = ORIENTED_EDGE ( 'NONE', *, *, #3371, .T. ) ;
#804 = ADVANCED_FACE ( 'NONE', ( #17457 ), #4302, .T. ) ;
#805 = CARTESIAN_POINT ( 'NONE',  ( 0.000000000000000000, -17.77780072541773748, 114.6296200873375284 ) ) ;
#806 = ORIENTED_EDGE ( 'NONE', *, *, #39159, .T. ) ;
#807 = CARTESIAN_POINT ( 'NONE',  ( 17.99999999999999645, -100.8494052988166345, -65.95368414179013428 ) ) ;
#808 = ORIENTED_EDGE ( 'NONE', *, *, #27933, .T. ) ;
#810 = CARTESIAN_POINT ( 'NONE',  ( 17.99999999999999645, -68.61497464550522807, -99.05794392877676557 ) ) ;
#809 = CIRCLE ( 'NONE', #33583, 31.49899999999999878 ) ;
#811 = DIRECTION ( 'NONE',  ( -1.000000000000000000, -0.000000000000000000, -0.000000000000000000 ) ) ;
#812 = ADVANCED_FACE ( 'NONE', ( #40957 ), #1260, .T. ) ;
#813 = CARTESIAN_POINT ( 'NONE',  ( 6.896599878636567205, -12.98179148322719101, -1.199999999999999956 ) ) ;
#814 = DIRECTION ( 'NONE',  ( 0.000000000000000000, -0.8477344278896755680, 0.5304209081197349684 ) ) ;
#815 = VERTEX_POINT ( 'NONE', #10445 ) ;
#817 = CARTESIAN_POINT ( 'NONE',  ( 8.999999999999998224, 0.000000000000000000, 0.000000000000000000 ) ) ;
#816 = CARTESIAN_POINT ( 'NONE',  ( 17.99999999999999645, 114.6488492393084613, -37.09625815499892809 ) ) ;
#818 = ORIENTED_EDGE ( 'NONE', *, *, #20409, .F. ) ;
#819 = CARTESIAN_POINT ( 'NONE',  ( 9.000000000000001776, -40.47821179127690527, -32.64221760512803172 ) ) ;
#820 = CARTESIAN_POINT ( 'NONE',  ( -24.68525358734468611, 31.00000000000000355, -18.92943107747915832 ) ) ;
#821 = VERTEX_POINT ( 'NONE', #40521 ) ;
#822 = CARTESIAN_POINT ( 'NONE',  ( 17.99999999999999645, 0.000000000000000000, 0.000000000000000000 ) ) ;
#823 = DIRECTION ( 'NONE',  ( 0.000000000000000000, -0.4610925014493143514, -0.8873520750565775383 ) ) ;
#824 = ITEM_DEFINED_TRANSFORMATION ( 'NONE', 'NONE', #6528,  #13552 ) ;
#825 = CARTESIAN_POINT ( 'NONE',  ( 9.000000000000001776, 19.12429268481864142, -114.4126803693777248 ) ) ;
#826 = AXIS2_PLACEMENT_3D ( 'NONE', #21872, #28610, #21453 ) ;
#827 = CARTESIAN_POINT ( 'NONE',  ( -61.47519263390311295, 31.00000000000000711, -35.49250405583519807 ) ) ;
#829 = EDGE_CURVE ( 'NONE', #19014, #17523, #39330, .T. ) ;
#828 = AXIS2_PLACEMENT_3D ( 'NONE', #23833, #39922, #37099 ) ;
#830 = AXIS2_PLACEMENT_3D ( 'NONE', #30813, #14241, #7673 ) ;
#831 = ORIENTED_EDGE ( 'NONE', *, *, #7767, .F. ) ;
#832 = CARTESIAN_POINT ( 'NONE',  ( 22.78600399167716262, 31.00000000000000355, -39.30137845375363526 ) ) ;
#833 = AXIS2_PLACEMENT_3D ( 'NONE', #2147, #5444, #11574 ) ;
#834 = CARTESIAN_POINT ( 'NONE',  ( -68.69954721042445556, 40.00000000000000711, 39.68009708086182741 ) ) ;
#835 = CIRCLE ( 'NONE', #12740, 59.00000000000000000 ) ;
#836 = DIRECTION ( 'NONE',  ( -1.000000000000000000, -0.000000000000000000, -0.000000000000000000 ) ) ;
#837 = DIRECTION ( 'NONE',  ( 0.000000000000000000, 0.000000000000000000, 1.000000000000000000 ) ) ;
#838 = DIRECTION ( 'NONE',  ( -1.000000000000000000, 0.000000000000000000, -0.000000000000000000 ) ) ;
#840 = ORIENTED_EDGE ( 'NONE', *, *, #25056, .F. ) ;
#839 = LINE ( 'NONE', #24020, #21677 ) ;
#841 = CARTESIAN_POINT ( 'NONE',  ( 9.000000000000001776, 49.65209126885763169, 15.44894276735568006 ) ) ;
#842 = DIRECTION ( 'NONE',  ( -1.000000000000000000, -0.000000000000000000, 0.000000000000000000 ) ) ;
#843 = ADVANCED_FACE ( 'NONE', ( #377 ), #20735, .F. ) ;
#844 = VERTEX_POINT ( 'NONE', #37259 ) ;
#845 = CARTESIAN_POINT ( 'NONE',  ( -47.94314659152439617, 40.00000000000000000, -16.27230485535717719 ) ) ;
#846 = CARTESIAN_POINT ( 'NONE',  ( 0.000000000000000000, -19.74581912682875284, 48.10512059033386123 ) ) ;
#847 = FACE_BOUND ( 'NONE', #40043, .T. ) ;
#848 = VERTEX_POINT ( 'NONE', #27911 ) ;
#849 = DIRECTION ( 'NONE',  ( 0.000000000000000000, 0.9996456111234526265, -0.02662052143777148688 ) ) ;
#850 = DIRECTION ( 'NONE',  ( -1.000000000000000000, 0.000000000000000000, -0.000000000000000000 ) ) ;
#851 = ORIENTED_EDGE ( 'NONE', *, *, #31292, .F. ) ;
#852 = DIRECTION ( 'NONE',  ( -1.000000000000000000, -0.000000000000000000, -0.000000000000000000 ) ) ;
#853 = ORIENTED_EDGE ( 'NONE', *, *, #28742, .T. ) ;
#854 = EDGE_CURVE ( 'NONE', #30629, #15430, #13742, .T. ) ;
#855 = DIRECTION ( 'NONE',  ( -1.000000000000000000, 0.000000000000000000, -0.000000000000000000 ) ) ;
#856 = ORIENTED_EDGE ( 'NONE', *, *, #38823, .F. ) ;
#857 = DIRECTION ( 'NONE',  ( 1.000000000000000000, 0.000000000000000000, 0.000000000000000000 ) ) ;
#858 = CARTESIAN_POINT ( 'NONE',  ( -96.33078216555148288, 31.00000000000000711, 32.58251675337926656 ) ) ;
#859 = ADVANCED_FACE ( 'NONE', ( #7595 ), #30942, .T. ) ;
#860 = EDGE_LOOP ( 'NONE', ( #15062, #36163, #30682, #9307 ) ) ;
#861 = AXIS2_PLACEMENT_3D ( 'NONE', #29019, #9136, #25758 ) ;
#862 = CYLINDRICAL_SURFACE ( 'NONE', #8706, 59.00000000000000000 ) ;
#863 = DIRECTION ( 'NONE',  ( 0.000000000000000000, 0.000000000000000000, 1.000000000000000000 ) ) ;
#864 = ORIENTED_EDGE ( 'NONE', *, *, #13821, .F. ) ;
#865 = CARTESIAN_POINT ( 'NONE',  ( 18.00000000000000355, -19.44205635905511897, -43.33776004284629124 ) ) ;
#866 = AXIS2_PLACEMENT_3D ( 'NONE', #26406, #23791, #17470 ) ;
#867 = CARTESIAN_POINT ( 'NONE',  ( 0.000000000000000000, 0.000000000000000000, 0.000000000000000000 ) ) ;
#868 = DIRECTION ( 'NONE',  ( 0.000000000000000000, 0.000000000000000000, 1.000000000000000000 ) ) ;
#869 = DIRECTION ( 'NONE',  ( 0.000000000000000000, 0.000000000000000000, 1.000000000000000000 ) ) ;
#870 = ORIENTED_EDGE ( 'NONE', *, *, #13246, .F. ) ;
#871 = DIRECTION ( 'NONE',  ( -0.7135933283232640534, 2.775557561562891351E-17, -0.7005601771243683551 ) ) ;
#872 = FACE_OUTER_BOUND ( 'NONE', #36740, .T. ) ;
#873 = CARTESIAN_POINT ( 'NONE',  ( 21.71086051706764763, 31.00000000000000355, -37.60982366119799991 ) ) ;
#874 = EDGE_CURVE ( 'NONE', #13955, #7568, #32381, .T. ) ;
#875 = EDGE_LOOP ( 'NONE', ( #609, #11222 ) ) ;
#877 = CARTESIAN_POINT ( 'NONE',  ( 17.99999999999999645, 0.000000000000000000, 0.000000000000000000 ) ) ;
#876 = CARTESIAN_POINT ( 'NONE',  ( 0.000000000000000000, -20.99948489194451540, 42.60488980472774045 ) ) ;
#878 = EDGE_CURVE ( 'NONE', #38848, #5227, #1025, .T. ) ;
#879 = DIRECTION ( 'NONE',  ( -1.000000000000000000, -0.000000000000000000, 0.000000000000000000 ) ) ;
#880 = VERTEX_POINT ( 'NONE', #27042 ) ;
#881 = CARTESIAN_POINT ( 'NONE',  ( 18.00000000000000355, 11.46872990052381880, 45.56340405422447049 ) ) ;
#882 = CARTESIAN_POINT ( 'NONE',  ( 6.197074855318628117, 40.00000000000000000, 46.98549035852928313 ) ) ;
#883 = CARTESIAN_POINT ( 'NONE',  ( 56.43498182459031653, 40.00000000000000000, -7.339809665447900144 ) ) ;
#884 = CIRCLE ( 'NONE', #32268, 13.59999999999999964 ) ;
#885 = EDGE_CURVE ( 'NONE', #23736, #7766, #38626, .T. ) ;
#886 = DIRECTION ( 'NONE',  ( -1.000000000000000000, 0.000000000000000000, 0.000000000000000000 ) ) ;
#887 = DIRECTION ( 'NONE',  ( 0.000000000000000000, 0.000000000000000000, 1.000000000000000000 ) ) ;
#888 = DIRECTION ( 'NONE',  ( 1.000000000000000000, -1.373900992973641868E-15, -3.994789077170585140E-16 ) ) ;
#889 = DIRECTION ( 'NONE',  ( 1.000000000000000000, 0.000000000000000000, 0.000000000000000000 ) ) ;
#890 = MECHANICAL_DESIGN_GEOMETRIC_PRESENTATION_REPRESENTATION (  '', ( #26712 ), #21180 ) ;
#891 = EDGE_CURVE ( 'NONE', #14013, #31709, #31171, .T. ) ;
#892 = ORIENTED_EDGE ( 'NONE', *, *, #25986, .F. ) ;
#893 = CARTESIAN_POINT ( 'NONE',  ( 24.60508655230852781, 40.00000000000000000, 6.583411914924224284 ) ) ;
#894 = EDGE_LOOP ( 'NONE', ( #24102, #33769, #35658, #18050 ) ) ;
#895 = CARTESIAN_POINT ( 'NONE',  ( 17.99999999999999645, -28.62203781742993414, -14.19692359621484989 ) ) ;
#896 = CARTESIAN_POINT ( 'NONE',  ( 109.0695705685763244, -106.4195705685744855, 6.999999999999998224 ) ) ;
#897 = EDGE_LOOP ( 'NONE', ( #25009, #43120, #20954, #33292 ) ) ;
#898 = DIRECTION ( 'NONE',  ( 1.000000000000000000, 0.000000000000000000, 0.000000000000000000 ) ) ;
#899 = CARTESIAN_POINT ( 'NONE',  ( 17.99999999999999645, 107.5680526044915410, 31.89649718262280231 ) ) ;
#900 = ORIENTED_EDGE ( 'NONE', *, *, #42670, .F. ) ;
#901 = FACE_OUTER_BOUND ( 'NONE', #22484, .T. ) ;
#902 = EDGE_LOOP ( 'NONE', ( #20737, #30290, #24579, #39196 ) ) ;
#903 = FACE_OUTER_BOUND ( 'NONE', #27461, .T. ) ;
#904 = EDGE_CURVE ( 'NONE', #35878, #42716, #20582, .T. ) ;
#905 = ORIENTED_EDGE ( 'NONE', *, *, #39410, .T. ) ;
#906 = ORIENTED_EDGE ( 'NONE', *, *, #34748, .T. ) ;
#907 = CARTESIAN_POINT ( 'NONE',  ( 58.79931003850258975, 31.00000000000000355, 51.72161244499935151 ) ) ;
#908 = ADVANCED_FACE ( 'NONE', ( #10220 ), #3863, .T. ) ;
#909 = VERTEX_POINT ( 'NONE', #37689 ) ;
#910 = DIRECTION ( 'NONE',  ( -1.000000000000000000, -0.000000000000000000, -0.000000000000000000 ) ) ;
#911 = AXIS2_PLACEMENT_3D ( 'NONE', #21019, #9699, #10718 ) ;
#912 = ORIENTED_EDGE ( 'NONE', *, *, #3824, .F. ) ;
#913 = DIRECTION ( 'NONE',  ( 1.000000000000000000, 0.000000000000000000, 0.000000000000000000 ) ) ;
#914 = ORIENTED_EDGE ( 'NONE', *, *, #37764, .T. ) ;
#915 = VECTOR ( 'NONE', #26629, 1000.000000000000000 ) ;
#916 = CARTESIAN_POINT ( 'NONE',  ( 63.29164158768324455, 39.99999999999999289, -71.97807289018581400 ) ) ;
#918 = DIRECTION ( 'NONE',  ( 0.000000000000000000, 0.000000000000000000, 1.000000000000000000 ) ) ;
#917 = CYLINDRICAL_SURFACE ( 'NONE', #38439, 116.0000000000000000 ) ;
#919 = CARTESIAN_POINT ( 'NONE',  ( 0.000000000000000000, -44.47301969247456555, 16.68249143361894582 ) ) ;
#920 = FACE_BOUND ( 'NONE', #14156, .T. ) ;
#921 =( GEOMETRIC_REPRESENTATION_CONTEXT ( 3 ) GLOBAL_UNCERTAINTY_ASSIGNED_CONTEXT ( ( #23939 ) ) GLOBAL_UNIT_ASSIGNED_CONTEXT ( ( #36668, #19284, #23199 ) ) REPRESENTATION_CONTEXT ( 'NONE', 'WORKASPACE' ) );
#922 = ORIENTED_EDGE ( 'NONE', *, *, #27475, .T. ) ;
#923 = DIRECTION ( 'NONE',  ( -1.000000000000000000, 0.000000000000000000, -0.000000000000000000 ) ) ;
#924 = CIRCLE ( 'NONE', #15612, 116.0000000000000000 ) ;
#925 = CARTESIAN_POINT ( 'NONE',  ( -4.000000000000000000, -2.309401076758512694, -3.433295621305382461 ) ) ;
#926 = EDGE_CURVE ( 'NONE', #27914, #34568, #8609, .T. ) ;
#927 = CARTESIAN_POINT ( 'NONE',  ( -39.09256291070916944, 31.00000000000000355, 79.30589209199378331 ) ) ;
#928 = EDGE_CURVE ( 'NONE', #37599, #28601, #37468, .T. ) ;
#929 = CARTESIAN_POINT ( 'NONE',  ( 0.000000000000000000, 0.000000000000000000, 0.000000000000000000 ) ) ;
#930 = ORIENTED_EDGE ( 'NONE', *, *, #21468, .T. ) ;
#931 = EDGE_CURVE ( 'NONE', #37795, #12884, #15890, .T. ) ;
#932 = ADVANCED_FACE ( 'NONE', ( #32027 ), #38338, .F. ) ;
#933 = AXIS2_PLACEMENT_3D ( 'NONE', #39544, #9680, #23024 ) ;
#934 = CARTESIAN_POINT ( 'NONE',  ( -15.43003214871520434, 40.00000000000000000, -17.59684744742188300 ) ) ;
#935 = ORIENTED_EDGE ( 'NONE', *, *, #8134, .T. ) ;
#936 = ORIENTED_EDGE ( 'NONE', *, *, #3217, .T. ) ;
#937 = SURFACE_STYLE_USAGE ( .BOTH. , #27168 ) ;
#938 = CARTESIAN_POINT ( 'NONE',  ( 56.05503971749756431, -12.05525454449572464, 8.006123197671259462 ) ) ;
#939 = CARTESIAN_POINT ( 'NONE',  ( -153.1500000000000057, -5.251434100941175950E-13, 9.999999999999998224 ) ) ;
#940 = EDGE_CURVE ( 'NONE', #30306, #27122, #29838, .T. ) ;
#941 = AXIS2_PLACEMENT_3D ( 'NONE', #14396, #33790, #37498 ) ;
#942 = DIRECTION ( 'NONE',  ( -3.996523416598930318E-16, 2.658563593772947863E-15, 1.000000000000000000 ) ) ;
#943 = VECTOR ( 'NONE', #11137, 1000.000000000000000 ) ;
#944 = ORIENTED_EDGE ( 'NONE', *, *, #37002, .T. ) ;
#945 = CYLINDRICAL_SURFACE ( 'NONE', #19407, 126.0000000000000284 ) ;
#946 = ORIENTED_EDGE ( 'NONE', *, *, #39507, .T. ) ;
#947 = CARTESIAN_POINT ( 'NONE',  ( 17.99999999999999645, 112.1427988504408404, -3.502162136922268409 ) ) ;
#948 = DIRECTION ( 'NONE',  ( 0.000000000000000000, 0.1837495178165638177, 0.9829730996839030066 ) ) ;
#949 = DIRECTION ( 'NONE',  ( 1.000000000000000000, 0.000000000000000000, 0.000000000000000000 ) ) ;
#950 = DIRECTION ( 'NONE',  ( -1.000000000000000000, 0.000000000000000000, 0.000000000000000000 ) ) ;
#951 = EDGE_LOOP ( 'NONE', ( #22743, #10963, #794, #31874 ) ) ;
#952 = VERTEX_POINT ( 'NONE', #8894 ) ;
#953 = DIRECTION ( 'NONE',  ( -1.000000000000000000, -0.000000000000000000, 0.000000000000000000 ) ) ;
#954 = CARTESIAN_POINT ( 'NONE',  ( 25.04716826810500763, 31.00000000000000355, 3.293035637142270655 ) ) ;
#955 = CARTESIAN_POINT ( 'NONE',  ( -139.4999999999992610, 2.182448244575515701E-13, 10.00000000000005684 ) ) ;
#956 = EDGE_CURVE ( 'NONE', #20569, #39944, #24280, .T. ) ;
#957 = DIRECTION ( 'NONE',  ( -1.000000000000000000, 0.000000000000000000, 0.000000000000000000 ) ) ;
#958 = AXIS2_PLACEMENT_3D ( 'NONE', #18288, #37644, #21128 ) ;
#959 = VERTEX_POINT ( 'NONE', #25095 ) ;
#961 = ORIENTED_EDGE ( 'NONE', *, *, #23057, .T. ) ;
#960 = FACE_OUTER_BOUND ( 'NONE', #43029, .T. ) ;
#962 = CARTESIAN_POINT ( 'NONE',  ( -19.32876798325804302, 31.00000000000000355, -39.37500834189552279 ) ) ;
#963 = EDGE_CURVE ( 'NONE', #39350, #15922, #24979, .T. ) ;
#964 = CARTESIAN_POINT ( 'NONE',  ( 18.00000000000000355, 0.000000000000000000, 0.000000000000000000 ) ) ;
#965 = AXIS2_PLACEMENT_3D ( 'NONE', #8712, #15089, #35532 ) ;
#967 = VERTEX_POINT ( 'NONE', #5404 ) ;
#966 = CARTESIAN_POINT ( 'NONE',  ( 18.00000000000000355, 2.123073309835852296, -47.45152853935331905 ) ) ;
#968 = ORIENTED_EDGE ( 'NONE', *, *, #16720, .T. ) ;
#969 = CARTESIAN_POINT ( 'NONE',  ( 60.82800096160986669, 39.99999999999999289, 30.10617641797072963 ) ) ;
#970 = CIRCLE ( 'NONE', #29563, 11.00000000000000000 ) ;
#971 = CARTESIAN_POINT ( 'NONE',  ( -2.059999999999998721, 2.522772406243545965E-16, -0.3080913168122742518 ) ) ;
#972 = AXIS2_PLACEMENT_3D ( 'NONE', #2544, #29205, #40272 ) ;
#973 = FACE_OUTER_BOUND ( 'NONE', #23662, .T. ) ;
#974 = ORIENTED_EDGE ( 'NONE', *, *, #40589, .F. ) ;
#975 = CARTESIAN_POINT ( 'NONE',  ( 18.00000000000000355, 0.000000000000000000, 0.000000000000000000 ) ) ;
#976 = VERTEX_POINT ( 'NONE', #15272 ) ;
#977 = CIRCLE ( 'NONE', #4471, 10.50000000000000178 ) ;
#978 = DIRECTION ( 'NONE',  ( -1.000000000000000000, 0.000000000000000000, -0.000000000000000000 ) ) ;
#979 = CARTESIAN_POINT ( 'NONE',  ( 17.99999999999999645, 35.72777019205667415, 106.3569410558018404 ) ) ;
#980 = EDGE_CURVE ( 'NONE', #6774, #2440, #28766, .T. ) ;
#981 = CARTESIAN_POINT ( 'NONE',  ( 54.89583333452979730, 31.00000000000000355, -3.599741573803383332 ) ) ;
#982 = EDGE_CURVE ( 'NONE', #41341, #19395, #11317, .T. ) ;
#983 = FACE_OUTER_BOUND ( 'NONE', #36703, .T. ) ;
#984 = ORIENTED_EDGE ( 'NONE', *, *, #40319, .F. ) ;
#985 = ADVANCED_FACE ( 'NONE', ( #21393 ), #5177, .F. ) ;
#986 = EDGE_CURVE ( 'NONE', #1564, #14692, #18727, .T. ) ;
#987 = AXIS2_PLACEMENT_3D ( 'NONE', #7218, #20574, #3932 ) ;
#988 = EDGE_CURVE ( 'NONE', #38106, #24796, #34858, .T. ) ;
#989 = CARTESIAN_POINT ( 'NONE',  ( 2.000000000000008882, 3.464101615137749945, 0.000000000000000000 ) ) ;
#990 = VERTEX_POINT ( 'NONE', #24646 ) ;
#991 = CARTESIAN_POINT ( 'NONE',  ( -4.233603722440171246, 40.00000000000000000, -32.08218167604271542 ) ) ;
#992 = ORIENTED_EDGE ( 'NONE', *, *, #4759, .F. ) ;
#993 = DIRECTION ( 'NONE',  ( -1.000000000000000000, -0.000000000000000000, 0.000000000000000000 ) ) ;
#994 = DIRECTION ( 'NONE',  ( 1.000000000000000000, 0.000000000000000000, 0.000000000000000000 ) ) ;
#995 = CARTESIAN_POINT ( 'NONE',  ( 72.60479858918232310, 31.00000000000000000, -24.53750584076950503 ) ) ;
#996 = CARTESIAN_POINT ( 'NONE',  ( 60.45897909546184934, 39.99999999999999289, -46.24578392211154210 ) ) ;
#997 = DIRECTION ( 'NONE',  ( -1.000000000000000000, 0.000000000000000000, 0.000000000000000000 ) ) ;
#998 = AXIS2_PLACEMENT_3D ( 'NONE', #24641, #24427, #14162 ) ;
#999 = AXIS2_PLACEMENT_3D ( 'NONE', #30530, #600, #23567 ) ;
#1000 = ORIENTED_EDGE ( 'NONE', *, *, #14875, .T. ) ;
#1001 = DIRECTION ( 'NONE',  ( -1.000000000000000000, 0.000000000000000000, 0.000000000000000000 ) ) ;
#1002 = ORIENTED_EDGE ( 'NONE', *, *, #16383, .T. ) ;
#1003 = CARTESIAN_POINT ( 'NONE',  ( 32.30287614962725229, -35.35525454449572180, 69.29271901957299917 ) ) ;
#1004 = AXIS2_PLACEMENT_3D ( 'NONE', #40545, #838, #17927 ) ;
#1005 = LINE ( 'NONE', #30507, #336 ) ;
#1006 = VECTOR ( 'NONE', #32825, 1000.000000000000000 ) ;
#1008 = ORIENTED_EDGE ( 'NONE', *, *, #6860, .T. ) ;
#1007 = DIRECTION ( 'NONE',  ( 0.000000000000000000, 0.000000000000000000, 1.000000000000000000 ) ) ;
#1009 = FACE_OUTER_BOUND ( 'NONE', #21764, .T. ) ;
#1010 = ORIENTED_EDGE ( 'NONE', *, *, #30191, .T. ) ;
#1011 = DIRECTION ( 'NONE',  ( 0.000000000000000000, -0.5963673585385078635, 0.8027116379309588989 ) ) ;
#1012 = CARTESIAN_POINT ( 'NONE',  ( 76.36724925129128394, 39.99999999999999289, 58.57876755120444301 ) ) ;
#1013 = LINE ( 'NONE', #20939, #23659 ) ;
#1014 = ORIENTED_EDGE ( 'NONE', *, *, #35545, .F. ) ;
#1015 = DIRECTION ( 'NONE',  ( -1.000000000000000000, 0.000000000000000000, 0.000000000000000000 ) ) ;
#1016 = DIRECTION ( 'NONE',  ( -1.000000000000000000, -0.000000000000000000, -0.000000000000000000 ) ) ;
#1017 = EDGE_CURVE ( 'NONE', #26550, #30103, #18543, .T. ) ;
#1018 = CIRCLE ( 'NONE', #40724, 116.0000000000000000 ) ;
#1019 = FILL_AREA_STYLE ('',( #24212 ) ) ;
#1020 = VERTEX_POINT ( 'NONE', #41166 ) ;
#1021 = CARTESIAN_POINT ( 'NONE',  ( 0.000000000000000000, 45.78515115856060191, -12.64416602183617577 ) ) ;
#1022 = ORIENTED_EDGE ( 'NONE', *, *, #9532, .F. ) ;
#1023 = CARTESIAN_POINT ( 'NONE',  ( -18.66214908251097881, 40.00000000000000000, 24.25811346063289164 ) ) ;
#1024 = DIRECTION ( 'NONE',  ( -1.058513553088275437E-16, -1.000000000000000000, 8.813324511995299047E-17 ) ) ;
#1025 = LINE ( 'NONE', #34207, #33055 ) ;
#1026 = AXIS2_PLACEMENT_3D ( 'NONE', #28287, #21111, #7751 ) ;
#1027 = CARTESIAN_POINT ( 'NONE',  ( 17.99999999999999645, -111.1352304691228596, 15.40237066878559524 ) ) ;
#1029 = ORIENTED_EDGE ( 'NONE', *, *, #12507, .F. ) ;
#1028 = CIRCLE ( 'NONE', #32411, 31.49899999999999878 ) ;
#1031 = DIRECTION ( 'NONE',  ( 1.000000000000000000, 0.000000000000000000, 0.000000000000000000 ) ) ;
#1030 = CARTESIAN_POINT ( 'NONE',  ( -6.200000000000001066, 18.77999999999999758, 0.000000000000000000 ) ) ;
#1032 = ORIENTED_EDGE ( 'NONE', *, *, #22720, .T. ) ;
#1033 = AXIS2_PLACEMENT_3D ( 'NONE', #6274, #5845, #19201 ) ;
#1034 = FACE_OUTER_BOUND ( 'NONE', #27525, .T. ) ;
#1035 = AXIS2_PLACEMENT_3D ( 'NONE', #1477, #28568, #4981 ) ;
#1036 = CARTESIAN_POINT ( 'NONE',  ( 23.12883206328222130, 31.00000000000000355, 11.39561251172168355 ) ) ;
#1037 = ORIENTED_EDGE ( 'NONE', *, *, #36924, .F. ) ;
#1038 = CARTESIAN_POINT ( 'NONE',  ( 0.000000000000000000, 0.000000000000000000, 0.000000000000000000 ) ) ;
#1039 = CIRCLE ( 'NONE', #13632, 120.5010000000000190 ) ;
#1040 = ADVANCED_FACE ( 'NONE', ( #31818 ), #1685, .F. ) ;
#1041 = EDGE_CURVE ( 'NONE', #35404, #38913, #11022, .T. ) ;
#1042 = FACE_BOUND ( 'NONE', #4502, .T. ) ;
#1043 = CONTEXT_DEPENDENT_SHAPE_REPRESENTATION ( #29529, #32173 ) ;
#1044 = EDGE_CURVE ( 'NONE', #28956, #25474, #28562, .T. ) ;
#1046 = AXIS2_PLACEMENT_3D ( 'NONE', #16688, #39312, #36058 ) ;
#1045 = CARTESIAN_POINT ( 'NONE',  ( 17.99999999999999645, 23.10276247328101817, 118.2656051737070726 ) ) ;
#1047 = CARTESIAN_POINT ( 'NONE',  ( 40.54457361686378647, 31.00000000000000355, 52.83773991529862712 ) ) ;
#1048 = ORIENTED_EDGE ( 'NONE', *, *, #15189, .T. ) ;
#1049 = CARTESIAN_POINT ( 'NONE',  ( 38.14553738579559905, 31.00000000000000355, 29.36968266378863746 ) ) ;
#1050 = CARTESIAN_POINT ( 'NONE',  ( -76.41092972884307244, 40.00000000000000711, -25.93877460596726436 ) ) ;
#1051 = ADVANCED_FACE ( 'NONE', ( #41826 ), #22022, .F. ) ;
#1052 = CARTESIAN_POINT ( 'NONE',  ( 5.657435538624008755E-15, 4.615443851143735910E-16, -20.00000000000001776 ) ) ;
#1053 = EDGE_CURVE ( 'NONE', #10216, #990, #8208, .T. ) ;
#1054 = CARTESIAN_POINT ( 'NONE',  ( 26.85238513915532721, -2.055254544495723756, 88.54322126041917329 ) ) ;
#1055 = CARTESIAN_POINT ( 'NONE',  ( 42.80287614962790599, -14.05525454449571932, 69.29271901957253021 ) ) ;
#1056 = AXIS2_PLACEMENT_3D ( 'NONE', #38928, #28514, #25246 ) ;
#1057 = AXIS2_PLACEMENT_3D ( 'NONE', #31225, #645, #40360 ) ;
#1059 = VERTEX_POINT ( 'NONE', #1467 ) ;
#1058 = DIRECTION ( 'NONE',  ( -1.000000000000000000, -0.000000000000000000, -0.000000000000000000 ) ) ;
#1060 = CARTESIAN_POINT ( 'NONE',  ( 17.99999999999999645, 19.69434969228107946, -24.58291258574028504 ) ) ;
#1061 = AXIS2_PLACEMENT_3D ( 'NONE', #3485, #16649, #12857 ) ;
#1062 = LINE ( 'NONE', #10025, #39695 ) ;
#1063 = ORIENTED_EDGE ( 'NONE', *, *, #11889, .T. ) ;
#1064 = CARTESIAN_POINT ( 'NONE',  ( 47.00375723443311671, 40.00000000000000000, -27.15133022689256137 ) ) ;
#1065 = CARTESIAN_POINT ( 'NONE',  ( 17.99999999999999645, -119.7318547011700502, -13.59315897125848238 ) ) ;
#1066 = FACE_OUTER_BOUND ( 'NONE', #10074, .T. ) ;
#1067 = AXIS2_PLACEMENT_3D ( 'NONE', #24112, #32133, #25203 ) ;
#1068 = ORIENTED_EDGE ( 'NONE', *, *, #42063, .F. ) ;
#1069 = DIRECTION ( 'NONE',  ( 0.000000000000000000, 0.000000000000000000, -1.000000000000000000 ) ) ;
#1070 = CARTESIAN_POINT ( 'NONE',  ( -4.000000000000000000, -1.560351142792950618, -0.2242961665059814425 ) ) ;
#1071 = AXIS2_PLACEMENT_3D ( 'NONE', #15177, #27600, #8166 ) ;
#1072 = VERTEX_POINT ( 'NONE', #41383 ) ;
#1073 = DIRECTION ( 'NONE',  ( 0.000000000000000000, 0.5264321628773506179, 0.8502171357296174348 ) ) ;
#1074 = EDGE_LOOP ( 'NONE', ( #11891, #33108, #40829, #19012 ) ) ;
#1075 = ADVANCED_FACE ( 'NONE', ( #35492 ), #15037, .F. ) ;
#1076 = CARTESIAN_POINT ( 'NONE',  ( 17.99999999999999645, 108.8684555192050425, -27.12806418649509865 ) ) ;
#1077 = ORIENTED_EDGE ( 'NONE', *, *, #32254, .F. ) ;
#1078 = DIRECTION ( 'NONE',  ( -1.000000000000000000, 0.000000000000000000, -0.000000000000000000 ) ) ;
#1079 = LINE ( 'NONE', #1308, #38060 ) ;
#1080 = ORIENTED_EDGE ( 'NONE', *, *, #13414, .F. ) ;
#1081 = DIRECTION ( 'NONE',  ( 1.000000000000000000, 1.836909530733573776E-16, 0.000000000000000000 ) ) ;
#1082 = CARTESIAN_POINT ( 'NONE',  ( 17.99999999999999645, -75.72520367775034345, -82.78868281116056949 ) ) ;
#1083 = ORIENTED_EDGE ( 'NONE', *, *, #35669, .F. ) ;
#1084 = CARTESIAN_POINT ( 'NONE',  ( 0.000000000000000000, 0.000000000000000000, -20.00000000000000000 ) ) ;
#1085 = DIRECTION ( 'NONE',  ( 0.5000000000000022204, 0.8660254037844374864, -0.000000000000000000 ) ) ;
#1086 = VECTOR ( 'NONE', #19756, 1000.000000000000000 ) ;
#1087 = FACE_OUTER_BOUND ( 'NONE', #9984, .T. ) ;
#1088 = ADVANCED_FACE ( 'NONE', ( #42882 ), #16099, .T. ) ;
#1089 = DIRECTION ( 'NONE',  ( 1.000000000000000000, 0.000000000000000000, 0.000000000000000000 ) ) ;
#1090 = AXIS2_PLACEMENT_3D ( 'NONE', #18379, #25768, #18816 ) ;
#1091 = EDGE_CURVE ( 'NONE', #37611, #35369, #9602, .T. ) ;
#1092 = EDGE_LOOP ( 'NONE', ( #29241, #12983 ) ) ;
#1093 = AXIS2_PLACEMENT_3D ( 'NONE', #27876, #28528, #8219 ) ;
#1094 = DIRECTION ( 'NONE',  ( -1.836909530733573776E-16, -1.000000000000000000, 0.000000000000000000 ) ) ;
#1095 = CARTESIAN_POINT ( 'NONE',  ( 18.00000000000000355, 46.87740477351718482, 16.82754413119463166 ) ) ;
#1096 = CARTESIAN_POINT ( 'NONE',  ( 28.66079171547214699, 31.00000000000000355, 21.97938003711830035 ) ) ;
#1097 = ORIENTED_EDGE ( 'NONE', *, *, #35883, .F. ) ;
#1098 = VECTOR ( 'NONE', #1166, 1000.000000000000000 ) ;
#1100 = CARTESIAN_POINT ( 'NONE',  ( -5.639656061357299244, -10.48075544252182922, -1.199999999999999956 ) ) ;
#1099 = FACE_OUTER_BOUND ( 'NONE', #14245, .T. ) ;
#1101 = VECTOR ( 'NONE', #5570, 1000.000000000000000 ) ;
#1102 = CARTESIAN_POINT ( 'NONE',  ( 0.000000000000000000, 0.000000000000000000, 0.000000000000000000 ) ) ;
#1103 = VERTEX_POINT ( 'NONE', #43106 ) ;
#1104 = AXIS2_PLACEMENT_3D ( 'NONE', #21842, #32253, #22048 ) ;
#1105 = EDGE_CURVE ( 'NONE', #15611, #25329, #26347, .T. ) ;
#1106 = VECTOR ( 'NONE', #4814, 1000.000000000000000 ) ;
#1107 = FACE_OUTER_BOUND ( 'NONE', #41830, .T. ) ;
#1108 = CARTESIAN_POINT ( 'NONE',  ( 12.21457428495364006, 40.00000000000000000, 45.57612047952555656 ) ) ;
#1109 = CARTESIAN_POINT ( 'NONE',  ( -47.35250803175856049, 40.00000000000000000, -23.44639516808875257 ) ) ;
#1110 = EDGE_CURVE ( 'NONE', #26358, #42713, #39820, .T. ) ;
#1111 = AXIS2_PLACEMENT_3D ( 'NONE', #4135, #21442, #27296 ) ;
#1112 = FACE_OUTER_BOUND ( 'NONE', #23319, .T. ) ;
#1113 = EDGE_CURVE ( 'NONE', #25476, #1122, #22887, .T. ) ;
#1114 = DIRECTION ( 'NONE',  ( -1.000000000000000000, 0.000000000000000000, 0.000000000000000000 ) ) ;
#1115 = LINE ( 'NONE', #41249, #32972 ) ;
#1116 = CARTESIAN_POINT ( 'NONE',  ( 0.000000000000000000, 0.000000000000000000, 0.000000000000000000 ) ) ;
#1117 = ORIENTED_EDGE ( 'NONE', *, *, #14504, .F. ) ;
#1118 = CARTESIAN_POINT ( 'NONE',  ( 25.10416666396844576, 40.00000000000000000, 1.636246165087044124 ) ) ;
#1119 = ORIENTED_EDGE ( 'NONE', *, *, #1105, .F. ) ;
#1120 = CYLINDRICAL_SURFACE ( 'NONE', #4108, 120.5010000000000190 ) ;
#1121 = LINE ( 'NONE', #5270, #14511 ) ;
#1122 = VERTEX_POINT ( 'NONE', #9534 ) ;
#1123 = VECTOR ( 'NONE', #42915, 1000.000000000000000 ) ;
#1124 = DIRECTION ( 'NONE',  ( -1.000000000000000000, 0.000000000000000000, 0.000000000000000000 ) ) ;
#1125 = CARTESIAN_POINT ( 'NONE',  ( 18.00000000000000355, 0.6505223195683098592, 51.99593080916757515 ) ) ;
#1126 = ORIENTED_EDGE ( 'NONE', *, *, #36071, .T. ) ;
#1127 = CARTESIAN_POINT ( 'NONE',  ( 17.99999999999999645, 0.000000000000000000, 0.000000000000000000 ) ) ;
#1128 = VECTOR ( 'NONE', #24223, 1000.000000000000000 ) ;
#1129 = ORIENTED_EDGE ( 'NONE', *, *, #17307, .T. ) ;
#1130 = AXIS2_PLACEMENT_3D ( 'NONE', #36549, #35909, #36340 ) ;
#1131 = EDGE_CURVE ( 'NONE', #1479, #25103, #35694, .T. ) ;
#1132 = AXIS2_PLACEMENT_3D ( 'NONE', #26513, #40223, #10359 ) ;
#1133 = EDGE_CURVE ( 'NONE', #20337, #15352, #38862, .T. ) ;
#1134 = EDGE_LOOP ( 'NONE', ( #26701, #6464, #26573, #27044 ) ) ;
#1135 = CARTESIAN_POINT ( 'NONE',  ( 17.99999999999999645, 66.49630760163600485, 90.36876423296011751 ) ) ;
#1136 = CARTESIAN_POINT ( 'NONE',  ( 50.06853320191206791, 31.00000000000000000, -56.91684085115753078 ) ) ;
#1138 = ADVANCED_FACE ( 'NONE', ( #39392 ), #9094, .F. ) ;
#1137 = EDGE_LOOP ( 'NONE', ( #30207, #1126, #30886, #19679 ) ) ;
#1139 = DIRECTION ( 'NONE',  ( -1.000000000000000000, -0.000000000000000000, -0.000000000000000000 ) ) ;
#1140 = AXIS2_PLACEMENT_3D ( 'NONE', #22224, #25270, #35675 ) ;
#1141 = DIRECTION ( 'NONE',  ( 0.000000000000000000, 0.000000000000000000, 1.000000000000000000 ) ) ;
#1142 = ORIENTED_EDGE ( 'NONE', *, *, #23345, .T. ) ;
#1143 = CARTESIAN_POINT ( 'NONE',  ( 0.000000000000000000, -19.12429268481634281, -114.4126803693781085 ) ) ;
#1144 = AXIS2_PLACEMENT_3D ( 'NONE', #30578, #20557, #14211 ) ;
#1145 = ORIENTED_EDGE ( 'NONE', *, *, #9536, .T. ) ;
#1146 = CARTESIAN_POINT ( 'NONE',  ( 58.37089435906660384, 39.99999999999999289, -75.89027429297954086 ) ) ;
#1148 = CARTESIAN_POINT ( 'NONE',  ( 0.000000000000000000, -46.87740477351715640, -3.172455868805708956 ) ) ;
#1147 = CARTESIAN_POINT ( 'NONE',  ( 17.99999999999999645, 23.10276247328255650, -118.2656051737067600 ) ) ;
#1149 = AXIS2_PLACEMENT_3D ( 'NONE', #42196, #42420, #12567 ) ;
#1150 = DIRECTION ( 'NONE',  ( -1.000000000000000000, -0.000000000000000000, -0.000000000000000000 ) ) ;
#1151 = FACE_OUTER_BOUND ( 'NONE', #14974, .T. ) ;
#1152 = EDGE_CURVE ( 'NONE', #33231, #25294, #1928, .T. ) ;
#1153 = ORIENTED_EDGE ( 'NONE', *, *, #18819, .F. ) ;
#1154 = LINE ( 'NONE', #28469, #26160 ) ;
#1155 = CARTESIAN_POINT ( 'NONE',  ( 81.15556025174309696, 31.00000000000000000, 27.54985289775053658 ) ) ;
#1156 = CARTESIAN_POINT ( 'NONE',  ( 17.99999999999999645, 0.000000000000000000, 0.000000000000000000 ) ) ;
#1157 = CIRCLE ( 'NONE', #3913, 116.0000000000000000 ) ;
#1158 = ORIENTED_EDGE ( 'NONE', *, *, #7222, .F. ) ;
#1159 = AXIS2_PLACEMENT_3D ( 'NONE', #11232, #4885, #21301 ) ;
#1160 = CARTESIAN_POINT ( 'NONE',  ( -13.43146050690766735, 40.00000000000000000, 27.15249184974963015 ) ) ;
#1161 = ADVANCED_FACE ( 'NONE', ( #39182 ), #28973, .F. ) ;
#1162 = AXIS2_PLACEMENT_3D ( 'NONE', #1977, #1334, #17979 ) ;
#1163 = EDGE_LOOP ( 'NONE', ( #23182, #25027, #39890, #38508 ) ) ;
#1164 = AXIS2_PLACEMENT_3D ( 'NONE', #31098, #1183, #33928 ) ;
#1165 = ORIENTED_EDGE ( 'NONE', *, *, #22144, .F. ) ;
#1166 = DIRECTION ( 'NONE',  ( -1.000000000000000000, 0.000000000000000000, 0.000000000000000000 ) ) ;
#1167 = CYLINDRICAL_SURFACE ( 'NONE', #25601, 2.500000000000000444 ) ;
#1168 = CYLINDRICAL_SURFACE ( 'NONE', #20654, 11.00000000000023448 ) ;
#1169 = AXIS2_PLACEMENT_3D ( 'NONE', #25224, #31311, #41088 ) ;
#1170 = EDGE_CURVE ( 'NONE', #1826, #25635, #19389, .T. ) ;
#1171 = CARTESIAN_POINT ( 'NONE',  ( 17.99999999999999645, 0.000000000000000000, 0.000000000000000000 ) ) ;
#1172 = CIRCLE ( 'NONE', #28380, 59.00000000000000000 ) ;
#1173 = ORIENTED_EDGE ( 'NONE', *, *, #21059, .F. ) ;
#1174 = CARTESIAN_POINT ( 'NONE',  ( 17.99999999999999645, -31.48608500567869584, -0.9019157472707834966 ) ) ;
#1175 = ORIENTED_EDGE ( 'NONE', *, *, #11123, .T. ) ;
#1176 = DIRECTION ( 'NONE',  ( 0.000000000000000000, -0.6845471059286952764, 0.7289686274214054462 ) ) ;
#1177 = FACE_OUTER_BOUND ( 'NONE', #17116, .T. ) ;
#1178 = DIRECTION ( 'NONE',  ( 0.000000000000000000, -0.9996456111234529596, 0.02662052143776450636 ) ) ;
#1179 = CARTESIAN_POINT ( 'NONE',  ( 0.000000000000000000, 27.79676263918187118, 37.88001506494779846 ) ) ;
#1180 = EDGE_LOOP ( 'NONE', ( #17105, #24847, #19897, #18235 ) ) ;
#1181 = EDGE_LOOP ( 'NONE', ( #24173, #32686, #12826, #41645 ) ) ;
#1182 = CYLINDRICAL_SURFACE ( 'NONE', #32194, 15.99999999999998579 ) ;
#1183 = DIRECTION ( 'NONE',  ( 0.000000000000000000, -1.000000000000000000, 5.297542245118643184E-16 ) ) ;
#1184 = EDGE_CURVE ( 'NONE', #19145, #1657, #25354, .T. ) ;
#1185 = ORIENTED_EDGE ( 'NONE', *, *, #14879, .T. ) ;
#1187 = ORIENTED_EDGE ( 'NONE', *, *, #19283, .F. ) ;
#1186 = DIRECTION ( 'NONE',  ( 0.000000000000000000, 0.000000000000000000, 1.000000000000000000 ) ) ;
#1188 = CARTESIAN_POINT ( 'NONE',  ( 14.57966847436265212, 31.00000000000000355, -42.69519604896471776 ) ) ;
#1189 = EDGE_CURVE ( 'NONE', #27145, #20374, #25648, .T. ) ;
#1190 = CARTESIAN_POINT ( 'NONE',  ( -10.00000000000000000, 0.000000000000000000, 0.000000000000000000 ) ) ;
#1191 = AXIS2_PLACEMENT_3D ( 'NONE', #21747, #1610, #28494 ) ;
#1192 = CIRCLE ( 'NONE', #3258, 58.99999999999998579 ) ;
#1193 = CIRCLE ( 'NONE', #25630, 10.99999999999999822 ) ;
#1195 = CARTESIAN_POINT ( 'NONE',  ( -2.107686228591307694E-13, 150.5000000000013642, 10.00000000000041922 ) ) ;
#1194 = LINE ( 'NONE', #27849, #32826 ) ;
#1196 = ORIENTED_EDGE ( 'NONE', *, *, #1926, .F. ) ;
#1197 = CARTESIAN_POINT ( 'NONE',  ( -20.51812799677388455, 40.00000000000000000, -60.74091093256832607 ) ) ;
#1198 = AXIS2_PLACEMENT_3D ( 'NONE', #38100, #11288, #30916 ) ;
#1199 = VECTOR ( 'NONE', #41315, 1000.000000000000000 ) ;
#1200 = ADVANCED_FACE ( 'NONE', ( #6039 ), #15892, .F. ) ;
#1201 = CIRCLE ( 'NONE', #28408, 158.4999999999992042 ) ;
#1202 = DIRECTION ( 'NONE',  ( 1.000000000000000000, 0.000000000000000000, 0.000000000000000000 ) ) ;
#1203 = PRODUCT_DEFINITION_CONTEXT ( 'detailed design', #5815, 'design' ) ;
#1204 = CARTESIAN_POINT ( 'NONE',  ( -10.00000000000000000, 0.000000000000000000, 0.000000000000000000 ) ) ;
#1205 = ORIENTED_EDGE ( 'NONE', *, *, #13432, .T. ) ;
#1206 = DIRECTION ( 'NONE',  ( -1.000000000000000000, 0.000000000000000000, -0.000000000000000000 ) ) ;
#1207 = ADVANCED_FACE ( 'NONE', ( #5817 ), #3387, .F. ) ;
#1208 = ORIENTED_EDGE ( 'NONE', *, *, #35087, .T. ) ;
#1209 = DIRECTION ( 'NONE',  ( 0.000000000000000000, 0.000000000000000000, 1.000000000000000000 ) ) ;
#1210 = DIRECTION ( 'NONE',  ( 1.000000000000000000, 0.000000000000000000, -0.000000000000000000 ) ) ;
#1211 = VECTOR ( 'NONE', #11533, 1000.000000000000000 ) ;
#1212 = CARTESIAN_POINT ( 'NONE',  ( 17.07784400123870938, 31.00000000000000355, -50.31546185293520779 ) ) ;
#1213 = DIRECTION ( 'NONE',  ( 0.000000000000000000, -0.9213119778704087492, -0.3888241754733308131 ) ) ;
#1214 = ORIENTED_EDGE ( 'NONE', *, *, #36823, .T. ) ;
#1215 = PRODUCT_DEFINITION_SHAPE ( 'NONE', 'NONE',  #43215 ) ;
#1216 = DIRECTION ( 'NONE',  ( 1.000000000000000000, 0.000000000000000000, 0.000000000000000000 ) ) ;
#1217 = ORIENTED_EDGE ( 'NONE', *, *, #19654, .T. ) ;
#1218 = EDGE_CURVE ( 'NONE', #29305, #30609, #4032, .T. ) ;
#1219 = CARTESIAN_POINT ( 'NONE',  ( 29.64712525329720449, 40.00000000000000000, -17.12831674356021239 ) ) ;
#1220 = ORIENTED_EDGE ( 'NONE', *, *, #33956, .F. ) ;
#1221 = DIRECTION ( 'NONE',  ( 1.000000000000000000, 0.000000000000000000, 0.000000000000000000 ) ) ;
#1222 = EDGE_CURVE ( 'NONE', #25672, #815, #10160, .T. ) ;
#1223 = DIRECTION ( 'NONE',  ( -1.000000000000000000, -0.000000000000000000, -0.000000000000000000 ) ) ;
#1224 = AXIS2_PLACEMENT_3D ( 'NONE', #2448, #15398, #16029 ) ;
#1225 = CARTESIAN_POINT ( 'NONE',  ( 64.75392801420538547, 31.00000000000000000, -56.64582372546510669 ) ) ;
#1226 = CARTESIAN_POINT ( 'NONE',  ( 42.86165537668587433, 40.00000000000000000, -73.99543480067944756 ) ) ;
#1227 = DIRECTION ( 'NONE',  ( 0.000000000000000000, -0.4132121857683850874, 0.9106347728549100129 ) ) ;
#1228 = AXIS2_PLACEMENT_3D ( 'NONE', #13976, #31198, #33796 ) ;
#1229 = ORIENTED_EDGE ( 'NONE', *, *, #25180, .F. ) ;
#1230 = CARTESIAN_POINT ( 'NONE',  ( 17.99999999999999645, -5.822172717930484964, 31.41458249383138934 ) ) ;
#1231 = VECTOR ( 'NONE', #41233, 1000.000000000000000 ) ;
#1232 = ORIENTED_EDGE ( 'NONE', *, *, #22577, .T. ) ;
#1233 = AXIS2_PLACEMENT_3D ( 'NONE', #17157, #20430, #27832 ) ;
#1234 = FACE_OUTER_BOUND ( 'NONE', #15938, .T. ) ;
#1235 = FACE_OUTER_BOUND ( 'NONE', #41355, .T. ) ;
#1236 = AXIS2_PLACEMENT_3D ( 'NONE', #12534, #4173, #10527 ) ;
#1238 = EDGE_LOOP ( 'NONE', ( #38806, #1010, #34766, #20779 ) ) ;
#1237 = CYLINDRICAL_SURFACE ( 'NONE', #2547, 116.0000000000000000 ) ;
#1239 = CARTESIAN_POINT ( 'NONE',  ( 8.999999999999998224, -12.42760411676061949, 33.78690065568420664 ) ) ;
#1240 = ORIENTED_EDGE ( 'NONE', *, *, #38847, .T. ) ;
#1241 = CARTESIAN_POINT ( 'NONE',  ( 2.290893957444128645E-15, 4.647089433458768681, -3.572167766733382877 ) ) ;
#1242 = CARTESIAN_POINT ( 'NONE',  ( 63.67823170517923614, 39.99999999999999289, 72.58713758494482704 ) ) ;
#1243 = PLANE ( 'NONE',  #19484 ) ;
#1244 = AXIS2_PLACEMENT_3D ( 'NONE', #41617, #5610, #15672 ) ;
#1245 = EDGE_LOOP ( 'NONE', ( #28084, #35112, #6542, #37 ) ) ;
#1246 = EDGE_CURVE ( 'NONE', #6594, #34567, #33508, .T. ) ;
#1247 = CARTESIAN_POINT ( 'NONE',  ( 18.00000000000000355, 0.000000000000000000, 0.000000000000000000 ) ) ;
#1248 = ADVANCED_FACE ( 'NONE', ( #7102 ), #37425, .F. ) ;
#1249 = CYLINDRICAL_SURFACE ( 'NONE', #23927, 116.0000000000000000 ) ;
#1250 = EDGE_CURVE ( 'NONE', #22146, #27962, #27029, .T. ) ;
#1251 = EDGE_CURVE ( 'NONE', #4089, #31991, #23727, .T. ) ;
#1252 = DIRECTION ( 'NONE',  ( -1.000000000000000000, 0.000000000000000000, -0.000000000000000000 ) ) ;
#1253 = EDGE_LOOP ( 'NONE', ( #40270, #15926, #15655, #30488 ) ) ;
#1254 = DIRECTION ( 'NONE',  ( 0.000000000000000000, -0.4132121857683850874, 0.9106347728549100129 ) ) ;
#1255 = EDGE_LOOP ( 'NONE', ( #36454, #18678, #2896, #13801 ) ) ;
#1256 = DIRECTION ( 'NONE',  ( -3.996523416598930318E-16, 2.658563593772947863E-15, 1.000000000000000000 ) ) ;
#1257 = CARTESIAN_POINT ( 'NONE',  ( -29.39530816626169596, 40.00000000000000000, -14.54745122861429252 ) ) ;
#1258 = CARTESIAN_POINT ( 'NONE',  ( -106.4195705685749402, 106.4195705685765745, 7.000000000000337508 ) ) ;
#1259 = VECTOR ( 'NONE', #5273, 1000.000000000000000 ) ;
#1260 = CYLINDRICAL_SURFACE ( 'NONE', #17092, 47.49900000000000233 ) ;
#1261 = DIRECTION ( 'NONE',  ( -3.996523416598930318E-16, 2.658563593772947863E-15, 1.000000000000000000 ) ) ;
#1262 = ORIENTED_EDGE ( 'NONE', *, *, #13717, .T. ) ;
#1263 = AXIS2_PLACEMENT_3D ( 'NONE', #33333, #9330, #12840 ) ;
#1265 = CARTESIAN_POINT ( 'NONE',  ( -0.1404048886732797152, -4.699864953788083888, -3.686887068327043160 ) ) ;
#1264 = CARTESIAN_POINT ( 'NONE',  ( 0.000000000000000000, -106.6051926090974007, 45.73109345704783379 ) ) ;
#1266 = AXIS2_PLACEMENT_3D ( 'NONE', #33038, #13435, #39354 ) ;
#1267 = ORIENTED_EDGE ( 'NONE', *, *, #21003, .T. ) ;
#1268 = VECTOR ( 'NONE', #14046, 1000.000000000000000 ) ;
#1269 = CARTESIAN_POINT ( 'NONE',  ( 17.99999999999999645, 117.6086855750634470, 26.24286718912143712 ) ) ;
#1270 = DIRECTION ( 'NONE',  ( 1.000000000000000000, 0.000000000000000000, 0.000000000000000000 ) ) ;
#1271 = CARTESIAN_POINT ( 'NONE',  ( -4.233603722440171246, 31.00000000000000355, -32.08218167604271542 ) ) ;
#1272 = ORIENTED_EDGE ( 'NONE', *, *, #26632, .F. ) ;
#1273 = DIRECTION ( 'NONE',  ( 1.000000000000000000, 0.000000000000000000, 0.000000000000000000 ) ) ;
#1274 = CIRCLE ( 'NONE', #42337, 31.49900000000000588 ) ;
#1275 = PLANE ( 'NONE',  #36174 ) ;
#1276 = DIRECTION ( 'NONE',  ( 0.000000000000000000, 0.000000000000000000, 1.000000000000000000 ) ) ;
#1277 = CARTESIAN_POINT ( 'NONE',  ( -75.41724699911947027, 31.00000000000000711, 25.61573074746135248 ) ) ;
#1278 = EDGE_CURVE ( 'NONE', #11061, #11670, #23587, .T. ) ;
#1279 = ORIENTED_EDGE ( 'NONE', *, *, #36562, .F. ) ;
#1280 = CARTESIAN_POINT ( 'NONE',  ( 41.62382930724211860, 31.00000000000000355, -20.43270582883756248 ) ) ;
#1281 = CARTESIAN_POINT ( 'NONE',  ( -58.57471716409879292, 40.00000000000000711, 66.78942258476980953 ) ) ;
#1282 = DIRECTION ( 'NONE',  ( 1.000000000000000000, -1.373900992973641868E-15, -3.994789077170585140E-16 ) ) ;
#1283 = CYLINDRICAL_SURFACE ( 'NONE', #38174, 59.00000000000000000 ) ;
#1284 = DIRECTION ( 'NONE',  ( -1.000000000000000000, -0.000000000000000000, -0.000000000000000000 ) ) ;
#1285 = AXIS2_PLACEMENT_3D ( 'NONE', #2931, #42870, #13027 ) ;
#1286 = VECTOR ( 'NONE', #26797, 1000.000000000000000 ) ;
#1288 = ORIENTED_EDGE ( 'NONE', *, *, #14682, .T. ) ;
#1287 = CARTESIAN_POINT ( 'NONE',  ( 17.99999999999999645, 30.01658535635412406, -108.1077105353194838 ) ) ;
#1289 = CARTESIAN_POINT ( 'NONE',  ( -22.00000000000000000, 31.00000000000000355, -7.355690625810191807E-15 ) ) ;
#1290 = CARTESIAN_POINT ( 'NONE',  ( -2.100000000000000089, 2.571758278209441957E-16, -4.694516984716113228 ) ) ;
#1291 = AXIS2_PLACEMENT_3D ( 'NONE', #13178, #29752, #29970 ) ;
#1292 = ORIENTED_EDGE ( 'NONE', *, *, #35237, .T. ) ;
#1293 = CARTESIAN_POINT ( 'NONE',  ( -16.10381281257427943, 40.00000000000000000, -60.09637020943575436 ) ) ;
#1294 = DIRECTION ( 'NONE',  ( -1.000000000000000000, 0.000000000000000000, 0.000000000000000000 ) ) ;
#1295 = DIRECTION ( 'NONE',  ( 1.000000000000000000, -3.035766082959412415E-17, 0.000000000000000000 ) ) ;
#1296 = ORIENTED_EDGE ( 'NONE', *, *, #34658, .F. ) ;
#1297 = LINE ( 'NONE', #14644, #18318 ) ;
#1298 = CYLINDRICAL_SURFACE ( 'NONE', #14562, 36.00000000000000000 ) ;
#1299 = EDGE_CURVE ( 'NONE', #13037, #20999, #3593, .T. ) ;
#1300 = EDGE_CURVE ( 'NONE', #42289, #32276, #30248, .T. ) ;
#1301 = ORIENTED_EDGE ( 'NONE', *, *, #551, .T. ) ;
#1302 = DIRECTION ( 'NONE',  ( 0.000000000000000000, 0.1837495178165707566, -0.9829730996839017854 ) ) ;
#1303 = ORIENTED_EDGE ( 'NONE', *, *, #30038, .T. ) ;
#1304 = EDGE_CURVE ( 'NONE', #37428, #15011, #7754, .T. ) ;
#1305 = CARTESIAN_POINT ( 'NONE',  ( 18.00000000000000355, -39.78933988720132220, 24.98727647984988920 ) ) ;
#1306 = ORIENTED_EDGE ( 'NONE', *, *, #9813, .T. ) ;
#1307 = DIRECTION ( 'NONE',  ( -1.000000000000000000, 0.000000000000000000, 0.000000000000000000 ) ) ;
#1308 = CARTESIAN_POINT ( 'NONE',  ( 8.999999999999998224, 31.94619804602764290, 16.59639811537368814 ) ) ;
#1309 = ORIENTED_EDGE ( 'NONE', *, *, #28423, .T. ) ;
#1310 = DIRECTION ( 'NONE',  ( -3.996523416598930318E-16, 2.658563593772947863E-15, 1.000000000000000000 ) ) ;
#1311 = ADVANCED_FACE ( 'NONE', ( #30890 ), #10828, .T. ) ;
#1312 = CARTESIAN_POINT ( 'NONE',  ( 0.000000000000000000, -53.40478689619659747, -108.0204598100370816 ) ) ;
#1313 = ORIENTED_EDGE ( 'NONE', *, *, #34877, .F. ) ;
#1314 = CARTESIAN_POINT ( 'NONE',  ( 17.99999999999999645, -13.22719389141998825, 28.58720592780592185 ) ) ;
#1315 = DIRECTION ( 'NONE',  ( 1.000000000000000000, 0.000000000000000000, 0.000000000000000000 ) ) ;
#1316 = EDGE_CURVE ( 'NONE', #17266, #6343, #30474, .T. ) ;
#1317 = EDGE_LOOP ( 'NONE', ( #30939, #28167, #23527, #23489 ) ) ;
#1318 = AXIS2_PLACEMENT_3D ( 'NONE', #17445, #4506, #34191 ) ;
#1319 = CYLINDRICAL_SURFACE ( 'NONE', #30831, 59.00000000000000000 ) ;
#1320 = LINE ( 'NONE', #38190, #25849 ) ;
#1321 = CIRCLE ( 'NONE', #6892, 1.000000000000000444 ) ;
#1322 = ORIENTED_EDGE ( 'NONE', *, *, #8182, .F. ) ;
#1323 = CARTESIAN_POINT ( 'NONE',  ( -150.5000000000000284, 1.999999999999996669, 5.277182299893249324E-13 ) ) ;
#1324 = CARTESIAN_POINT ( 'NONE',  ( 9.000000000000001776, 30.03615769709792360, -42.44795908868958634 ) ) ;
#1325 = CARTESIAN_POINT ( 'NONE',  ( 32.65420139560029611, 31.00000000000000355, -42.57517516360295673 ) ) ;
#1326 = VERTEX_POINT ( 'NONE', #40902 ) ;
#1328 = DIRECTION ( 'NONE',  ( 1.000000000000000000, -0.000000000000000000, -0.000000000000000000 ) ) ;
#1327 = CARTESIAN_POINT ( 'NONE',  ( 17.99999999999999645, -25.46650492921910924, 19.29328419707777087 ) ) ;
#1329 = CARTESIAN_POINT ( 'NONE',  ( 17.99999999999999645, -104.2166695095708491, -60.49278301857915352 ) ) ;
#1330 = ORIENTED_EDGE ( 'NONE', *, *, #27210, .T. ) ;
#1331 = CARTESIAN_POINT ( 'NONE',  ( 18.00000000000000355, -43.83938735307280865, 18.28286404005783083 ) ) ;
#1332 = CARTESIAN_POINT ( 'NONE',  ( -38.92335646797288717, 40.00000000000000000, 29.86975225897632313 ) ) ;
#1333 = CARTESIAN_POINT ( 'NONE',  ( -26.81486728383016072, 40.00000000000000000, -46.61672233255473685 ) ) ;
#1334 = DIRECTION ( 'NONE',  ( -1.000000000000000000, -0.000000000000000000, -0.000000000000000000 ) ) ;
#1335 = CARTESIAN_POINT ( 'NONE',  ( 17.99999999999999645, 61.59243992711459015, 93.77976230226062171 ) ) ;
#1336 = CARTESIAN_POINT ( 'NONE',  ( -91.96080130434573618, -35.35525454449571470, 14.45886780445633946 ) ) ;
#1337 = LINE ( 'NONE', #28630, #17622 ) ;
#1338 = ORIENTED_EDGE ( 'NONE', *, *, #20817, .F. ) ;
#1339 = CARTESIAN_POINT ( 'NONE',  ( -38.31599561464027914, 40.00000000000000000, 10.26995502114586678 ) ) ;
#1340 = VERTEX_POINT ( 'NONE', #11056 ) ;
#1341 = CARTESIAN_POINT ( 'NONE',  ( 0.000000000000000000, 39.64889472655730884, 33.64468972902522381 ) ) ;
#1342 = CARTESIAN_POINT ( 'NONE',  ( -1.257172072275743346, 3.892973519171203378, -3.433252694550776862 ) ) ;
#1343 = EDGE_LOOP ( 'NONE', ( #41084, #12283, #18643, #25685 ) ) ;
#1344 = CIRCLE ( 'NONE', #42448, 58.99999999999999289 ) ;
#1345 = CIRCLE ( 'NONE', #25774, 47.49900000000000944 ) ;
#1346 = DIRECTION ( 'NONE',  ( 0.000000000000000000, 0.6382441836448211614, -0.7698339834299053885 ) ) ;
#1347 = EDGE_CURVE ( 'NONE', #36755, #39935, #24383, .T. ) ;
#1348 = DIRECTION ( 'NONE',  ( -1.000000000000000000, -0.000000000000000000, -0.000000000000000000 ) ) ;
#1349 = ORIENTED_EDGE ( 'NONE', *, *, #33619, .F. ) ;
#1350 = DIRECTION ( 'NONE',  ( 0.000000000000000000, 0.8477344278896686847, 0.5304209081197459597 ) ) ;
#1351 = ORIENTED_EDGE ( 'NONE', *, *, #21891, .F. ) ;
#1352 = AXIS2_PLACEMENT_3D ( 'NONE', #10473, #36866, #36639 ) ;
#1353 = ORIENTED_EDGE ( 'NONE', *, *, #34670, .F. ) ;
#1354 = DIRECTION ( 'NONE',  ( 0.000000000000000000, 0.9911528310040076395, -0.1327255272837190025 ) ) ;
#1355 = CARTESIAN_POINT ( 'NONE',  ( -22.66037885604483648, 31.00000000000000355, 66.40833514169634100 ) ) ;
#1356 = EDGE_LOOP ( 'NONE', ( #36830, #1080, #6475, #23716 ) ) ;
#1357 = CARTESIAN_POINT ( 'NONE',  ( -4.000000000000000000, 2.471528634177585282, -3.686887442155186712 ) ) ;
#1358 = EDGE_CURVE ( 'NONE', #37944, #3752, #39471, .T. ) ;
#1359 = DIRECTION ( 'NONE',  ( -1.000000000000000000, 0.000000000000000000, 0.000000000000000000 ) ) ;
#1360 = VERTEX_POINT ( 'NONE', #26983 ) ;
#1361 = EDGE_CURVE ( 'NONE', #7867, #25259, #40258, .T. ) ;
#1362 = DIRECTION ( 'NONE',  ( -1.000000000000000000, 0.000000000000000000, 0.000000000000000000 ) ) ;
#1363 = ORIENTED_EDGE ( 'NONE', *, *, #1409, .F. ) ;
#1364 = CARTESIAN_POINT ( 'NONE',  ( -29.11455967534193334, 40.00000000000000000, 85.38284731560057139 ) ) ;
#1365 = CARTESIAN_POINT ( 'NONE',  ( -1.587008504153756938, 31.00000000000000355, -24.39691638390477380 ) ) ;
#1366 = EDGE_CURVE ( 'NONE', #15009, #26006, #30046, .T. ) ;
#1368 = DIRECTION ( 'NONE',  ( 0.000000000000000000, 0.000000000000000000, 1.000000000000000000 ) ) ;
#1367 = CARTESIAN_POINT ( 'NONE',  ( 0.000000000000000000, 0.000000000000000000, 0.000000000000000000 ) ) ;
#1369 = CARTESIAN_POINT ( 'NONE',  ( 106.4195705685741302, 106.4195705685767166, 6.999999999999998224 ) ) ;
#1370 = DIRECTION ( 'NONE',  ( 0.000000000000000000, 0.000000000000000000, 1.000000000000000000 ) ) ;
#1371 = ORIENTED_EDGE ( 'NONE', *, *, #9764, .F. ) ;
#1372 =( NAMED_UNIT ( * ) PLANE_ANGLE_UNIT ( ) SI_UNIT ( $, .RADIAN. ) );
#1373 = FILL_AREA_STYLE ('',( #25619 ) ) ;
#1374 = CIRCLE ( 'NONE', #17434, 20.00000000000000711 ) ;
#1375 = ORIENTED_EDGE ( 'NONE', *, *, #11380, .F. ) ;
#1376 = CARTESIAN_POINT ( 'NONE',  ( 6.075999999999997847, 0.000000000000000000, 0.000000000000000000 ) ) ;
#1377 = AXIS2_PLACEMENT_3D ( 'NONE', #15007, #24843, #38308 ) ;
#1378 = FACE_OUTER_BOUND ( 'NONE', #24533, .T. ) ;
#1379 = CARTESIAN_POINT ( 'NONE',  ( -10.00000000000000000, 0.000000000000000000, 0.000000000000000000 ) ) ;
#1380 = EDGE_LOOP ( 'NONE', ( #24309, #27972, #18983, #30106 ) ) ;
#1381 = CARTESIAN_POINT ( 'NONE',  ( 26.62151981922250243, 40.00000000000000000, -3.482817046706076169 ) ) ;
#1382 = EDGE_CURVE ( 'NONE', #11528, #32977, #36990, .T. ) ;
#1383 = VERTEX_POINT ( 'NONE', #10602 ) ;
#1384 = ORIENTED_EDGE ( 'NONE', *, *, #40939, .F. ) ;
#1385 = CARTESIAN_POINT ( 'NONE',  ( 0.000000000000000000, 0.000000000000000000, 0.000000000000000000 ) ) ;
#1386 = CARTESIAN_POINT ( 'NONE',  ( -5.991980000000000750, 0.000000000000000000, 0.000000000000000000 ) ) ;
#1387 = CYLINDRICAL_SURFACE ( 'NONE', #37984, 59.00000000000000000 ) ;
#1388 = DIRECTION ( 'NONE',  ( 1.000000000000000000, 0.000000000000000000, 0.000000000000000000 ) ) ;
#1389 = ORIENTED_EDGE ( 'NONE', *, *, #13360, .T. ) ;
#1390 = DIRECTION ( 'NONE',  ( -0.000000000000000000, -0.000000000000000000, 1.000000000000000000 ) ) ;
#1391 = ORIENTED_EDGE ( 'NONE', *, *, #30943, .F. ) ;
#1392 = DIRECTION ( 'NONE',  ( 0.000000000000000000, 0.000000000000000000, -1.000000000000000000 ) ) ;
#1393 = FACE_BOUND ( 'NONE', #25323, .T. ) ;
#1394 = DIRECTION ( 'NONE',  ( 1.000000000000000000, 0.000000000000000000, 0.000000000000000000 ) ) ;
#1395 = DIRECTION ( 'NONE',  ( 1.000000000000000000, 0.000000000000000000, 0.000000000000000000 ) ) ;
#1396 = VERTEX_POINT ( 'NONE', #26758 ) ;
#1397 = ORIENTED_EDGE ( 'NONE', *, *, #35387, .T. ) ;
#1398 = FACE_OUTER_BOUND ( 'NONE', #30424, .T. ) ;
#1399 = PLANE ( 'NONE',  #19376 ) ;
#1400 = AXIS2_PLACEMENT_3D ( 'NONE', #34444, #15066, #14847 ) ;
#1401 = VERTEX_POINT ( 'NONE', #40030 ) ;
#1403 = ORIENTED_EDGE ( 'NONE', *, *, #24830, .F. ) ;
#1402 = CARTESIAN_POINT ( 'NONE',  ( -15.99999999999997691, 17.11489954122026447, 5.571627607371296764E-15 ) ) ;
#1404 = AXIS2_PLACEMENT_3D ( 'NONE', #10594, #6881, #3377 ) ;
#1405 = CARTESIAN_POINT ( 'NONE',  ( -40.27082278477694643, 31.00000000000000355, 10.71261860272906397 ) ) ;
#1406 = AXIS2_PLACEMENT_3D ( 'NONE', #30781, #21002, #41434 ) ;
#1407 = CARTESIAN_POINT ( 'NONE',  ( 0.000000000000000000, 31.17727234463848163, -111.7317219465816862 ) ) ;
#1408 = AXIS2_PLACEMENT_3D ( 'NONE', #15972, #42962, #8970 ) ;
#1409 = EDGE_CURVE ( 'NONE', #30643, #17666, #40880, .T. ) ;
#1411 = LINE ( 'NONE', #41324, #24064 ) ;
#1410 = CARTESIAN_POINT ( 'NONE',  ( 17.99999999999999645, 116.0452958106480708, 32.46506308663498430 ) ) ;
#1412 = ORIENTED_EDGE ( 'NONE', *, *, #33372, .F. ) ;
#1413 = LINE ( 'NONE', #4915, #35985 ) ;
#1414 = CARTESIAN_POINT ( 'NONE',  ( 66.37122006405570573, 39.99999999999999289, -8.639838683448301637 ) ) ;
#1415 = DIRECTION ( 'NONE',  ( 1.000000000000000000, 0.000000000000000000, 0.000000000000000000 ) ) ;
#1416 = EDGE_CURVE ( 'NONE', #42813, #631, #22192, .T. ) ;
#1417 = FACE_OUTER_BOUND ( 'NONE', #14128, .T. ) ;
#1418 = VERTEX_POINT ( 'NONE', #8834 ) ;
#1419 = DIRECTION ( 'NONE',  ( -1.000000000000000000, 0.000000000000000000, -0.000000000000000000 ) ) ;
#1420 = ORIENTED_EDGE ( 'NONE', *, *, #21705, .F. ) ;
#1421 = SURFACE_STYLE_USAGE ( .BOTH. , #38079 ) ;
#1422 = DIRECTION ( 'NONE',  ( 1.000000000000000000, 0.000000000000000000, -6.546126324440832913E-16 ) ) ;
#1423 = CARTESIAN_POINT ( 'NONE',  ( 9.000000000000001776, -13.56094713063538038, -50.20060470671754160 ) ) ;
#1424 = CIRCLE ( 'NONE', #27206, 11.08000000000000007 ) ;
#1425 = CARTESIAN_POINT ( 'NONE',  ( -27.38011802910879311, 31.00000000000000355, -55.51905197969063011 ) ) ;
#1426 = DIRECTION ( 'NONE',  ( 0.9247238835424298475, 0.000000000000000000, 0.3806385939525924744 ) ) ;
#1427 = ORIENTED_EDGE ( 'NONE', *, *, #7222, .T. ) ;
#1428 = CARTESIAN_POINT ( 'NONE',  ( 17.99999999999999645, -29.68570942776479527, 10.53307442156924267 ) ) ;
#1429 = ADVANCED_FACE ( 'NONE', ( #35226 ), #28513, .T. ) ;
#1430 = AXIS2_PLACEMENT_3D ( 'NONE', #39969, #23881, #37145 ) ;
#1431 = EDGE_LOOP ( 'NONE', ( #35385, #15024, #20016, #15168 ) ) ;
#1432 = CARTESIAN_POINT ( 'NONE',  ( -6.599999999999997868, 20.00000000000000000, 0.000000000000000000 ) ) ;
#1433 = ADVANCED_FACE ( 'NONE', ( #34584 ), #41777, .F. ) ;
#1434 = CARTESIAN_POINT ( 'NONE',  ( 17.99999999999999645, -31.48608500567871005, 0.9019157472703476230 ) ) ;
#1435 = CARTESIAN_POINT ( 'NONE',  ( 83.01093309086799366, 31.00000000000000000, 28.30804032755801458 ) ) ;
#1436 = CARTESIAN_POINT ( 'NONE',  ( -59.98614492175870794, 40.00000000000000711, 68.21249229748744369 ) ) ;
#1437 = VECTOR ( 'NONE', #37464, 1000.000000000000000 ) ;
#1438 = CYLINDRICAL_SURFACE ( 'NONE', #16743, 36.00000000000000000 ) ;
#1439 = ORIENTED_EDGE ( 'NONE', *, *, #28050, .T. ) ;
#1440 = DIRECTION ( 'NONE',  ( -1.000000000000000000, 0.000000000000000000, 0.000000000000000000 ) ) ;
#1441 = VERTEX_POINT ( 'NONE', #7969 ) ;
#1442 = DIRECTION ( 'NONE',  ( 0.1305261922200494362, 0.9914448613738107152, 0.000000000000000000 ) ) ;
#1443 = DIRECTION ( 'NONE',  ( 1.000000000000000000, 0.000000000000000000, 0.000000000000000000 ) ) ;
#1445 = VERTEX_POINT ( 'NONE', #25245 ) ;
#1444 = CARTESIAN_POINT ( 'NONE',  ( 17.99999999999999645, -16.86122981692000167, -27.13802899033310112 ) ) ;
#1446 = DIRECTION ( 'NONE',  ( -1.000000000000000000, -0.000000000000000000, -0.000000000000000000 ) ) ;
#1447 = ORIENTED_EDGE ( 'NONE', *, *, #10542, .F. ) ;
#1448 = CARTESIAN_POINT ( 'NONE',  ( 17.99999999999999645, -76.48293397876204835, -82.08917884620389316 ) ) ;
#1449 = CARTESIAN_POINT ( 'NONE',  ( -99.89583333318432778, 40.00000000000000711, 6.544984695199788760 ) ) ;
#1450 = CYLINDRICAL_SURFACE ( 'NONE', #14595, 59.00000000000000000 ) ;
#1451 = VERTEX_POINT ( 'NONE', #27857 ) ;
#1452 = DIRECTION ( 'NONE',  ( 3.009274222672345096E-17, 1.000000000000000000, -2.455023325076455345E-18 ) ) ;
#1453 = CARTESIAN_POINT ( 'NONE',  ( 17.99999999999999645, 0.000000000000000000, 0.000000000000000000 ) ) ;
#1454 = CIRCLE ( 'NONE', #18933, 2.649999999999979039 ) ;
#1455 = ADVANCED_FACE ( 'NONE', ( #11264 ), #35019, .F. ) ;
#1457 = CARTESIAN_POINT ( 'NONE',  ( -10.00000000000000000, 0.000000000000000000, 0.000000000000000000 ) ) ;
#1456 = DIRECTION ( 'NONE',  ( 1.000000000000000000, 0.000000000000000000, 0.000000000000000000 ) ) ;
#1458 = VERTEX_POINT ( 'NONE', #41111 ) ;
#1459 = DIRECTION ( 'NONE',  ( 0.000000000000000000, 0.000000000000000000, -1.000000000000000000 ) ) ;
#1461 = ORIENTED_EDGE ( 'NONE', *, *, #17602, .T. ) ;
#1460 = AXIS2_PLACEMENT_3D ( 'NONE', #22396, #26282, #32380 ) ;
#1462 = DIRECTION ( 'NONE',  ( 1.000000000000000000, 0.000000000000000000, 0.000000000000000000 ) ) ;
#1463 = CARTESIAN_POINT ( 'NONE',  ( -15.23573235977941032, 40.00000000000000000, 26.30445775087293114 ) ) ;
#1464 = FACE_OUTER_BOUND ( 'NONE', #33238, .T. ) ;
#1465 = AXIS2_PLACEMENT_3D ( 'NONE', #42756, #39917, #17079 ) ;
#1466 = EDGE_CURVE ( 'NONE', #2965, #37680, #15217, .T. ) ;
#1467 = CARTESIAN_POINT ( 'NONE',  ( 0.000000000000000000, -34.45183346761142928, 10.44371441202643247 ) ) ;
#1468 = VECTOR ( 'NONE', #2507, 1000.000000000000000 ) ;
#1469 = EDGE_CURVE ( 'NONE', #15044, #4662, #21969, .T. ) ;
#1470 = DIRECTION ( 'NONE',  ( 1.000000000000000000, 0.000000000000000000, -6.546126324440850663E-16 ) ) ;
#1471 = ORIENTED_EDGE ( 'NONE', *, *, #31671, .F. ) ;
#1473 = PLANE ( 'NONE',  #40141 ) ;
#1472 = LINE ( 'NONE', #24883, #10518 ) ;
#1474 = ORIENTED_EDGE ( 'NONE', *, *, #10997, .F. ) ;
#1475 = CIRCLE ( 'NONE', #9143, 158.5000000000000284 ) ;
#1476 = DIRECTION ( 'NONE',  ( 1.000000000000000000, 0.000000000000000000, 0.000000000000000000 ) ) ;
#1477 = CARTESIAN_POINT ( 'NONE',  ( 0.000000000000000000, 0.000000000000000000, 0.000000000000000000 ) ) ;
#1478 = CARTESIAN_POINT ( 'NONE',  ( -1.799870782497340782, 31.00000000000000355, 27.60416666422008802 ) ) ;
#1479 = VERTEX_POINT ( 'NONE', #41978 ) ;
#1480 = DIRECTION ( 'NONE',  ( 0.000000000000000000, -0.9822872507286903865, 0.1873813145857149975 ) ) ;
#1481 = CARTESIAN_POINT ( 'NONE',  ( 17.99999999999999645, 0.000000000000000000, 0.000000000000000000 ) ) ;
#1482 = CARTESIAN_POINT ( 'NONE',  ( 0.000000000000000000, 0.000000000000000000, 0.000000000000000000 ) ) ;
#1483 = CIRCLE ( 'NONE', #31467, 47.49900000000000233 ) ;
#1484 = CARTESIAN_POINT ( 'NONE',  ( -77.84600223180727596, 31.00000000000000711, -20.84395318355897686 ) ) ;
#1485 = EDGE_CURVE ( 'NONE', #40340, #3463, #1630, .T. ) ;
#1486 = ADVANCED_FACE ( 'NONE', ( #34809 ), #31977, .F. ) ;
#1487 = VERTEX_POINT ( 'NONE', #25449 ) ;
#1488 = CARTESIAN_POINT ( 'NONE',  ( 43.74200748489511881, 31.00000000000000355, 38.49442098324159645 ) ) ;
#1489 = EDGE_CURVE ( 'NONE', #27244, #29070, #11648, .T. ) ;
#1490 = EDGE_CURVE ( 'NONE', #40777, #23134, #15822, .T. ) ;
#1491 = CARTESIAN_POINT ( 'NONE',  ( 6.054110834496887250, 40.00000000000000000, -92.60416666599778068 ) ) ;
#1492 = VERTEX_POINT ( 'NONE', #28714 ) ;
#1493 = AXIS2_PLACEMENT_3D ( 'NONE', #14709, #28451, #34754 ) ;
#1494 = CARTESIAN_POINT ( 'NONE',  ( 2.500000000000000000, -1.178949249685218748, -2.041999999999998039 ) ) ;
#1495 = AXIS2_PLACEMENT_3D ( 'NONE', #18764, #1256, #11313 ) ;
#1496 = CARTESIAN_POINT ( 'NONE',  ( 17.99999999999999645, 31.11570115861495367, 4.898994019976747438 ) ) ;
#1497 = CARTESIAN_POINT ( 'NONE',  ( 2.500000000000000000, 1.768423874527822459, -1.021000000000002794 ) ) ;
#1498 = AXIS2_PLACEMENT_3D ( 'NONE', #12904, #5900, #29925 ) ;
#1500 = ORIENTED_EDGE ( 'NONE', *, *, #16941, .F. ) ;
#1499 = DIRECTION ( 'NONE',  ( -1.000000000000000000, 0.000000000000000000, -0.000000000000000000 ) ) ;
#1501 = DIRECTION ( 'NONE',  ( -1.000000000000000000, 0.000000000000000000, 0.000000000000000000 ) ) ;
#1502 = CARTESIAN_POINT ( 'NONE',  ( 17.99999999999999645, -47.58001226230612701, 110.7096808509482031 ) ) ;
#1503 = ORIENTED_EDGE ( 'NONE', *, *, #25146, .T. ) ;
#1504 = CARTESIAN_POINT ( 'NONE',  ( -8.856203846296160975, 40.00000000000000000, 67.27320953167645712 ) ) ;
#1505 = CARTESIAN_POINT ( 'NONE',  ( 17.99999999999999645, -0.04937522221144796664, 31.94951095880159997 ) ) ;
#1506 = AXIS2_PLACEMENT_3D ( 'NONE', #23245, #29347, #42409 ) ;
#1507 = VERTEX_POINT ( 'NONE', #21334 ) ;
#1508 = CARTESIAN_POINT ( 'NONE',  ( 17.99999999999999645, -14.84191762912296930, -27.78316904333141224 ) ) ;
#1509 = CARTESIAN_POINT ( 'NONE',  ( -12.69999999999999929, 0.000000000000000000, 0.000000000000000000 ) ) ;
#1510 = VERTEX_POINT ( 'NONE', #38709 ) ;
#1511 = DIRECTION ( 'NONE',  ( -1.000000000000000000, -0.000000000000000000, -0.000000000000000000 ) ) ;
#1512 = ORIENTED_EDGE ( 'NONE', *, *, #39526, .T. ) ;
#1513 = EDGE_CURVE ( 'NONE', #34370, #34755, #40157, .T. ) ;
#1514 = FACE_OUTER_BOUND ( 'NONE', #30875, .T. ) ;
#1515 = ORIENTED_EDGE ( 'NONE', *, *, #36276, .F. ) ;
#1516 = DIRECTION ( 'NONE',  ( 1.000000000000000000, -0.000000000000000000, -0.000000000000000000 ) ) ;
#1517 = CARTESIAN_POINT ( 'NONE',  ( 6.386360208629405122, 31.00000000000000355, 99.40013590833048340 ) ) ;
#1518 = EDGE_LOOP ( 'NONE', ( #6252, #2651, #27456, #24851 ) ) ;
#1519 = EDGE_CURVE ( 'NONE', #13726, #7950, #22815, .T. ) ;
#1520 = CARTESIAN_POINT ( 'NONE',  ( 17.99999999999999645, 116.0452958106484971, -32.46506308663343532 ) ) ;
#1521 = CARTESIAN_POINT ( 'NONE',  ( 0.000000000000000000, 0.000000000000000000, 0.000000000000000000 ) ) ;
#1522 = ORIENTED_EDGE ( 'NONE', *, *, #5733, .T. ) ;
#1523 = DIRECTION ( 'NONE',  ( -3.996523416598930318E-16, 2.658563593772947863E-15, 1.000000000000000000 ) ) ;
#1524 = AXIS2_PLACEMENT_3D ( 'NONE', #27752, #41012, #11160 ) ;
#1525 = VECTOR ( 'NONE', #20373, 1000.000000000000000 ) ;
#1526 = DIRECTION ( 'NONE',  ( 0.000000000000000000, 0.000000000000000000, 1.000000000000000000 ) ) ;
#1527 = ORIENTED_EDGE ( 'NONE', *, *, #23327, .T. ) ;
#1528 = CARTESIAN_POINT ( 'NONE',  ( -10.00000000000000000, 0.000000000000000000, 0.000000000000000000 ) ) ;
#1529 = AXIS2_PLACEMENT_3D ( 'NONE', #17939, #37941, #11353 ) ;
#1530 = CYLINDRICAL_SURFACE ( 'NONE', #23575, 116.0000000000000000 ) ;
#1531 = PRODUCT_CONTEXT ( 'NONE', #24534, 'mechanical' ) ;
#1532 = CARTESIAN_POINT ( 'NONE',  ( 0.000000000000000000, 12.30077720129167851, -50.52416135122069107 ) ) ;
#1533 = CARTESIAN_POINT ( 'NONE',  ( 23.39270017067629936, 31.00000000000000355, 40.49502024156475244 ) ) ;
#1534 = CIRCLE ( 'NONE', #41238, 58.99999999999999289 ) ;
#1535 = ORIENTED_EDGE ( 'NONE', *, *, #4676, .T. ) ;
#1537 = CARTESIAN_POINT ( 'NONE',  ( 9.000000000000001776, 18.53613841426788511, 48.58406706613909876 ) ) ;
#1536 = DIRECTION ( 'NONE',  ( 1.000000000000000000, -0.000000000000000000, 0.000000000000000000 ) ) ;
#1538 = DIRECTION ( 'NONE',  ( 0.000000000000000000, -0.2486898871648415832, -0.9685831611286344067 ) ) ;
#1539 = ADVANCED_FACE ( 'NONE', ( #18278 ), #14551, .T. ) ;
#1540 = VERTEX_POINT ( 'NONE', #31542 ) ;
#1541 = ADVANCED_FACE ( 'NONE', ( #38072 ), #21560, .F. ) ;
#1542 = EDGE_CURVE ( 'NONE', #10322, #22974, #16546, .T. ) ;
#1543 = FACE_BOUND ( 'NONE', #40820, .T. ) ;
#1544 = CARTESIAN_POINT ( 'NONE',  ( -46.87443272357899815, 40.00000000000000000, 35.96965017775951878 ) ) ;
#1545 = CARTESIAN_POINT ( 'NONE',  ( -59.63693792272297856, 40.00000000000000711, 15.87187584492933823 ) ) ;
#1546 = EDGE_CURVE ( 'NONE', #21840, #276, #30548, .T. ) ;
#1547 = ADVANCED_BREP_SHAPE_REPRESENTATION ( '', ( #14024, #13552 ), #23928 ) ;
#1548 = DIRECTION ( 'NONE',  ( 1.000000000000000000, 0.000000000000000000, 0.000000000000000000 ) ) ;
#1549 = CARTESIAN_POINT ( 'NONE',  ( 17.99999999999999645, -31.81777574834303124, 10.70123563439434733 ) ) ;
#1550 = EDGE_CURVE ( 'NONE', #42889, #32412, #38089, .T. ) ;
#1551 = CARTESIAN_POINT ( 'NONE',  ( -3.983177536951265640, -13.66651769228263191, -1.199999999999999956 ) ) ;
#1552 = CARTESIAN_POINT ( 'NONE',  ( 7.411374251232441424, 31.00000000000000355, -21.84767871671174788 ) ) ;
#1553 = VECTOR ( 'NONE', #41674, 1000.000000000000000 ) ;
#1554 = ORIENTED_EDGE ( 'NONE', *, *, #26625, .F. ) ;
#1555 = CARTESIAN_POINT ( 'NONE',  ( 20.45440555730427690, 40.00000000000000000, -26.67302265141799467 ) ) ;
#1556 = VERTEX_POINT ( 'NONE', #2685 ) ;
#1557 = FACE_OUTER_BOUND ( 'NONE', #26440, .T. ) ;
#1558 = DIRECTION ( 'NONE',  ( 0.000000000000000000, 0.000000000000000000, 1.000000000000000000 ) ) ;
#1559 = VECTOR ( 'NONE', #8751, 1000.000000000000000 ) ;
#1560 = ORIENTED_EDGE ( 'NONE', *, *, #1735, .F. ) ;
#1561 = CARTESIAN_POINT ( 'NONE',  ( 0.000000000000000000, 0.000000000000000000, 0.000000000000000000 ) ) ;
#1562 = AXIS2_PLACEMENT_3D ( 'NONE', #17234, #10209, #40722 ) ;
#1563 = FACE_OUTER_BOUND ( 'NONE', #19348, .T. ) ;
#1564 = VERTEX_POINT ( 'NONE', #12986 ) ;
#1565 = CARTESIAN_POINT ( 'NONE',  ( 0.000000000000000000, 7.162210897276451327, -51.50439529848821252 ) ) ;
#1566 = VERTEX_POINT ( 'NONE', #25670 ) ;
#1567 = CIRCLE ( 'NONE', #7140, 139.5000000000000000 ) ;
#1568 = VERTEX_POINT ( 'NONE', #39563 ) ;
#1569 = CYLINDRICAL_SURFACE ( 'NONE', #11124, 58.99999999999999289 ) ;
#1570 = CARTESIAN_POINT ( 'NONE',  ( -31.21560191380782001, 31.00000000000000355, 63.07420938637471863 ) ) ;
#1571 = ORIENTED_EDGE ( 'NONE', *, *, #22036, .T. ) ;
#1572 = CARTESIAN_POINT ( 'NONE',  ( -4.000000000000000000, 0.8576368993457507139, -3.433240632782198709 ) ) ;
#1573 = EDGE_CURVE ( 'NONE', #20690, #32792, #39134, .T. ) ;
#1574 = FACE_OUTER_BOUND ( 'NONE', #28406, .T. ) ;
#1575 = VERTEX_POINT ( 'NONE', #9693 ) ;
#1576 = CARTESIAN_POINT ( 'NONE',  ( -91.96080130434580724, -40.05525454449572464, 14.45886780445738218 ) ) ;
#1577 = ORIENTED_EDGE ( 'NONE', *, *, #5048, .F. ) ;
#1578 = CARTESIAN_POINT ( 'NONE',  ( 72.29027477046881245, 39.99999999999999289, -63.25088587038124643 ) ) ;
#1579 = CARTESIAN_POINT ( 'NONE',  ( -101.1468392228030098, 40.00000000000000711, 13.20405500234329921 ) ) ;
#1581 = CARTESIAN_POINT ( 'NONE',  ( 17.99999999999999645, -0.04937522221144796664, 31.94951095880159997 ) ) ;
#1580 = CARTESIAN_POINT ( 'NONE',  ( 17.99999999999999645, -67.32409792376564894, 89.75376489259340929 ) ) ;
#1582 = CARTESIAN_POINT ( 'NONE',  ( 17.99999999999999645, 88.00363688980654331, -82.31555682352568226 ) ) ;
#1583 = DIRECTION ( 'NONE',  ( -1.000000000000000000, -0.000000000000000000, -0.000000000000000000 ) ) ;
#1584 = ORIENTED_EDGE ( 'NONE', *, *, #35545, .T. ) ;
#1585 = CIRCLE ( 'NONE', #25992, 59.00000000000000711 ) ;
#1586 = FACE_OUTER_BOUND ( 'NONE', #37622, .T. ) ;
#1587 = VERTEX_POINT ( 'NONE', #32607 ) ;
#1588 = CARTESIAN_POINT ( 'NONE',  ( 0.000000000000000000, 117.6086855750638165, -26.24286718911982774 ) ) ;
#1589 = CYLINDRICAL_SURFACE ( 'NONE', #29710, 59.00000000000000000 ) ;
#1590 = DIRECTION ( 'NONE',  ( 1.000000000000000000, 0.000000000000000000, 0.000000000000000000 ) ) ;
#1591 = EDGE_LOOP ( 'NONE', ( #7231, #22635, #19798, #19757 ) ) ;
#1592 = CIRCLE ( 'NONE', #22536, 120.5010000000000190 ) ;
#1593 = EDGE_CURVE ( 'NONE', #38742, #16728, #32617, .T. ) ;
#1594 = CARTESIAN_POINT ( 'NONE',  ( -3.169834189307653816, 40.00000000000000000, -24.13593742708953727 ) ) ;
#1595 = EDGE_CURVE ( 'NONE', #28016, #28450, #25874, .T. ) ;
#1596 = CIRCLE ( 'NONE', #19055, 120.5010000000000332 ) ;
#1597 = ORIENTED_EDGE ( 'NONE', *, *, #33469, .T. ) ;
#1598 = ORIENTED_EDGE ( 'NONE', *, *, #28032, .T. ) ;
#1599 = DIRECTION ( 'NONE',  ( 0.000000000000000000, 0.000000000000000000, 1.000000000000000000 ) ) ;
#1600 = CARTESIAN_POINT ( 'NONE',  ( 9.000000000000001776, -44.25018368420724357, -27.31155879685227106 ) ) ;
#1601 = CARTESIAN_POINT ( 'NONE',  ( 17.99999999999999645, -95.38615066514023511, 59.07414607872794932 ) ) ;
#1602 = DIRECTION ( 'NONE',  ( -1.000000000000000000, -0.000000000000000000, -0.000000000000000000 ) ) ;
#1603 = EDGE_CURVE ( 'NONE', #22368, #7685, #16049, .T. ) ;
#1604 = ORIENTED_EDGE ( 'NONE', *, *, #24927, .F. ) ;
#1605 = DIRECTION ( 'NONE',  ( -1.000000000000000000, 0.000000000000000000, -0.000000000000000000 ) ) ;
#1606 = VERTEX_POINT ( 'NONE', #5979 ) ;
#1607 = DIRECTION ( 'NONE',  ( 0.000000000000000000, 1.423061292157245201E-14, -1.000000000000000000 ) ) ;
#1608 = CYLINDRICAL_SURFACE ( 'NONE', #41636, 36.00000000000000000 ) ;
#1609 = ADVANCED_FACE ( 'NONE', ( #26289 ), #5564, .T. ) ;
#1610 = DIRECTION ( 'NONE',  ( -1.000000000000000000, -0.000000000000000000, 0.000000000000000000 ) ) ;
#1611 = DIRECTION ( 'NONE',  ( -0.000000000000000000, -0.000000000000000000, 1.000000000000000000 ) ) ;
#1612 = ORIENTED_EDGE ( 'NONE', *, *, #24949, .T. ) ;
#1613 = VERTEX_POINT ( 'NONE', #18921 ) ;
#1614 = LINE ( 'NONE', #25028, #22451 ) ;
#1615 = CARTESIAN_POINT ( 'NONE',  ( 8.999999999999998224, -83.58328028049608349, -80.43528614701409651 ) ) ;
#1616 = CIRCLE ( 'NONE', #23243, 120.5010000000000190 ) ;
#1617 = VERTEX_POINT ( 'NONE', #16258 ) ;
#1619 = VERTEX_POINT ( 'NONE', #19753 ) ;
#1618 = CYLINDRICAL_SURFACE ( 'NONE', #16685, 120.5010000000000190 ) ;
#1620 = CARTESIAN_POINT ( 'NONE',  ( 41.62382930724211860, 31.00000000000000355, -20.43270582883756248 ) ) ;
#1621 = ORIENTED_EDGE ( 'NONE', *, *, #34799, .T. ) ;
#1622 = CARTESIAN_POINT ( 'NONE',  ( 8.999999999999998224, -48.55277268144258329, -105.3500273609084843 ) ) ;
#1623 =( GEOMETRIC_REPRESENTATION_CONTEXT ( 3 ) GLOBAL_UNCERTAINTY_ASSIGNED_CONTEXT ( ( #40903 ) ) GLOBAL_UNIT_ASSIGNED_CONTEXT ( ( #23045, #2897, #33672 ) ) REPRESENTATION_CONTEXT ( 'NONE', 'WORKASPACE' ) );
#1625 =( LENGTH_UNIT ( ) NAMED_UNIT ( * ) SI_UNIT ( .MILLI., .METRE. ) );
#1624 = FACE_OUTER_BOUND ( 'NONE', #41541, .T. ) ;
#1626 = VERTEX_POINT ( 'NONE', #16479 ) ;
#1627 = DIRECTION ( 'NONE',  ( -1.000000000000000000, 0.000000000000000000, -0.000000000000000000 ) ) ;
#1629 = CARTESIAN_POINT ( 'NONE',  ( -38.62815422673675414, 40.00000000000000000, -50.51519254952906124 ) ) ;
#1628 = VECTOR ( 'NONE', #12194, 1000.000000000000000 ) ;
#1630 = LINE ( 'NONE', #18719, #34602 ) ;
#1631 = CARTESIAN_POINT ( 'NONE',  ( 17.99999999999999645, -97.19627249181141337, 71.22763238166453448 ) ) ;
#1632 = VERTEX_POINT ( 'NONE', #42825 ) ;
#1633 = DIRECTION ( 'NONE',  ( 0.000000000000000000, 0.000000000000000000, 1.000000000000000000 ) ) ;
#1634 = AXIS2_PLACEMENT_3D ( 'NONE', #30829, #3526, #20184 ) ;
#1635 = ORIENTED_EDGE ( 'NONE', *, *, #34762, .F. ) ;
#1636 =( NAMED_UNIT ( * ) PLANE_ANGLE_UNIT ( ) SI_UNIT ( $, .RADIAN. ) );
#1637 = DIRECTION ( 'NONE',  ( 0.000000000000000000, 0.000000000000000000, 1.000000000000000000 ) ) ;
#1638 = CARTESIAN_POINT ( 'NONE',  ( 0.000000000000000000, 0.000000000000000000, 6.999999999999998224 ) ) ;
#1639 = AXIS2_PLACEMENT_3D ( 'NONE', #41736, #34977, #25208 ) ;
#1640 = CARTESIAN_POINT ( 'NONE',  ( 33.41571365387085280, 31.00000000000000355, 57.85165222247763239 ) ) ;
#1641 = DIRECTION ( 'NONE',  ( -1.000000000000000000, -0.000000000000000000, 0.000000000000000000 ) ) ;
#1642 = ORIENTED_EDGE ( 'NONE', *, *, #28139, .T. ) ;
#1643 = AXIS2_PLACEMENT_3D ( 'NONE', #34065, #36296, #17735 ) ;
#1644 = EDGE_CURVE ( 'NONE', #36379, #2044, #19323, .T. ) ;
#1645 = EDGE_CURVE ( 'NONE', #20720, #16577, #30447, .T. ) ;
#1646 = DIRECTION ( 'NONE',  ( -1.000000000000000000, -0.000000000000000000, -0.000000000000000000 ) ) ;
#1647 = VECTOR ( 'NONE', #26840, 1000.000000000000000 ) ;
#1648 = ORIENTED_EDGE ( 'NONE', *, *, #10294, .F. ) ;
#1649 = DIRECTION ( 'NONE',  ( -1.000000000000000000, -0.000000000000000000, 0.000000000000000000 ) ) ;
#1650 = DIRECTION ( 'NONE',  ( -1.000000000000000000, 0.000000000000000000, 0.000000000000000000 ) ) ;
#1651 = CARTESIAN_POINT ( 'NONE',  ( 69.92891852055319646, 31.00000000000000000, 53.79372986807582180 ) ) ;
#1652 = CARTESIAN_POINT ( 'NONE',  ( 83.01093309090690298, 39.99999999999999289, 28.30804032753857058 ) ) ;
#1653 = FACE_OUTER_BOUND ( 'NONE', #7306, .T. ) ;
#1654 = EDGE_CURVE ( 'NONE', #20992, #25205, #27692, .T. ) ;
#1655 = VERTEX_POINT ( 'NONE', #33020 ) ;
#1656 = CARTESIAN_POINT ( 'NONE',  ( 17.99999999999999645, -110.0562500189195561, -49.07252625220223052 ) ) ;
#1657 = VERTEX_POINT ( 'NONE', #2471 ) ;
#1658 = CARTESIAN_POINT ( 'NONE',  ( 17.99999999999999645, 27.24480646643607074, 15.80846360676594564 ) ) ;
#1659 = EDGE_CURVE ( 'NONE', #14903, #38713, #36091, .T. ) ;
#1660 = CARTESIAN_POINT ( 'NONE',  ( 17.99999999999999645, -89.07460286905796920, -81.15544420875052367 ) ) ;
#1662 = ORIENTED_EDGE ( 'NONE', *, *, #26038, .F. ) ;
#1661 = CARTESIAN_POINT ( 'NONE',  ( 9.000000000000000000, -18.42432724429453827, -30.92804820216021611 ) ) ;
#1663 = CARTESIAN_POINT ( 'NONE',  ( 0.000000000000000000, -107.2885202478262556, -54.86040852957423652 ) ) ;
#1664 = VERTEX_POINT ( 'NONE', #29142 ) ;
#1665 = DIRECTION ( 'NONE',  ( 1.000000000000000000, 0.000000000000000000, 0.000000000000000000 ) ) ;
#1666 = AXIS2_PLACEMENT_3D ( 'NONE', #22494, #18373, #5015 ) ;
#1667 = CARTESIAN_POINT ( 'NONE',  ( -12.08748825390017068, 40.00000000000000000, -91.69541640458645304 ) ) ;
#1668 = DIRECTION ( 'NONE',  ( -1.000000000000000000, -0.000000000000000000, -0.000000000000000000 ) ) ;
#1669 = VECTOR ( 'NONE', #942, 1000.000000000000000 ) ;
#1670 = ORIENTED_EDGE ( 'NONE', *, *, #29679, .T. ) ;
#1671 = DIRECTION ( 'NONE',  ( 0.000000000000000000, -6.887872625202028030E-15, 1.000000000000000000 ) ) ;
#1672 = DIRECTION ( 'NONE',  ( -1.000000000000000000, 0.000000000000000000, 0.000000000000000000 ) ) ;
#1673 = CIRCLE ( 'NONE', #5167, 11.00000000000023803 ) ;
#1675 = DIRECTION ( 'NONE',  ( 0.000000000000000000, 0.000000000000000000, 1.000000000000000000 ) ) ;
#1674 = DIRECTION ( 'NONE',  ( -1.000000000000000000, -0.000000000000000000, -0.000000000000000000 ) ) ;
#1676 = CIRCLE ( 'NONE', #21230, 116.0000000000000000 ) ;
#1677 = VERTEX_POINT ( 'NONE', #42410 ) ;
#1678 = DIRECTION ( 'NONE',  ( 0.000000000000000000, 0.000000000000000000, 1.000000000000000000 ) ) ;
#1680 = VERTEX_POINT ( 'NONE', #36080 ) ;
#1679 = EDGE_CURVE ( 'NONE', #1587, #16211, #9474, .T. ) ;
#1681 = DIRECTION ( 'NONE',  ( 0.000000000000000000, 0.000000000000000000, 1.000000000000000000 ) ) ;
#1682 = CARTESIAN_POINT ( 'NONE',  ( -23.27229071022945561, 40.00000000000000000, 20.35677778009942074 ) ) ;
#1683 = CYLINDRICAL_SURFACE ( 'NONE', #42445, 59.00000000000000000 ) ;
#1684 = EDGE_CURVE ( 'NONE', #28176, #33446, #6198, .T. ) ;
#1685 = CYLINDRICAL_SURFACE ( 'NONE', #31197, 59.00000000000000000 ) ;
#1686 = CARTESIAN_POINT ( 'NONE',  ( 0.000000000000000000, -68.63002662989811142, 93.51962064069482494 ) ) ;
#1687 = ORIENTED_EDGE ( 'NONE', *, *, #18227, .T. ) ;
#1689 = LINE ( 'NONE', #38134, #22089 ) ;
#1688 = PRODUCT_DEFINITION_FORMATION_WITH_SPECIFIED_SOURCE ( 'ANY', '', #42610, .NOT_KNOWN. ) ;
#1690 = VERTEX_POINT ( 'NONE', #39770 ) ;
#1691 = CIRCLE ( 'NONE', #6532, 20.00000000000000711 ) ;
#1692 = LINE ( 'NONE', #4529, #37119 ) ;
#1693 = CARTESIAN_POINT ( 'NONE',  ( 0.000000000000000000, -63.55543939553702160, -97.03971415477388973 ) ) ;
#1694 = CARTESIAN_POINT ( 'NONE',  ( -5.542584477697039880, 31.00000000000000355, -42.01772079774592328 ) ) ;
#1695 = ORIENTED_EDGE ( 'NONE', *, *, #28401, .T. ) ;
#1696 = DIRECTION ( 'NONE',  ( 0.000000000000000000, 0.000000000000000000, 1.000000000000000000 ) ) ;
#1697 = AXIS2_PLACEMENT_3D ( 'NONE', #25090, #12178, #11967 ) ;
#1698 = AXIS2_PLACEMENT_3D ( 'NONE', #14434, #8719, #5019 ) ;
#1699 = DIRECTION ( 'NONE',  ( -1.000000000000000000, -0.000000000000000000, -0.000000000000000000 ) ) ;
#1700 = CARTESIAN_POINT ( 'NONE',  ( -5.072363130230006512, 31.00000000000000355, 77.60416666578095146 ) ) ;
#1701 = EDGE_LOOP ( 'NONE', ( #4047, #40782, #39916, #41488 ) ) ;
#1702 = CARTESIAN_POINT ( 'NONE',  ( -38.36856355434107257, 31.00000000000000355, 33.53830235993100217 ) ) ;
#1703 = VECTOR ( 'NONE', #42041, 1000.000000000000000 ) ;
#1704 = CARTESIAN_POINT ( 'NONE',  ( 38.45889818826288575, 40.00000000000000000, 77.98987599019784511 ) ) ;
#1705 = EDGE_CURVE ( 'NONE', #13925, #12177, #32177, .T. ) ;
#1706 = EDGE_CURVE ( 'NONE', #19229, #32995, #9544, .T. ) ;
#1707 = AXIS2_PLACEMENT_3D ( 'NONE', #31150, #34618, #793 ) ;
#1708 = EDGE_LOOP ( 'NONE', ( #10398, #37993, #11211, #26932 ) ) ;
#1709 = CARTESIAN_POINT ( 'NONE',  ( -3.983177536951265640, -13.66651769228263191, 0.000000000000000000 ) ) ;
#1710 = DIRECTION ( 'NONE',  ( 0.000000000000000000, 0.000000000000000000, 1.000000000000000000 ) ) ;
#1711 = EDGE_CURVE ( 'NONE', #14485, #3869, #3242, .T. ) ;
#1712 = DIRECTION ( 'NONE',  ( 0.000000000000000000, 0.8477344278896721264, -0.5304209081197405196 ) ) ;
#1714 = ORIENTED_EDGE ( 'NONE', *, *, #33506, .T. ) ;
#1713 = DIRECTION ( 'NONE',  ( 0.000000000000000000, 0.000000000000000000, 1.000000000000000000 ) ) ;
#1715 = CARTESIAN_POINT ( 'NONE',  ( 9.000000000000001776, 35.78484819117785776, -110.3423972910429143 ) ) ;
#1716 = CARTESIAN_POINT ( 'NONE',  ( 18.00000000000000355, -30.93515269692137792, 36.04401931830242489 ) ) ;
#1717 = AXIS2_PLACEMENT_3D ( 'NONE', #37382, #7499, #20862 ) ;
#1718 = ORIENTED_EDGE ( 'NONE', *, *, #8640, .F. ) ;
#1719 = CARTESIAN_POINT ( 'NONE',  ( -59.82155519081633344, 40.00000000000000711, -7.874468279900277423 ) ) ;
#1720 = FACE_OUTER_BOUND ( 'NONE', #13675, .T. ) ;
#1721 = ORIENTED_EDGE ( 'NONE', *, *, #16760, .T. ) ;
#1722 = DIRECTION ( 'NONE',  ( -1.000000000000000000, 0.000000000000000000, 0.000000000000000000 ) ) ;
#1723 = DIRECTION ( 'NONE',  ( -1.000000000000000000, 0.000000000000000000, 0.000000000000000000 ) ) ;
#1724 = CLOSED_SHELL ( 'NONE', ( #33748, #24407, #157, #36662, #5189, #23558, #390, #13764, #40052, #859, #36455, #9652, #29855, #18232, #42688, #39745, #11732, #908, #27872, #4463, #1907, #5772, #22328, #14283, #29088, #39216, #37250, #35865 ) ) ;
#1725 = CYLINDRICAL_SURFACE ( 'NONE', #26329, 116.0000000000000000 ) ;
#1726 = ORIENTED_EDGE ( 'NONE', *, *, #15773, .T. ) ;
#1727 = AXIS2_PLACEMENT_3D ( 'NONE', #22337, #26009, #32324 ) ;
#1728 = ORIENTED_EDGE ( 'NONE', *, *, #8593, .F. ) ;
#1729 = LINE ( 'NONE', #38809, #31640 ) ;
#1730 = ORIENTED_EDGE ( 'NONE', *, *, #21825, .T. ) ;
#1731 = VECTOR ( 'NONE', #38363, 1000.000000000000000 ) ;
#1732 = CARTESIAN_POINT ( 'NONE',  ( 17.99999999999999645, -51.27532863109303918, -99.79535634195178773 ) ) ;
#1733 = LINE ( 'NONE', #25556, #7441 ) ;
#1734 = EDGE_CURVE ( 'NONE', #26760, #12939, #15154, .T. ) ;
#1735 = EDGE_CURVE ( 'NONE', #14587, #36747, #28482, .T. ) ;
#1736 = CYLINDRICAL_SURFACE ( 'NONE', #17061, 51.99999999999999289 ) ;
#1737 = DIRECTION ( 'NONE',  ( 0.000000000000000000, 0.000000000000000000, 1.000000000000000000 ) ) ;
#1738 = VERTEX_POINT ( 'NONE', #36723 ) ;
#1739 = FACE_OUTER_BOUND ( 'NONE', #12587, .T. ) ;
#1740 = AXIS2_PLACEMENT_3D ( 'NONE', #15647, #2288, #29380 ) ;
#1741 = B_SPLINE_CURVE_WITH_KNOTS ( 'NONE', 3,
 ( #35894, #5599, #29597, #12170, #36120, #28962 ),
 .UNSPECIFIED., .F., .F.,
 ( 4, 2, 4 ),
 ( 0.000000000000000000, 0.0002095117440854740156, 0.0004190234881709480313 ),
 .UNSPECIFIED. ) ;
#1742 = DIRECTION ( 'NONE',  ( 0.000000000000000000, -5.351180891996252112E-15, -1.000000000000000000 ) ) ;
#1743 = ORIENTED_EDGE ( 'NONE', *, *, #6496, .F. ) ;
#1744 = CARTESIAN_POINT ( 'NONE',  ( 0.000000000000000000, 0.000000000000000000, -20.00000000000000000 ) ) ;
#1745 = DIRECTION ( 'NONE',  ( 0.000000000000000000, 0.000000000000000000, 1.000000000000000000 ) ) ;
#1746 = DIRECTION ( 'NONE',  ( 0.7071067811865561215, -6.123233995736766036E-17, 0.7071067811865389130 ) ) ;
#1747 = EDGE_CURVE ( 'NONE', #10605, #21443, #549, .T. ) ;
#1748 = DIRECTION ( 'NONE',  ( 1.000000000000000000, 0.000000000000000000, 0.000000000000000000 ) ) ;
#1749 = EDGE_CURVE ( 'NONE', #5647, #37373, #5403, .T. ) ;
#1750 = CARTESIAN_POINT ( 'NONE',  ( -50.10416666532988472, 31.00000000000000355, -3.272492339034341224 ) ) ;
#1751 = VERTEX_POINT ( 'NONE', #27579 ) ;
#1753 = DIRECTION ( 'NONE',  ( -1.000000000000000000, 0.000000000000000000, 0.000000000000000000 ) ) ;
#1752 = DIRECTION ( 'NONE',  ( -1.000000000000000000, 0.000000000000000000, 0.000000000000000000 ) ) ;
#1755 = ORIENTED_EDGE ( 'NONE', *, *, #12188, .F. ) ;
#1754 = AXIS2_PLACEMENT_3D ( 'NONE', #12987, #22608, #29997 ) ;
#1756 = AXIS2_PLACEMENT_3D ( 'NONE', #34470, #27963, #14657 ) ;
#1757 = CARTESIAN_POINT ( 'NONE',  ( -51.34291522965900612, 40.00000000000000000, 29.65708359768123970 ) ) ;
#1758 = CONICAL_SURFACE ( 'NONE', #26878, 4.000000000000000000, 0.8911886515913786111 ) ;
#1759 = CARTESIAN_POINT ( 'NONE',  ( 32.82854187708761629, 40.00000000000000000, -56.64543409044760125 ) ) ;
#1760 = AXIS2_PLACEMENT_3D ( 'NONE', #28995, #11618, #11837 ) ;
#1761 = EDGE_CURVE ( 'NONE', #39524, #24229, #29802, .T. ) ;
#1762 = AXIS2_PLACEMENT_3D ( 'NONE', #27667, #30279, #789 ) ;
#1763 = DIRECTION ( 'NONE',  ( 1.000000000000000000, 0.000000000000000000, 0.000000000000000000 ) ) ;
#1764 = VECTOR ( 'NONE', #23522, 1000.000000000000000 ) ;
#1765 = LINE ( 'NONE', #32517, #6772 ) ;
#1766 = EDGE_CURVE ( 'NONE', #20507, #33396, #18698, .T. ) ;
#1767 = CIRCLE ( 'NONE', #21326, 20.00000000000000711 ) ;
#1768 = DIRECTION ( 'NONE',  ( -1.000000000000000000, -0.000000000000000000, 0.000000000000000000 ) ) ;
#1769 = CARTESIAN_POINT ( 'NONE',  ( 23.79574588541966662, 31.00000000000000355, -6.380716493563439506 ) ) ;
#1770 = AXIS2_PLACEMENT_3D ( 'NONE', #19960, #39540, #42804 ) ;
#1771 = ORIENTED_EDGE ( 'NONE', *, *, #632, .T. ) ;
#1772 = CARTESIAN_POINT ( 'NONE',  ( 10.63353083439206870, 40.00000000000000000, -31.33693976183458219 ) ) ;
#1773 = ORIENTED_EDGE ( 'NONE', *, *, #5212, .F. ) ;
#1774 = CARTESIAN_POINT ( 'NONE',  ( 9.000000000000001776, -115.6826031496112677, 8.575274253897077870 ) ) ;
#1775 = CYLINDRICAL_SURFACE ( 'NONE', #29863, 59.00000000000000000 ) ;
#1776 = ORIENTED_EDGE ( 'NONE', *, *, #7769, .F. ) ;
#1777 = DIRECTION ( 'NONE',  ( 1.000000000000000000, 0.000000000000000000, 0.000000000000000000 ) ) ;
#1778 = CARTESIAN_POINT ( 'NONE',  ( -139.5000000000000000, 0.000000000000000000, -20.00000000000000000 ) ) ;
#1779 = ORIENTED_EDGE ( 'NONE', *, *, #39181, .T. ) ;
#1780 = DIRECTION ( 'NONE',  ( -1.000000000000000000, -0.000000000000000000, -0.000000000000000000 ) ) ;
#1781 = ORIENTED_EDGE ( 'NONE', *, *, #20661, .T. ) ;
#1782 = VERTEX_POINT ( 'NONE', #39977 ) ;
#1783 = DIRECTION ( 'NONE',  ( 0.000000000000000000, 0.000000000000000000, 1.000000000000000000 ) ) ;
#1784 = EDGE_CURVE ( 'NONE', #3612, #28259, #36711, .T. ) ;
#1785 = CARTESIAN_POINT ( 'NONE',  ( -74.30604906370724905, 31.00000000000000711, -36.76128443491435860 ) ) ;
#1786 = VERTEX_POINT ( 'NONE', #29995 ) ;
#1787 = CARTESIAN_POINT ( 'NONE',  ( 17.99999999999999645, -6.486220790507708500, -112.0098273076987994 ) ) ;
#1788 = EDGE_CURVE ( 'NONE', #40221, #1575, #38128, .T. ) ;
#1789 = AXIS2_PLACEMENT_3D ( 'NONE', #21509, #5299, #5514 ) ;
#1790 = EDGE_CURVE ( 'NONE', #7217, #33553, #19352, .T. ) ;
#1791 = EDGE_CURVE ( 'NONE', #5484, #37859, #483, .T. ) ;
#1792 = DIRECTION ( 'NONE',  ( -1.000000000000000000, -0.000000000000000000, -0.000000000000000000 ) ) ;
#1793 = EDGE_LOOP ( 'NONE', ( #14472, #36351, #5138, #29212 ) ) ;
#1794 = AXIS2_PLACEMENT_3D ( 'NONE', #23744, #37015, #33964 ) ;
#1795 = DIRECTION ( 'NONE',  ( 0.000000000000000000, 0.3641605752528230266, -0.9313361774523382097 ) ) ;
#1796 = CARTESIAN_POINT ( 'NONE',  ( -6.638544827991895048, 40.00000000000000000, 99.59190654106264162 ) ) ;
#1797 = CARTESIAN_POINT ( 'NONE',  ( -14.30682334061562067, 31.00000000000000355, -18.65445469299708492 ) ) ;
#1799 = DIRECTION ( 'NONE',  ( 0.000000000000000000, 0.000000000000000000, 1.000000000000000000 ) ) ;
#1798 = DIRECTION ( 'NONE',  ( -1.000000000000000000, 0.000000000000000000, 0.000000000000000000 ) ) ;
#1800 = AXIS2_PLACEMENT_3D ( 'NONE', #38039, #25013, #7935 ) ;
#1801 = DIRECTION ( 'NONE',  ( -1.000000000000000000, -0.000000000000000000, 0.000000000000000000 ) ) ;
#1802 = CARTESIAN_POINT ( 'NONE',  ( 18.00000000000000355, 50.95304419620824632, 10.38206564895679307 ) ) ;
#1803 = ORIENTED_EDGE ( 'NONE', *, *, #38011, .T. ) ;
#1804 = SURFACE_STYLE_USAGE ( .BOTH. , #18872 ) ;
#1805 = AXIS2_PLACEMENT_3D ( 'NONE', #6929, #17448, #20081 ) ;
#1806 = DIRECTION ( 'NONE',  ( 0.000000000000000000, 0.4132121857683790922, -0.9106347728549127885 ) ) ;
#1807 = EDGE_LOOP ( 'NONE', ( #11294, #17144 ) ) ;
#1808 = DIRECTION ( 'NONE',  ( -1.000000000000000000, 0.000000000000000000, -0.000000000000000000 ) ) ;
#1809 = CARTESIAN_POINT ( 'NONE',  ( -94.39576909109665337, 31.00000000000000711, 32.06004391471374504 ) ) ;
#1810 = DIRECTION ( 'NONE',  ( 0.000000000000000000, 0.000000000000000000, -1.000000000000000000 ) ) ;
#1811 = ORIENTED_EDGE ( 'NONE', *, *, #1382, .T. ) ;
#1812 = CARTESIAN_POINT ( 'NONE',  ( -18.66214908251097881, 40.00000000000000000, 24.25811346063289164 ) ) ;
#1813 = ORIENTED_EDGE ( 'NONE', *, *, #7774, .T. ) ;
#1814 = VERTEX_POINT ( 'NONE', #3544 ) ;
#1815 = DIRECTION ( 'NONE',  ( 0.000000000000000000, 0.000000000000000000, -1.000000000000000000 ) ) ;
#1816 = CYLINDRICAL_SURFACE ( 'NONE', #15838, 31.49899999999999878 ) ;
#1818 = FACE_OUTER_BOUND ( 'NONE', #13046, .T. ) ;
#1817 = VECTOR ( 'NONE', #39641, 1000.000000000000000 ) ;
#1819 = CARTESIAN_POINT ( 'NONE',  ( 17.99999999999999645, 56.51398178981825993, 96.92493144647468739 ) ) ;
#1820 = VECTOR ( 'NONE', #22340, 1000.000000000000000 ) ;
#1821 = VECTOR ( 'NONE', #36180, 1000.000000000000000 ) ;
#1822 = AXIS2_PLACEMENT_3D ( 'NONE', #3123, #23058, #3356 ) ;
#1823 = DIRECTION ( 'NONE',  ( 0.000000000000000000, 0.000000000000000000, 1.000000000000000000 ) ) ;
#1824 = ORIENTED_EDGE ( 'NONE', *, *, #37060, .F. ) ;
#1825 = DIRECTION ( 'NONE',  ( -1.000000000000000000, 0.000000000000000000, -0.000000000000000000 ) ) ;
#1826 = VERTEX_POINT ( 'NONE', #26708 ) ;
#1827 = CARTESIAN_POINT ( 'NONE',  ( 21.00000000000000355, 0.000000000000000000, 0.000000000000000000 ) ) ;
#1828 = DIRECTION ( 'NONE',  ( -1.000000000000000000, -0.000000000000000000, -0.000000000000000000 ) ) ;
#1829 = TOROIDAL_SURFACE ( 'NONE', #8128, 19.11697999999999809, 0.08401999999999931745 ) ;
#1830 = AXIS2_PLACEMENT_3D ( 'NONE', #32331, #15999, #41930 ) ;
#1831 = AXIS2_PLACEMENT_3D ( 'NONE', #34391, #17651, #21143 ) ;
#1832 = CARTESIAN_POINT ( 'NONE',  ( 0.000000000000000000, 38.92705108641732181, 27.21837053747810486 ) ) ;
#1833 = DIRECTION ( 'NONE',  ( -1.000000000000000000, -0.000000000000000000, 0.000000000000000000 ) ) ;
#1834 = VERTEX_POINT ( 'NONE', #16918 ) ;
#1835 = ORIENTED_EDGE ( 'NONE', *, *, #5889, .T. ) ;
#1836 = CARTESIAN_POINT ( 'NONE',  ( -10.00000000000000000, 0.000000000000000000, 0.000000000000000000 ) ) ;
#1837 = CARTESIAN_POINT ( 'NONE',  ( 18.00000000000000355, 0.000000000000000000, 0.000000000000000000 ) ) ;
#1838 = CIRCLE ( 'NONE', #22774, 4.500000000000000888 ) ;
#1839 = VERTEX_POINT ( 'NONE', #30200 ) ;
#1841 = ORIENTED_EDGE ( 'NONE', *, *, #1734, .F. ) ;
#1840 = CYLINDRICAL_SURFACE ( 'NONE', #32683, 2.500000000000000444 ) ;
#1842 = CARTESIAN_POINT ( 'NONE',  ( -5.264430561742837078, 31.00000000000000355, 39.44269128747090747 ) ) ;
#1843 = ORIENTED_EDGE ( 'NONE', *, *, #23082, .T. ) ;
#1844 = CARTESIAN_POINT ( 'NONE',  ( 9.000000000000001776, 6.854627147198713466, 115.7972974066013734 ) ) ;
#1845 = CIRCLE ( 'NONE', #26244, 52.00000000000000000 ) ;
#1846 = EDGE_CURVE ( 'NONE', #7063, #33557, #17971, .T. ) ;
#1847 = EDGE_CURVE ( 'NONE', #28966, #22227, #259, .T. ) ;
#1848 = CARTESIAN_POINT ( 'NONE',  ( -4.000000000000000000, 0.3987449864459974846, -0.01220643443059782861 ) ) ;
#1849 = EDGE_CURVE ( 'NONE', #13721, #23787, #23523, .T. ) ;
#1850 = ORIENTED_EDGE ( 'NONE', *, *, #38700, .F. ) ;
#1851 = CARTESIAN_POINT ( 'NONE',  ( -53.44803860755722269, 40.00000000000000000, 46.73995993581220176 ) ) ;
#1852 = DIRECTION ( 'NONE',  ( -1.000000000000000000, -0.000000000000000000, 0.000000000000000000 ) ) ;
#1853 = EDGE_CURVE ( 'NONE', #23198, #41127, #30420, .T. ) ;
#1854 = CARTESIAN_POINT ( 'NONE',  ( 0.000000000000000000, 0.5156212287294736907, -112.1962860721878315 ) ) ;
#1856 = VERTEX_POINT ( 'NONE', #24106 ) ;
#1855 = AXIS2_PLACEMENT_3D ( 'NONE', #27043, #40312, #13954 ) ;
#1857 = CARTESIAN_POINT ( 'NONE',  ( 0.000000000000000000, -63.24564713401861837, 102.5693868539693341 ) ) ;
#1858 = VERTEX_POINT ( 'NONE', #20857 ) ;
#1859 = AXIS2_PLACEMENT_3D ( 'NONE', #12679, #347, #35759 ) ;
#1860 = CARTESIAN_POINT ( 'NONE',  ( 17.99999999999999645, 0.000000000000000000, 0.000000000000000000 ) ) ;
#1861 = LINE ( 'NONE', #41783, #36631 ) ;
#1862 = EDGE_CURVE ( 'NONE', #2165, #22806, #9572, .T. ) ;
#1863 = CARTESIAN_POINT ( 'NONE',  ( 49.83821931962687302, 31.00000000000000355, 43.70611527624207326 ) ) ;
#1864 = CYLINDRICAL_SURFACE ( 'NONE', #10730, 36.00000000000000000 ) ;
#1865 = ORIENTED_EDGE ( 'NONE', *, *, #32961, .F. ) ;
#1867 = CIRCLE ( 'NONE', #3928, 100.0000000000000711 ) ;
#1866 = DIRECTION ( 'NONE',  ( 0.000000000000000000, -0.5076658003388467844, 0.8615540813938020737 ) ) ;
#1868 = AXIS2_PLACEMENT_3D ( 'NONE', #20455, #33716, #13903 ) ;
#1869 = ORIENTED_EDGE ( 'NONE', *, *, #10489, .T. ) ;
#1870 = CARTESIAN_POINT ( 'NONE',  ( 0.000000000000000000, -111.2721026680459602, -14.38025178762732104 ) ) ;
#1871 = CARTESIAN_POINT ( 'NONE',  ( -31.74999999999995737, 5.204748896376250699E-16, -4.250000000000000000 ) ) ;
#1872 = CARTESIAN_POINT ( 'NONE',  ( 66.32976035609178211, 31.00000000000000000, 58.33333674018341952 ) ) ;
#1873 = CARTESIAN_POINT ( 'NONE',  ( 78.79907178679739843, 39.99999999999999289, 38.97904116291323362 ) ) ;
#1874 = DIRECTION ( 'NONE',  ( -1.000000000000000000, -0.000000000000000000, -0.000000000000000000 ) ) ;
#1875 = ADVANCED_FACE ( 'NONE', ( #10771 ), #41062, .F. ) ;
#1876 = EDGE_LOOP ( 'NONE', ( #31239, #28384, #15885, #12832 ) ) ;
#1877 = CYLINDRICAL_SURFACE ( 'NONE', #15876, 59.00000000000000000 ) ;
#1878 = ORIENTED_EDGE ( 'NONE', *, *, #22280, .T. ) ;
#1879 = DIRECTION ( 'NONE',  ( 0.000000000000000000, -1.224646799147338663E-16, 1.000000000000000000 ) ) ;
#1880 = CIRCLE ( 'NONE', #41625, 20.00000000000000711 ) ;
#1882 = ORIENTED_EDGE ( 'NONE', *, *, #1133, .F. ) ;
#1881 = CARTESIAN_POINT ( 'NONE',  ( -17.77999999999999758, 0.000000000000000000, 14.99999999999999822 ) ) ;
#1883 = DIRECTION ( 'NONE',  ( 0.000000000000000000, 0.5528000653611888637, 0.8333139190825179510 ) ) ;
#1884 = ORIENTED_EDGE ( 'NONE', *, *, #31822, .F. ) ;
#1885 = DIRECTION ( 'NONE',  ( 1.000000000000000000, 0.000000000000000000, 0.000000000000000000 ) ) ;
#1886 = CIRCLE ( 'NONE', #13069, 2.649999999999985700 ) ;
#1887 = CARTESIAN_POINT ( 'NONE',  ( 18.00000000000000355, -45.78515115856051665, 12.64416602183649374 ) ) ;
#1888 = AXIS2_PLACEMENT_3D ( 'NONE', #35141, #2178, #24725 ) ;
#1889 = ORIENTED_EDGE ( 'NONE', *, *, #29827, .F. ) ;
#1890 = DIRECTION ( 'NONE',  ( 0.000000000000000000, 0.000000000000000000, 1.000000000000000000 ) ) ;
#1891 = CARTESIAN_POINT ( 'NONE',  ( 0.000000000000000000, 0.000000000000000000, 6.999999999999998224 ) ) ;
#1892 = CIRCLE ( 'NONE', #7469, 47.49900000000000233 ) ;
#1893 = EDGE_CURVE ( 'NONE', #15044, #36592, #15853, .T. ) ;
#1895 = DIRECTION ( 'NONE',  ( 0.000000000000000000, 0.000000000000000000, 1.000000000000000000 ) ) ;
#1894 = DIRECTION ( 'NONE',  ( 1.000000000000000000, 0.000000000000000000, 0.000000000000000000 ) ) ;
#1896 = EDGE_LOOP ( 'NONE', ( #11436, #40390, #32204, #905 ) ) ;
#1897 = CYLINDRICAL_SURFACE ( 'NONE', #19187, 20.00000000000000711 ) ;
#1898 = ORIENTED_EDGE ( 'NONE', *, *, #38041, .T. ) ;
#1899 = FACE_OUTER_BOUND ( 'NONE', #32104, .T. ) ;
#1900 = CARTESIAN_POINT ( 'NONE',  ( 33.88265278290065652, 40.00000000000000000, 16.77599488388066007 ) ) ;
#1901 = CARTESIAN_POINT ( 'NONE',  ( 17.99999999999999645, -111.1352304691226607, -15.40237066878709449 ) ) ;
#1902 = ADVANCED_FACE ( 'NONE', ( #18230 ), #11652, .T. ) ;
#1903 = CARTESIAN_POINT ( 'NONE',  ( 17.99999999999999645, 112.1702510623870097, 2.471285140324554153 ) ) ;
#1904 = CARTESIAN_POINT ( 'NONE',  ( 17.99999999999999645, 2.007101075699966763, 31.43498920425970411 ) ) ;
#1905 = EDGE_LOOP ( 'NONE', ( #41869, #18159, #28124, #17802 ) ) ;
#1906 = CYLINDRICAL_SURFACE ( 'NONE', #39428, 116.0000000000000000 ) ;
#1907 = ADVANCED_FACE ( 'NONE', ( #4413 ), #18019, .F. ) ;
#1908 = EDGE_LOOP ( 'NONE', ( #29076, #35836, #6519, #20696 ) ) ;
#1909 = LINE ( 'NONE', #17682, #19718 ) ;
#1910 = LINE ( 'NONE', #38348, #33814 ) ;
#1911 = ADVANCED_FACE ( 'NONE', ( #37800 ), #11005, .T. ) ;
#1912 = CARTESIAN_POINT ( 'NONE',  ( -20.88694679984194380, 31.00000000000000355, -36.15586224631631751 ) ) ;
#1914 = ORIENTED_EDGE ( 'NONE', *, *, #17311, .T. ) ;
#1913 = AXIS2_PLACEMENT_3D ( 'NONE', #19735, #32996, #26904 ) ;
#1915 = AXIS2_PLACEMENT_3D ( 'NONE', #6755, #173, #42960 ) ;
#1916 = CIRCLE ( 'NONE', #30499, 20.00000000000000000 ) ;
#1917 = LINE ( 'NONE', #18341, #1703 ) ;
#1918 = CARTESIAN_POINT ( 'NONE',  ( 10.12401712103624263, 31.00000000000000355, 76.79210772277129138 ) ) ;
#1919 = AXIS2_PLACEMENT_3D ( 'NONE', #28460, #29089, #38444 ) ;
#1920 = AXIS2_PLACEMENT_3D ( 'NONE', #13229, #22634, #26102 ) ;
#1921 = ORIENTED_EDGE ( 'NONE', *, *, #11316, .T. ) ;
#1923 = CARTESIAN_POINT ( 'NONE',  ( -48.87578956997907653, 31.00000000000000355, 16.50293044076727611 ) ) ;
#1922 = VECTOR ( 'NONE', #17544, 1000.000000000000000 ) ;
#1924 = CARTESIAN_POINT ( 'NONE',  ( -44.26264085331523290, 40.00000000000000711, 76.66224561666088277 ) ) ;
#1925 = ORIENTED_EDGE ( 'NONE', *, *, #28284, .T. ) ;
#1926 = EDGE_CURVE ( 'NONE', #26169, #28773, #7919, .T. ) ;
#1927 = DIRECTION ( 'NONE',  ( -1.734723475976807341E-16, 1.000000000000000000, 0.000000000000000000 ) ) ;
#1928 = CIRCLE ( 'NONE', #26344, 120.5010000000000190 ) ;
#1929 = DIRECTION ( 'NONE',  ( -1.000000000000000000, 0.000000000000000000, -0.000000000000000000 ) ) ;
#1930 = DIRECTION ( 'NONE',  ( 1.000000000000000000, 0.000000000000000000, 0.000000000000000000 ) ) ;
#1932 = VERTEX_POINT ( 'NONE', #31699 ) ;
#1931 = FACE_OUTER_BOUND ( 'NONE', #23917, .T. ) ;
#1933 = DIRECTION ( 'NONE',  ( -1.000000000000000000, -0.000000000000000000, -0.000000000000000000 ) ) ;
#1934 = CARTESIAN_POINT ( 'NONE',  ( 1.317756351988342622, -3.857995168970215438, -0.04852650426602527628 ) ) ;
#1935 = ORIENTED_EDGE ( 'NONE', *, *, #31361, .T. ) ;
#1936 = CARTESIAN_POINT ( 'NONE',  ( -51.86900026051868196, 40.00000000000000000, 45.50549606403863123 ) ) ;
#1937 = DIRECTION ( 'NONE',  ( 0.000000000000000000, 0.000000000000000000, 1.000000000000000000 ) ) ;
#1938 = ORIENTED_EDGE ( 'NONE', *, *, #18657, .T. ) ;
#1939 = CIRCLE ( 'NONE', #17377, 13.59999999999999787 ) ;
#1940 = CARTESIAN_POINT ( 'NONE',  ( 0.000000000000000000, 0.000000000000000000, 0.000000000000000000 ) ) ;
#1941 = DIRECTION ( 'NONE',  ( -1.000000000000000000, 0.000000000000000000, 0.000000000000000000 ) ) ;
#1942 = DIRECTION ( 'NONE',  ( 1.000000000000000000, 0.000000000000000000, 0.000000000000000000 ) ) ;
#1943 = ORIENTED_EDGE ( 'NONE', *, *, #4066, .F. ) ;
#1944 = AXIS2_PLACEMENT_3D ( 'NONE', #29688, #36411, #36632 ) ;
#1945 = ADVANCED_FACE ( 'NONE', ( #18436 ), #5075, .F. ) ;
#1946 = CIRCLE ( 'NONE', #31930, 120.5010000000000190 ) ;
#1947 = ORIENTED_EDGE ( 'NONE', *, *, #31855, .F. ) ;
#1948 = VECTOR ( 'NONE', #35399, 1000.000000000000000 ) ;
#1949 = DIRECTION ( 'NONE',  ( 0.000000000000000000, 0.000000000000000000, 1.000000000000000000 ) ) ;
#1950 = EDGE_LOOP ( 'NONE', ( #13636, #31594, #9140, #29773 ) ) ;
#1951 = AXIS2_PLACEMENT_3D ( 'NONE', #27384, #1390, #37822 ) ;
#1952 = CARTESIAN_POINT ( 'NONE',  ( 2.500000000000000000, 1.768423874527823791, 1.020999999999998353 ) ) ;
#1953 = CARTESIAN_POINT ( 'NONE',  ( -36.94957890273524725, -12.05525454449572109, 165.5452302238048503 ) ) ;
#1954 = AXIS2_PLACEMENT_3D ( 'NONE', #23607, #40343, #27284 ) ;
#1955 = CARTESIAN_POINT ( 'NONE',  ( 17.99999999999999645, 67.32409792376505209, 89.75376489259387824 ) ) ;
#1956 = LINE ( 'NONE', #5865, #17884 ) ;
#1957 = VERTEX_POINT ( 'NONE', #34531 ) ;
#1958 = CARTESIAN_POINT ( 'NONE',  ( -15.99999999999997691, 31.00000000000000355, -2.499999999999994671 ) ) ;
#1959 = UNCERTAINTY_MEASURE_WITH_UNIT (LENGTH_MEASURE( 1.000000000000000082E-05 ), #24390, 'distance_accuracy_value', 'NONE');
#1960 = EDGE_CURVE ( 'NONE', #25462, #7155, #40191, .T. ) ;
#1961 = CARTESIAN_POINT ( 'NONE',  ( 17.99999999999999645, 34.74871106919619024, 106.6808302961373158 ) ) ;
#1962 = VERTEX_POINT ( 'NONE', #8353 ) ;
#1963 = CARTESIAN_POINT ( 'NONE',  ( 0.000000000000000000, 0.000000000000000000, 0.000000000000000000 ) ) ;
#1964 = ADVANCED_FACE ( 'NONE', ( #21508 ), #14717, .F. ) ;
#1965 = DIRECTION ( 'NONE',  ( 0.000000000000000000, 0.5076658003388409002, -0.8615540813938056264 ) ) ;
#1966 = CARTESIAN_POINT ( 'NONE',  ( -106.4195705685756081, 17.99999999999998934, -106.4195705685752529 ) ) ;
#1967 = DIRECTION ( 'NONE',  ( 0.000000000000000000, 0.8951632913550604531, 0.4457383557765420834 ) ) ;
#1968 = CARTESIAN_POINT ( 'NONE',  ( 26.72236725836960147, 31.00000000000000355, -46.28813965123160301 ) ) ;
#1969 = ORIENTED_EDGE ( 'NONE', *, *, #3743, .T. ) ;
#1971 = CARTESIAN_POINT ( 'NONE',  ( 17.99999999999999645, -27.24480646643597126, -15.80846360676612861 ) ) ;
#1970 = DIRECTION ( 'NONE',  ( -1.000000000000000000, -0.000000000000000000, -0.000000000000000000 ) ) ;
#1972 = AXIS2_PLACEMENT_3D ( 'NONE', #17498, #27288, #14422 ) ;
#1973 = VERTEX_POINT ( 'NONE', #28021 ) ;
#1974 = AXIS2_PLACEMENT_3D ( 'NONE', #16341, #358, #9340 ) ;
#1975 = CARTESIAN_POINT ( 'NONE',  ( 18.36587843422771016, 40.00000000000000000, 54.06640964556338957 ) ) ;
#1976 = EDGE_CURVE ( 'NONE', #39935, #35045, #2570, .T. ) ;
#1977 = CARTESIAN_POINT ( 'NONE',  ( -10.00000000000000000, 0.000000000000000000, 0.000000000000000000 ) ) ;
#1978 = DIRECTION ( 'NONE',  ( 1.000000000000000000, 0.000000000000000000, 0.000000000000000000 ) ) ;
#1979 = EDGE_CURVE ( 'NONE', #33515, #30585, #22847, .T. ) ;
#1980 = DIRECTION ( 'NONE',  ( 1.000000000000000000, 0.000000000000000000, 0.000000000000000000 ) ) ;
#1981 = CARTESIAN_POINT ( 'NONE',  ( 17.96659372829068246, 31.00000000000000355, -15.76829228678407624 ) ) ;
#1982 = ORIENTED_EDGE ( 'NONE', *, *, #20784, .F. ) ;
#1983 = CARTESIAN_POINT ( 'NONE',  ( -4.929261580875707871, 40.00000000000000000, 37.46659216873931797 ) ) ;
#1984 = ORIENTED_EDGE ( 'NONE', *, *, #344, .T. ) ;
#1985 = CARTESIAN_POINT ( 'NONE',  ( 17.99999999999999645, 0.000000000000000000, 0.000000000000000000 ) ) ;
#1986 = FACE_OUTER_BOUND ( 'NONE', #6911, .T. ) ;
#1987 = ORIENTED_EDGE ( 'NONE', *, *, #38485, .T. ) ;
#1988 = DIRECTION ( 'NONE',  ( 1.000000000000000000, 0.000000000000000000, 0.000000000000000000 ) ) ;
#1989 = ORIENTED_EDGE ( 'NONE', *, *, #42017, .T. ) ;
#1990 = CARTESIAN_POINT ( 'NONE',  ( 18.00000000000000355, 38.92705108641770551, -27.21837053747755419 ) ) ;
#1991 = ORIENTED_EDGE ( 'NONE', *, *, #26679, .F. ) ;
#1992 = ADVANCED_FACE ( 'NONE', ( #41280 ), #37589, .F. ) ;
#1993 = VERTEX_POINT ( 'NONE', #31925 ) ;
#1994 = CARTESIAN_POINT ( 'NONE',  ( 17.99999999999999645, 108.8880088604282008, -39.99251838045848473 ) ) ;
#1995 = CARTESIAN_POINT ( 'NONE',  ( -5.410573124821301150, 31.00000000000000355, -84.40011308935179102 ) ) ;
#1996 = ORIENTED_EDGE ( 'NONE', *, *, #34716, .F. ) ;
#1997 = DIRECTION ( 'NONE',  ( -1.000000000000000000, 0.000000000000000000, 0.000000000000000000 ) ) ;
#1998 = AXIS2_PLACEMENT_3D ( 'NONE', #12015, #32851, #21645 ) ;
#1999 = AXIS2_PLACEMENT_3D ( 'NONE', #2718, #33289, #29180 ) ;
#2000 = CARTESIAN_POINT ( 'NONE',  ( 0.000000000000000000, 0.000000000000000000, -4.974599999999998801 ) ) ;
#2001 = AXIS2_PLACEMENT_3D ( 'NONE', #29527, #25426, #41960 ) ;
#2002 = ORIENTED_EDGE ( 'NONE', *, *, #29349, .T. ) ;
#2003 = DIRECTION ( 'NONE',  ( 0.000000000000000000, -0.8951632913550663373, 0.4457383557765300930 ) ) ;
#2004 = EDGE_CURVE ( 'NONE', #41484, #24680, #21070, .T. ) ;
#2005 = CARTESIAN_POINT ( 'NONE',  ( -80.34276469473088866, 40.00000000000000711, 61.48650092628135866 ) ) ;
#2006 = CARTESIAN_POINT ( 'NONE',  ( 26.10672890669568602, 31.00000000000000355, 8.893381768403882504 ) ) ;
#2007 = ADVANCED_FACE ( 'NONE', ( #34968, #2009 ), #24763, .F. ) ;
#2009 = FACE_OUTER_BOUND ( 'NONE', #34245, .T. ) ;
#2008 = DIRECTION ( 'NONE',  ( -1.000000000000000000, -0.000000000000000000, -0.000000000000000000 ) ) ;
#2010 = CARTESIAN_POINT ( 'NONE',  ( 17.99999999999999645, -103.4151313792875158, 61.85306461934377609 ) ) ;
#2011 = DIRECTION ( 'NONE',  ( -1.000000000000000000, -0.000000000000000000, -0.000000000000000000 ) ) ;
#2012 = VERTEX_POINT ( 'NONE', #34317 ) ;
#2013 = VERTEX_POINT ( 'NONE', #26233 ) ;
#2014 = CARTESIAN_POINT ( 'NONE',  ( 17.99999999999999645, 115.9387338813861419, 3.769613505536437259 ) ) ;
#2015 = LINE ( 'NONE', #28029, #1123 ) ;
#2016 = CARTESIAN_POINT ( 'NONE',  ( 17.99999999999999645, -114.1529630473446986, -38.59523323561551678 ) ) ;
#2017 = ORIENTED_EDGE ( 'NONE', *, *, #39289, .T. ) ;
#2018 = CARTESIAN_POINT ( 'NONE',  ( 4.274771203358150196, 40.00000000000000000, -32.49882260841580006 ) ) ;
#2019 = CARTESIAN_POINT ( 'NONE',  ( -30.82418422902937039, 40.00000000000000000, 26.94311707097686792 ) ) ;
#2020 = VERTEX_POINT ( 'NONE', #22991 ) ;
#2021 = EDGE_CURVE ( 'NONE', #31789, #27337, #36232, .T. ) ;
#2022 = ORIENTED_EDGE ( 'NONE', *, *, #26835, .F. ) ;
#2023 = CARTESIAN_POINT ( 'NONE',  ( 0.000000000000000000, 0.000000000000000000, 0.000000000000000000 ) ) ;
#2024 = DIRECTION ( 'NONE',  ( 0.000000000000000000, -0.9957341762950354669, 0.09226835946329131621 ) ) ;
#2026 = ADVANCED_FACE ( 'NONE', ( #29500 ), #2211, .F. ) ;
#2025 = AXIS2_PLACEMENT_3D ( 'NONE', #33005, #28704, #15604 ) ;
#2027 = DIRECTION ( 'NONE',  ( 1.000000000000000000, 1.836909530733573776E-16, 0.000000000000000000 ) ) ;
#2028 = AXIS2_PLACEMENT_3D ( 'NONE', #36456, #40160, #7 ) ;
#2029 = EDGE_CURVE ( 'NONE', #416, #27001, #9206, .T. ) ;
#2030 = EDGE_CURVE ( 'NONE', #18, #17680, #8814, .T. ) ;
#2031 = CARTESIAN_POINT ( 'NONE',  ( 56.25020680251638083, -2.055254544495725977, 2.972870684497274762 ) ) ;
#2032 = CIRCLE ( 'NONE', #32689, 0.08401999999999888724 ) ;
#2033 = CARTESIAN_POINT ( 'NONE',  ( 0.000000000000000000, -67.32409792376564894, 89.75376489259340929 ) ) ;
#2034 = VERTEX_POINT ( 'NONE', #29293 ) ;
#2035 = DIRECTION ( 'NONE',  ( 1.000000000000000000, 0.000000000000000000, 0.000000000000000000 ) ) ;
#2036 = EDGE_LOOP ( 'NONE', ( #23878, #10776, #20193, #33755 ) ) ;
#2037 = DIRECTION ( 'NONE',  ( 0.000000000000000000, 1.541976423090494253E-15, 1.000000000000000000 ) ) ;
#2038 = DIRECTION ( 'NONE',  ( 0.000000000000000000, 0.000000000000000000, 1.000000000000000000 ) ) ;
#2039 = CARTESIAN_POINT ( 'NONE',  ( 18.00000000000000355, 43.83938735307268075, 18.28286404005813637 ) ) ;
#2040 = PLANE ( 'NONE',  #10116 ) ;
#2041 = VERTEX_POINT ( 'NONE', #16419 ) ;
#2042 = ORIENTED_EDGE ( 'NONE', *, *, #2004, .T. ) ;
#2043 = CARTESIAN_POINT ( 'NONE',  ( 18.00000000000000355, 15.49408907645172206, 44.90087086784598824 ) ) ;
#2044 = VERTEX_POINT ( 'NONE', #39279 ) ;
#2046 = ORIENTED_EDGE ( 'NONE', *, *, #35248, .T. ) ;
#2045 = DIRECTION ( 'NONE',  ( 3.996523416598993920E-16, 2.658563593772947074E-15, 1.000000000000000000 ) ) ;
#2047 = CARTESIAN_POINT ( 'NONE',  ( 46.08863070263671347, 31.00000000000000355, 35.47900410130831972 ) ) ;
#2048 = ORIENTED_EDGE ( 'NONE', *, *, #20310, .T. ) ;
#2049 = CARTESIAN_POINT ( 'NONE',  ( 0.000000000000000000, 68.61497464550733127, -99.05794392877533028 ) ) ;
#2050 = DIRECTION ( 'NONE',  ( -1.000000000000000000, 0.000000000000000000, 0.000000000000000000 ) ) ;
#2051 = ADVANCED_FACE ( 'NONE', ( #19277 ), #2637, .T. ) ;
#2052 = VERTEX_POINT ( 'NONE', #29086 ) ;
#2053 = CARTESIAN_POINT ( 'NONE',  ( -19.10382689932985656, 40.00000000000000000, -71.73905014343321795 ) ) ;
#2054 = AXIS2_PLACEMENT_3D ( 'NONE', #22164, #9018, #1823 ) ;
#2055 = AXIS2_PLACEMENT_3D ( 'NONE', #25182, #17558, #31268 ) ;
#2056 = CARTESIAN_POINT ( 'NONE',  ( 17.99999999999999645, -61.59243992711397198, -93.77976230226100540 ) ) ;
#2057 = EDGE_CURVE ( 'NONE', #25205, #20992, #33192, .T. ) ;
#2058 = CARTESIAN_POINT ( 'NONE',  ( 18.00000000000000355, -0.2227391519113303131, -46.98410307550732057 ) ) ;
#2059 = ORIENTED_EDGE ( 'NONE', *, *, #29299, .F. ) ;
#2060 = FACE_OUTER_BOUND ( 'NONE', #15986, .T. ) ;
#2061 = ORIENTED_EDGE ( 'NONE', *, *, #36953, .F. ) ;
#2062 = SURFACE_STYLE_FILL_AREA ( #12134 ) ;
#2063 = FACE_OUTER_BOUND ( 'NONE', #34647, .T. ) ;
#2064 = CARTESIAN_POINT ( 'NONE',  ( -8.920000000000003482, 0.000000000000000000, 14.91999999999999815 ) ) ;
#2065 = CARTESIAN_POINT ( 'NONE',  ( 16.30650823456882748, 31.00000000000000355, -60.90571087954511142 ) ) ;
#2066 = CARTESIAN_POINT ( 'NONE',  ( 17.99999999999999645, 0.000000000000000000, 0.000000000000000000 ) ) ;
#2067 = EDGE_LOOP ( 'NONE', ( #24561, #31518, #15195, #20919 ) ) ;
#2068 = SURFACE_STYLE_USAGE ( .BOTH. , #26308 ) ;
#2069 = ORIENTED_EDGE ( 'NONE', *, *, #42044, .F. ) ;
#2070 = LINE ( 'NONE', #24836, #5448 ) ;
#2071 = CARTESIAN_POINT ( 'NONE',  ( 17.99999999999999645, -107.2885202478262698, -54.86040852957422942 ) ) ;
#2072 = EDGE_CURVE ( 'NONE', #14692, #36478, #10913, .T. ) ;
#2073 = CARTESIAN_POINT ( 'NONE',  ( -37.02054590706428172, 31.00000000000000355, -75.34311506435014394 ) ) ;
#2074 = CARTESIAN_POINT ( 'NONE',  ( -40.08783408682389648, 40.00000000000000000, 81.04563091341927361 ) ) ;
#2075 = EDGE_CURVE ( 'NONE', #17062, #41964, #18621, .T. ) ;
#2076 = EDGE_CURVE ( 'NONE', #6200, #40762, #29720, .T. ) ;
#2077 = DIRECTION ( 'NONE',  ( -1.000000000000000000, 0.000000000000000000, 0.000000000000000000 ) ) ;
#2078 = EDGE_CURVE ( 'NONE', #9725, #29305, #22099, .T. ) ;
#2079 = ORIENTED_EDGE ( 'NONE', *, *, #3317, .T. ) ;
#2080 = CARTESIAN_POINT ( 'NONE',  ( -10.00000000000000000, 0.000000000000000000, 0.000000000000000000 ) ) ;
#2081 = ORIENTED_EDGE ( 'NONE', *, *, #1382, .F. ) ;
#2082 = CARTESIAN_POINT ( 'NONE',  ( 0.000000000000000000, -103.5682682299985515, -43.14958040911633219 ) ) ;
#2083 = VECTOR ( 'NONE', #34828, 1000.000000000000000 ) ;
#2084 = CIRCLE ( 'NONE', #27888, 2.649999999999999467 ) ;
#2086 = EDGE_LOOP ( 'NONE', ( #5203, #36771, #19499, #3248 ) ) ;
#2085 = DIRECTION ( 'NONE',  ( -1.000000000000000000, -1.836909530733573776E-16, 0.000000000000000000 ) ) ;
#2087 = VECTOR ( 'NONE', #14850, 1000.000000000000000 ) ;
#2088 = CARTESIAN_POINT ( 'NONE',  ( 17.99999999999999645, 26.29521155129848964, 17.34211205339357065 ) ) ;
#2089 = ORIENTED_EDGE ( 'NONE', *, *, #42452, .T. ) ;
#2090 = DIRECTION ( 'NONE',  ( 0.000000000000000000, -1.599473849036242511E-14, -1.000000000000000000 ) ) ;
#2091 = CARTESIAN_POINT ( 'NONE',  ( -9.000000000000005329, 0.000000000000000000, -12.59999999999999964 ) ) ;
#2092 = DIRECTION ( 'NONE',  ( -1.000000000000000000, -0.000000000000000000, -0.000000000000000000 ) ) ;
#2093 = EDGE_LOOP ( 'NONE', ( #14400, #9830, #23029, #24213 ) ) ;
#2094 = EDGE_CURVE ( 'NONE', #40855, #13726, #32552, .T. ) ;
#2095 = CARTESIAN_POINT ( 'NONE',  ( 27.02985023942251175, 31.00000000000000355, 3.586895573513789071 ) ) ;
#2096 = DIRECTION ( 'NONE',  ( 0.000000000000000000, 0.000000000000000000, 1.000000000000000000 ) ) ;
#2098 = CARTESIAN_POINT ( 'NONE',  ( 0.000000000000000000, -11.90021268425522827, -45.45261810511227907 ) ) ;
#2097 = DIRECTION ( 'NONE',  ( -1.000000000000000000, -0.000000000000000000, -0.000000000000000000 ) ) ;
#2099 = ORIENTED_EDGE ( 'NONE', *, *, #36276, .T. ) ;
#2100 = CARTESIAN_POINT ( 'NONE',  ( 0.000000000000000000, 0.000000000000000000, 0.000000000000000000 ) ) ;
#2101 = DIRECTION ( 'NONE',  ( -3.996523416598930318E-16, 2.658563593772947863E-15, 1.000000000000000000 ) ) ;
#2102 = CARTESIAN_POINT ( 'NONE',  ( -2.659806967433698599, 40.00000000000000000, 39.59793253468611596 ) ) ;
#2103 = CARTESIAN_POINT ( 'NONE',  ( 0.000000000000000000, -109.3506818544107659, -38.70953859161124910 ) ) ;
#2104 = CIRCLE ( 'NONE', #11204, 120.5010000000000474 ) ;
#2105 = EDGE_CURVE ( 'NONE', #18385, #10543, #20686, .T. ) ;
#2106 = DIRECTION ( 'NONE',  ( 0.000000000000000000, 0.000000000000000000, 1.000000000000000000 ) ) ;
#2107 = ADVANCED_FACE ( 'NONE', ( #18868, #2842 ), #3047, .T. ) ;
#2108 = DIRECTION ( 'NONE',  ( -1.000000000000000000, -0.000000000000000000, -0.000000000000000000 ) ) ;
#2109 = CIRCLE ( 'NONE', #4192, 59.00000000000000711 ) ;
#2110 = EDGE_LOOP ( 'NONE', ( #9573, #14181, #41848, #41209 ) ) ;
#2111 = CYLINDRICAL_SURFACE ( 'NONE', #38367, 59.00000000000000000 ) ;
#2112 = ORIENTED_EDGE ( 'NONE', *, *, #23938, .F. ) ;
#2113 = VECTOR ( 'NONE', #29831, 1000.000000000000000 ) ;
#2114 = DIRECTION ( 'NONE',  ( 0.000000000000000000, -0.9826841245925227453, 0.1852887240871045060 ) ) ;
#2115 = CARTESIAN_POINT ( 'NONE',  ( 9.000000000000001776, 63.55543939553896848, -97.03971415477259654 ) ) ;
#2116 = AXIS2_PLACEMENT_3D ( 'NONE', #27626, #8601, #35009 ) ;
#2118 = CARTESIAN_POINT ( 'NONE',  ( 34.98270738856093232, 31.00000000000000355, 4.602016392115340970 ) ) ;
#2117 = AXIS2_PLACEMENT_3D ( 'NONE', #13517, #40309, #26601 ) ;
#2119 = ORIENTED_EDGE ( 'NONE', *, *, #17419, .F. ) ;
#2120 = CARTESIAN_POINT ( 'NONE',  ( 18.00000000000000355, 0.000000000000000000, 0.000000000000000000 ) ) ;
#2121 = ORIENTED_EDGE ( 'NONE', *, *, #21743, .F. ) ;
#2122 = AXIS2_PLACEMENT_3D ( 'NONE', #11957, #8440, #18526 ) ;
#2123 = CARTESIAN_POINT ( 'NONE',  ( 4.000000000000000000, -1.560351142792952617, -0.2242961665059816367 ) ) ;
#2124 = CARTESIAN_POINT ( 'NONE',  ( -45.94448050778635917, 31.00000000000000355, -79.54744219826071117 ) ) ;
#2125 = ORIENTED_EDGE ( 'NONE', *, *, #9438, .F. ) ;
#2126 = CARTESIAN_POINT ( 'NONE',  ( 25.95756378415329024, 31.00000000000000355, 52.86556711865710412 ) ) ;
#2127 = ADVANCED_FACE ( 'NONE', ( #32128 ), #39080, .F. ) ;
#2128 = CARTESIAN_POINT ( 'NONE',  ( -84.90650804512098659, 40.00000000000000711, 28.83788733109305014 ) ) ;
#2129 = EDGE_LOOP ( 'NONE', ( #17727, #37551, #22985, #23177 ) ) ;
#2130 = DIRECTION ( 'NONE',  ( -1.000000000000000000, 0.000000000000000000, 0.000000000000000000 ) ) ;
#2131 = VECTOR ( 'NONE', #10668, 1000.000000000000000 ) ;
#2132 = DIRECTION ( 'NONE',  ( 0.000000000000000000, 0.000000000000000000, 1.000000000000000000 ) ) ;
#2133 = DIRECTION ( 'NONE',  ( -1.000000000000000000, -0.000000000000000000, -0.000000000000000000 ) ) ;
#2135 = EDGE_LOOP ( 'NONE', ( #36274, #8758, #39515, #37056, #6586, #37781, #26710, #12953, #23832, #37803, #32282, #16023, #34985, #3847, #8009, #29186 ) ) ;
#2134 = DIRECTION ( 'NONE',  ( 1.000000000000000000, 0.000000000000000000, 0.000000000000000000 ) ) ;
#2136 = DIRECTION ( 'NONE',  ( 0.000000000000000000, 0.000000000000000000, 1.000000000000000000 ) ) ;
#2137 = CIRCLE ( 'NONE', #26549, 59.00000000000001421 ) ;
#2138 = DIRECTION ( 'NONE',  ( 3.996523416598930318E-16, -2.658563593772947863E-15, -1.000000000000000000 ) ) ;
#2139 = ADVANCED_FACE ( 'NONE', ( #19493 ), #32757, .F. ) ;
#2140 = ORIENTED_EDGE ( 'NONE', *, *, #4828, .T. ) ;
#2141 = CARTESIAN_POINT ( 'NONE',  ( 55.68207322487837274, 39.99999999999999289, -32.16283696846894458 ) ) ;
#2142 = CARTESIAN_POINT ( 'NONE',  ( 0.000000000000000000, 0.000000000000000000, 9.999999999999998224 ) ) ;
#2143 = AXIS2_PLACEMENT_3D ( 'NONE', #35011, #31325, #38705 ) ;
#2144 = AXIS2_PLACEMENT_3D ( 'NONE', #9889, #251, #10762 ) ;
#2145 = ORIENTED_EDGE ( 'NONE', *, *, #7382, .T. ) ;
#2146 = EDGE_CURVE ( 'NONE', #27084, #7972, #303, .T. ) ;
#2147 = CARTESIAN_POINT ( 'NONE',  ( 8.999999999999998224, 0.000000000000000000, 0.000000000000000000 ) ) ;
#2148 = AXIS2_PLACEMENT_3D ( 'NONE', #35048, #41148, #41810 ) ;
#2149 = EDGE_CURVE ( 'NONE', #15934, #34314, #5196, .T. ) ;
#2150 = CARTESIAN_POINT ( 'NONE',  ( 17.99999999999999645, 0.000000000000000000, 0.000000000000000000 ) ) ;
#2151 = VERTEX_POINT ( 'NONE', #41176 ) ;
#2152 = ORIENTED_EDGE ( 'NONE', *, *, #33282, .T. ) ;
#2153 = CARTESIAN_POINT ( 'NONE',  ( 17.99999999999999645, 34.45183346761150744, -10.44371441202619444 ) ) ;
#2154 = ORIENTED_EDGE ( 'NONE', *, *, #19399, .F. ) ;
#2155 = AXIS2_PLACEMENT_3D ( 'NONE', #11538, #8833, #41170 ) ;
#2156 = DIRECTION ( 'NONE',  ( 0.000000000000000000, -0.9618256431728159361, -0.2736629900720938813 ) ) ;
#2157 = LINE ( 'NONE', #15514, #10955 ) ;
#2158 = LINE ( 'NONE', #18600, #37229 ) ;
#2159 = TOROIDAL_SURFACE ( 'NONE', #17537, 15.08402000000000065, 0.08401999999999888724 ) ;
#2160 = CYLINDRICAL_SURFACE ( 'NONE', #40106, 20.00000000000000355 ) ;
#2161 = ORIENTED_EDGE ( 'NONE', *, *, #33722, .T. ) ;
#2162 = CARTESIAN_POINT ( 'NONE',  ( 17.99999999999999645, 0.000000000000000000, 0.000000000000000000 ) ) ;
#2163 = ORIENTED_EDGE ( 'NONE', *, *, #33430, .T. ) ;
#2164 = CARTESIAN_POINT ( 'NONE',  ( 17.99999999999999645, -34.03109950475805334, 115.5957406979048727 ) ) ;
#2165 = VERTEX_POINT ( 'NONE', #16658 ) ;
#2166 = CARTESIAN_POINT ( 'NONE',  ( 17.99999999999999645, -10.40101730206447961, 120.0512800434970728 ) ) ;
#2167 = CARTESIAN_POINT ( 'NONE',  ( 0.000000000000000000, 112.1427988504407551, 3.502162136923788083 ) ) ;
#2168 = CYLINDRICAL_SURFACE ( 'NONE', #33717, 59.00000000000000000 ) ;
#2169 = CARTESIAN_POINT ( 'NONE',  ( 43.96541952717798551, 31.00000000000000355, 11.76906328551413239 ) ) ;
#2170 = ORIENTED_EDGE ( 'NONE', *, *, #3727, .F. ) ;
#2171 = DIRECTION ( 'NONE',  ( -1.000000000000000000, 0.000000000000000000, 0.000000000000000000 ) ) ;
#2172 = AXIS2_PLACEMENT_3D ( 'NONE', #12279, #2402, #11860 ) ;
#2173 = ORIENTED_EDGE ( 'NONE', *, *, #36590, .T. ) ;
#2174 = EDGE_CURVE ( 'NONE', #34774, #41169, #4771, .T. ) ;
#2175 = CARTESIAN_POINT ( 'NONE',  ( 28.01378275134445772, 40.00000000000000000, -56.83506808085938644 ) ) ;
#2176 = ADVANCED_FACE ( 'NONE', ( #10499 ), #26873, .T. ) ;
#2177 = CIRCLE ( 'NONE', #34964, 31.49900000000000233 ) ;
#2178 = DIRECTION ( 'NONE',  ( -3.996523416598930318E-16, 2.658563593772947863E-15, 1.000000000000000000 ) ) ;
#2179 = CYLINDRICAL_SURFACE ( 'NONE', #25628, 120.5010000000000190 ) ;
#2180 = DIRECTION ( 'NONE',  ( 0.000000000000000000, 0.000000000000000000, 1.000000000000000000 ) ) ;
#2181 = CARTESIAN_POINT ( 'NONE',  ( -10.00000000000000000, 0.000000000000000000, 0.000000000000000000 ) ) ;
#2182 = EDGE_CURVE ( 'NONE', #16388, #11355, #29943, .T. ) ;
#2183 = ORIENTED_EDGE ( 'NONE', *, *, #4223, .F. ) ;
#2184 = CARTESIAN_POINT ( 'NONE',  ( 11.92156526682413720, 40.00000000000000000, 35.08788755311113761 ) ) ;
#2185 = VERTEX_POINT ( 'NONE', #37103 ) ;
#2186 = CARTESIAN_POINT ( 'NONE',  ( 17.99999999999999645, 0.000000000000000000, 0.000000000000000000 ) ) ;
#2187 = DIRECTION ( 'NONE',  ( -1.000000000000000000, -0.000000000000000000, 0.000000000000000000 ) ) ;
#2188 = ORIENTED_EDGE ( 'NONE', *, *, #16579, .T. ) ;
#2189 = ADVANCED_FACE ( 'NONE', ( #42996 ), #37911, .T. ) ;
#2190 = CARTESIAN_POINT ( 'NONE',  ( 104.9999999999993321, -2.506021480131494702E-13, -40.00000000000000000 ) ) ;
#2191 = EDGE_LOOP ( 'NONE', ( #8546, #16543, #35546, #24311 ) ) ;
#2192 = CARTESIAN_POINT ( 'NONE',  ( 0.000000000000000000, -110.3490479609630910, -20.28201389785511211 ) ) ;
#2193 = ORIENTED_EDGE ( 'NONE', *, *, #12425, .T. ) ;
#2194 = CIRCLE ( 'NONE', #35651, 13.59999999999999964 ) ;
#2195 = ORIENTED_EDGE ( 'NONE', *, *, #27318, .T. ) ;
#2196 = DIRECTION ( 'NONE',  ( -1.000000000000000000, 0.000000000000000000, 0.000000000000000000 ) ) ;
#2197 = CIRCLE ( 'NONE', #17587, 116.0000000000000000 ) ;
#2198 = CARTESIAN_POINT ( 'NONE',  ( 77.59064570035201314, 31.00000000000000000, -38.12735739514867817 ) ) ;
#2199 = EDGE_LOOP ( 'NONE', ( #19507, #33307, #37312, #33705 ) ) ;
#2200 = CYLINDRICAL_SURFACE ( 'NONE', #37712, 13.59999999999999964 ) ;
#2201 = AXIS2_PLACEMENT_3D ( 'NONE', #9390, #41760, #42972 ) ;
#2202 = DIRECTION ( 'NONE',  ( -1.000000000000000000, 0.000000000000000000, 0.000000000000000000 ) ) ;
#2203 = EDGE_LOOP ( 'NONE', ( #23105, #31689, #40551, #10405 ) ) ;
#2204 = DIRECTION ( 'NONE',  ( 0.000000000000000000, 0.000000000000000000, 1.000000000000000000 ) ) ;
#2205 = CARTESIAN_POINT ( 'NONE',  ( 17.99999999999999645, -30.01658535635190361, -108.1077105353201233 ) ) ;
#2206 = EDGE_CURVE ( 'NONE', #37256, #39541, #6562, .T. ) ;
#2207 = AXIS2_PLACEMENT_3D ( 'NONE', #20856, #34105, #23680 ) ;
#2208 = CARTESIAN_POINT ( 'NONE',  ( 14.33709021557830887, 31.00000000000000355, 24.89380824183666263 ) ) ;
#2209 = EDGE_CURVE ( 'NONE', #39386, #13089, #10105, .T. ) ;
#2211 = CYLINDRICAL_SURFACE ( 'NONE', #37364, 58.99999999999999289 ) ;
#2210 = CARTESIAN_POINT ( 'NONE',  ( 17.99999999999999645, -64.58410930313458209, -101.7319213743688664 ) ) ;
#2212 = DIRECTION ( 'NONE',  ( 1.000000000000000000, -0.000000000000000000, -0.000000000000000000 ) ) ;
#2213 = LINE ( 'NONE', #42135, #39522 ) ;
#2214 = ORIENTED_EDGE ( 'NONE', *, *, #39218, .T. ) ;
#2215 = APPLICATION_PROTOCOL_DEFINITION ( 'draft international standard', 'automotive_design', 1998, #3559 ) ;
#2216 = SURFACE_STYLE_USAGE ( .BOTH. , #5718 ) ;
#2217 = VERTEX_POINT ( 'NONE', #31181 ) ;
#2218 = CYLINDRICAL_SURFACE ( 'NONE', #26867, 20.00000000000000355 ) ;
#2219 = CARTESIAN_POINT ( 'NONE',  ( 17.99999999999999645, -19.69434969228090893, 24.58291258574042004 ) ) ;
#2220 = ORIENTED_EDGE ( 'NONE', *, *, #24907, .F. ) ;
#2221 = CARTESIAN_POINT ( 'NONE',  ( -26.76192867387533170, 40.00000000000000000, -15.44647709060871321 ) ) ;
#2222 = EDGE_CURVE ( 'NONE', #637, #10990, #3491, .T. ) ;
#2223 = CARTESIAN_POINT ( 'NONE',  ( 37.09854380388319584, 40.00000000000000000, 2.490183985263671129 ) ) ;
#2224 = VERTEX_POINT ( 'NONE', #40149 ) ;
#2225 = ORIENTED_EDGE ( 'NONE', *, *, #27472, .F. ) ;
#2226 = DIRECTION ( 'NONE',  ( 1.000000000000000000, 0.000000000000000000, 0.000000000000000000 ) ) ;
#2227 = CARTESIAN_POINT ( 'NONE',  ( 0.000000000000000000, 43.83938735307293655, -18.28286404005752530 ) ) ;
#2228 = CIRCLE ( 'NONE', #833, 14.91999999999999993 ) ;
#2229 = DIRECTION ( 'NONE',  ( -1.000000000000000000, -0.000000000000000000, -0.000000000000000000 ) ) ;
#2230 = ADVANCED_FACE ( 'NONE', ( #9844 ), #207, .T. ) ;
#2231 = LINE ( 'NONE', #29316, #4872 ) ;
#2232 = VERTEX_POINT ( 'NONE', #13366 ) ;
#2233 = DIRECTION ( 'NONE',  ( -1.000000000000000000, 0.000000000000000000, 0.000000000000000000 ) ) ;
#2234 = ORIENTED_EDGE ( 'NONE', *, *, #5925, .T. ) ;
#2235 = DIRECTION ( 'NONE',  ( 0.000000000000000000, 0.000000000000000000, 1.000000000000000000 ) ) ;
#2236 = VECTOR ( 'NONE', #25974, 1000.000000000000000 ) ;
#2237 = DIRECTION ( 'NONE',  ( 3.996523416598930318E-16, -2.658563593772947863E-15, -1.000000000000000000 ) ) ;
#2238 = EDGE_CURVE ( 'NONE', #24063, #30314, #12903, .T. ) ;
#2239 = CARTESIAN_POINT ( 'NONE',  ( 0.000000000000000000, -75.72520367775142347, 82.78868281115956052 ) ) ;
#2240 = CARTESIAN_POINT ( 'NONE',  ( 0.000000000000000000, -34.03046037009231384, -33.13733193845841640 ) ) ;
#2241 = ORIENTED_EDGE ( 'NONE', *, *, #27292, .T. ) ;
#2242 = EDGE_LOOP ( 'NONE', ( #42171, #17699, #25234, #24047 ) ) ;
#2243 = CARTESIAN_POINT ( 'NONE',  ( 17.99999999999999645, -24.70533337038242649, 26.18485254986684296 ) ) ;
#2244 = ORIENTED_EDGE ( 'NONE', *, *, #15325, .T. ) ;
#2246 = ORIENTED_EDGE ( 'NONE', *, *, #35440, .F. ) ;
#2245 = CARTESIAN_POINT ( 'NONE',  ( 17.99999999999999645, 16.86122981692056655, -27.13802899033274940 ) ) ;
#2247 = CARTESIAN_POINT ( 'NONE',  ( -45.80426865612386678, 31.00000000000000355, -26.55377233851146812 ) ) ;
#2248 = ORIENTED_EDGE ( 'NONE', *, *, #42790, .F. ) ;
#2249 = DIRECTION ( 'NONE',  ( -1.000000000000000000, 0.000000000000000000, 0.000000000000000000 ) ) ;
#2250 = DIRECTION ( 'NONE',  ( -1.000000000000000000, 0.000000000000000000, -0.000000000000000000 ) ) ;
#2251 = ORIENTED_EDGE ( 'NONE', *, *, #38807, .T. ) ;
#2252 = VECTOR ( 'NONE', #35073, 1000.000000000000000 ) ;
#2253 = CARTESIAN_POINT ( 'NONE',  ( 4.437437895627098783, 40.00000000000000000, 69.40004907513484511 ) ) ;
#2254 = EDGE_CURVE ( 'NONE', #4572, #1856, #41466, .T. ) ;
#2256 = DIRECTION ( 'NONE',  ( 1.000000000000000000, 0.000000000000000000, 0.000000000000000000 ) ) ;
#2255 = DIRECTION ( 'NONE',  ( 1.000000000000000000, 0.000000000000000000, 0.000000000000000000 ) ) ;
#2257 = EDGE_CURVE ( 'NONE', #35838, #26002, #34649, .T. ) ;
#2258 = AXIS2_PLACEMENT_3D ( 'NONE', #25084, #35267, #21377 ) ;
#2259 = DIRECTION ( 'NONE',  ( 0.000000000000000000, 0.000000000000000000, 1.000000000000000000 ) ) ;
#2260 = VERTEX_POINT ( 'NONE', #6790 ) ;
#2261 = FACE_OUTER_BOUND ( 'NONE', #9210, .T. ) ;
#2262 = VERTEX_POINT ( 'NONE', #20150 ) ;
#2263 =( NAMED_UNIT ( * ) PLANE_ANGLE_UNIT ( ) SI_UNIT ( $, .RADIAN. ) );
#2264 = AXIS2_PLACEMENT_3D ( 'NONE', #5191, #11780, #14393 ) ;
#2265 = DIRECTION ( 'NONE',  ( 0.000000000000000000, 0.6783118362696173298, -0.7347741508630660778 ) ) ;
#2266 = CARTESIAN_POINT ( 'NONE',  ( 0.000000000000000000, 17.33727698085324320, -110.8498592715971967 ) ) ;
#2267 = CARTESIAN_POINT ( 'NONE',  ( -47.15756294055117337, 31.00000000000000355, -53.75246728999482571 ) ) ;
#2269 = CARTESIAN_POINT ( 'NONE',  ( 17.99999999999999645, -115.6826031496112677, 8.575274253897077870 ) ) ;
#2268 = CARTESIAN_POINT ( 'NONE',  ( -10.00000000000000000, 0.000000000000000000, 0.000000000000000000 ) ) ;
#2270 = ORIENTED_EDGE ( 'NONE', *, *, #38290, .T. ) ;
#2271 = CARTESIAN_POINT ( 'NONE',  ( 17.99999999999999645, 0.000000000000000000, 0.000000000000000000 ) ) ;
#2272 = EDGE_CURVE ( 'NONE', #5078, #31476, #13578, .T. ) ;
#2273 = EDGE_LOOP ( 'NONE', ( #26089, #30626, #3550, #8568 ) ) ;
#2274 = DIRECTION ( 'NONE',  ( -1.000000000000000000, -0.000000000000000000, 0.000000000000000000 ) ) ;
#2275 = DIRECTION ( 'NONE',  ( 1.000000000000000000, 0.000000000000000000, 0.000000000000000000 ) ) ;
#2276 = CARTESIAN_POINT ( 'NONE',  ( 43.66223835209735427, 31.00000000000000355, 88.82794485014694885 ) ) ;
#2277 = CARTESIAN_POINT ( 'NONE',  ( 96.90013369365227902, 39.99999999999999289, -6.223598210838602540 ) ) ;
#2278 = CARTESIAN_POINT ( 'NONE',  ( 0.000000000000000000, 0.000000000000000000, 0.000000000000000000 ) ) ;
#2279 = ADVANCED_FACE ( 'NONE', ( #13805 ), #27101, .F. ) ;
#2280 = AXIS2_PLACEMENT_3D ( 'NONE', #16765, #36785, #29844 ) ;
#2281 = ORIENTED_EDGE ( 'NONE', *, *, #19704, .T. ) ;
#2282 = CARTESIAN_POINT ( 'NONE',  ( 17.99999999999999645, -62.45178862086154226, -93.20969140437570388 ) ) ;
#2283 = ORIENTED_EDGE ( 'NONE', *, *, #829, .T. ) ;
#2284 = CARTESIAN_POINT ( 'NONE',  ( 0.000000000000000000, 90.81729652456265001, -72.16798910853526650 ) ) ;
#2285 = EDGE_CURVE ( 'NONE', #27962, #5227, #28246, .T. ) ;
#2287 = VERTEX_POINT ( 'NONE', #27920 ) ;
#2286 = CARTESIAN_POINT ( 'NONE',  ( 17.99999999999999645, -63.55543939553828636, 97.03971415477303708 ) ) ;
#2288 = DIRECTION ( 'NONE',  ( -1.000000000000000000, -0.000000000000000000, -0.000000000000000000 ) ) ;
#2289 = ORIENTED_EDGE ( 'NONE', *, *, #37302, .F. ) ;
#2290 = CARTESIAN_POINT ( 'NONE',  ( 9.000000000000000000, -6.007673836297746206, -35.49518073030003507 ) ) ;
#2291 = CARTESIAN_POINT ( 'NONE',  ( 17.99999999999999645, 0.000000000000000000, 0.000000000000000000 ) ) ;
#2292 = DIRECTION ( 'NONE',  ( 1.000000000000000000, 1.836909530733573776E-16, 0.000000000000000000 ) ) ;
#2293 = AXIS2_PLACEMENT_3D ( 'NONE', #28778, #5414, #32036 ) ;
#2294 = ORIENTED_EDGE ( 'NONE', *, *, #39324, .F. ) ;
#2295 = CARTESIAN_POINT ( 'NONE',  ( -21.37212791037561388, 31.00000000000000355, -7.253704819187424491 ) ) ;
#2296 = CARTESIAN_POINT ( 'NONE',  ( 17.99999999999999645, 0.000000000000000000, 0.000000000000000000 ) ) ;
#2298 = ORIENTED_EDGE ( 'NONE', *, *, #2587, .F. ) ;
#2297 = CYLINDRICAL_SURFACE ( 'NONE', #36237, 20.00000000000000355 ) ;
#2299 = ORIENTED_EDGE ( 'NONE', *, *, #39507, .F. ) ;
#2300 = DIRECTION ( 'NONE',  ( 1.000000000000000000, 0.000000000000000000, -0.000000000000000000 ) ) ;
#2301 = CARTESIAN_POINT ( 'NONE',  ( 0.000000000000000000, 0.000000000000000000, 0.000000000000000000 ) ) ;
#2302 = CARTESIAN_POINT ( 'NONE',  ( -37.13421060599359436, 40.00000000000000000, -21.52932707635456211 ) ) ;
#2303 = CARTESIAN_POINT ( 'NONE',  ( -19.74979319748359430, -2.055254544495722868, 2.972870684497276539 ) ) ;
#2304 = ADVANCED_FACE ( 'NONE', ( #23196 ), #24887, .T. ) ;
#2305 = EDGE_CURVE ( 'NONE', #20768, #38293, #28984, .T. ) ;
#2306 = DIRECTION ( 'NONE',  ( -1.000000000000000000, -0.000000000000000000, -0.000000000000000000 ) ) ;
#2307 = ADVANCED_FACE ( 'NONE', ( #8466, #22254 ), #2316, .F. ) ;
#2308 = EDGE_CURVE ( 'NONE', #27480, #2459, #14313, .T. ) ;
#2309 = AXIS2_PLACEMENT_3D ( 'NONE', #22613, #32612, #16054 ) ;
#2310 = CARTESIAN_POINT ( 'NONE',  ( 18.00000000000000355, -17.50309955389580452, -43.60271849949383949 ) ) ;
#2311 = ORIENTED_EDGE ( 'NONE', *, *, #27025, .F. ) ;
#2312 = CARTESIAN_POINT ( 'NONE',  ( 18.00000000000000355, -35.11945359308136716, 38.34871548466002622 ) ) ;
#2313 = ORIENTED_EDGE ( 'NONE', *, *, #16329, .T. ) ;
#2314 = VECTOR ( 'NONE', #37076, 1000.000000000000000 ) ;
#2315 = CARTESIAN_POINT ( 'NONE',  ( 8.999999999999998224, -28.35267316522799419, 22.18391138608698299 ) ) ;
#2316 = PLANE ( 'NONE',  #3104 ) ;
#2317 = CARTESIAN_POINT ( 'NONE',  ( 2.454369252093185239, 31.00000000000000355, 37.39583333513270702 ) ) ;
#2318 = ORIENTED_EDGE ( 'NONE', *, *, #36953, .T. ) ;
#2319 =( NAMED_UNIT ( * ) PLANE_ANGLE_UNIT ( ) SI_UNIT ( $, .RADIAN. ) );
#2320 = ORIENTED_EDGE ( 'NONE', *, *, #7928, .T. ) ;
#2321 =( GEOMETRIC_REPRESENTATION_CONTEXT ( 3 ) GLOBAL_UNCERTAINTY_ASSIGNED_CONTEXT ( ( #2360 ) ) GLOBAL_UNIT_ASSIGNED_CONTEXT ( ( #25403, #39085, #28871 ) ) REPRESENTATION_CONTEXT ( 'NONE', 'WORKASPACE' ) );
#2322 = DIRECTION ( 'NONE',  ( 1.000000000000000000, -0.000000000000000000, 0.000000000000000000 ) ) ;
#2323 = CARTESIAN_POINT ( 'NONE',  ( -77.37786320076959612, 31.00000000000000711, 44.69160382239309115 ) ) ;
#2324 = AXIS2_PLACEMENT_3D ( 'NONE', #35656, #8845, #12566 ) ;
#2325 = DIRECTION ( 'NONE',  ( 0.000000000000000000, -0.3140767120219362107, -0.9493976084683853900 ) ) ;
#2326 = EDGE_LOOP ( 'NONE', ( #31321, #23179 ) ) ;
#2327 = CARTESIAN_POINT ( 'NONE',  ( 8.570044366903687205, 31.00000000000000355, -64.27561742005508449 ) ) ;
#2328 = DIRECTION ( 'NONE',  ( 0.000000000000000000, 0.000000000000000000, -1.000000000000000000 ) ) ;
#2329 = VECTOR ( 'NONE', #26273, 1000.000000000000000 ) ;
#2330 = ORIENTED_EDGE ( 'NONE', *, *, #12459, .F. ) ;
#2331 = CYLINDRICAL_SURFACE ( 'NONE', #34563, 59.00000000000000000 ) ;
#2332 = DIRECTION ( 'NONE',  ( -1.000000000000000000, -0.000000000000000000, -0.000000000000000000 ) ) ;
#2333 = CARTESIAN_POINT ( 'NONE',  ( 0.000000000000000000, -29.03409033315573851, -12.21509719675420946 ) ) ;
#2334 = AXIS2_PLACEMENT_3D ( 'NONE', #13533, #7608, #20969 ) ;
#2336 = ORIENTED_EDGE ( 'NONE', *, *, #26033, .T. ) ;
#2335 = DIRECTION ( 'NONE',  ( -1.000000000000000000, -0.000000000000000000, 0.000000000000000000 ) ) ;
#2337 = CARTESIAN_POINT ( 'NONE',  ( 17.99999999999999645, 23.21237537461889389, -109.7700237000589709 ) ) ;
#2338 = DIRECTION ( 'NONE',  ( -1.000000000000000000, -0.000000000000000000, -0.000000000000000000 ) ) ;
#2339 = AXIS2_PLACEMENT_3D ( 'NONE', #20489, #13498, #26583 ) ;
#2340 = ORIENTED_EDGE ( 'NONE', *, *, #9156, .T. ) ;
#2341 = CARTESIAN_POINT ( 'NONE',  ( 74.89583333416871369, 39.99999999999999289, -4.908738512848213276 ) ) ;
#2342 = DIRECTION ( 'NONE',  ( 0.000000000000000000, 0.000000000000000000, 1.000000000000000000 ) ) ;
#2343 = VERTEX_POINT ( 'NONE', #38770 ) ;
#2344 = DIRECTION ( 'NONE',  ( -1.000000000000000000, -0.000000000000000000, 0.000000000000000000 ) ) ;
#2345 = ORIENTED_EDGE ( 'NONE', *, *, #3883, .F. ) ;
#2346 =( NAMED_UNIT ( * ) PLANE_ANGLE_UNIT ( ) SI_UNIT ( $, .RADIAN. ) );
#2347 = AXIS2_PLACEMENT_3D ( 'NONE', #14230, #10722, #10960 ) ;
#2348 = ORIENTED_EDGE ( 'NONE', *, *, #14413, .F. ) ;
#2349 = CARTESIAN_POINT ( 'NONE',  ( -8.749793197483594298, -2.055254544495723756, 2.972870684497274762 ) ) ;
#2350 = VERTEX_POINT ( 'NONE', #11987 ) ;
#2351 = DIRECTION ( 'NONE',  ( 1.000000000000000000, 0.000000000000000000, 0.000000000000000000 ) ) ;
#2352 = LINE ( 'NONE', #32492, #24211 ) ;
#2353 = DIRECTION ( 'NONE',  ( -1.000000000000000000, -0.000000000000000000, -0.000000000000000000 ) ) ;
#2354 = EDGE_CURVE ( 'NONE', #3997, #39762, #19898, .T. ) ;
#2355 = ADVANCED_FACE ( 'NONE', ( #32235 ), #25304, .F. ) ;
#2356 = DIRECTION ( 'NONE',  ( -1.000000000000000000, 0.000000000000000000, 0.000000000000000000 ) ) ;
#2358 = ORIENTED_EDGE ( 'NONE', *, *, #10200, .F. ) ;
#2357 = VECTOR ( 'NONE', #29659, 1000.000000000000000 ) ;
#2359 = DIRECTION ( 'NONE',  ( -1.000000000000000000, 0.000000000000000000, 0.000000000000000000 ) ) ;
#2360 = UNCERTAINTY_MEASURE_WITH_UNIT (LENGTH_MEASURE( 1.000000000000000082E-05 ), #25403, 'distance_accuracy_value', 'NONE');
#2361 = ADVANCED_FACE ( 'NONE', ( #41393 ), #8900, .F. ) ;
#2362 = AXIS2_PLACEMENT_3D ( 'NONE', #40085, #9789, #35959 ) ;
#2363 = ORIENTED_EDGE ( 'NONE', *, *, #23969, .T. ) ;
#2364 = AXIS2_PLACEMENT_3D ( 'NONE', #36310, #38734, #6007 ) ;
#2365 = CARTESIAN_POINT ( 'NONE',  ( 23.00000000000001066, -1.165156337948621952E-13, -25.99999999999999289 ) ) ;
#2366 = ORIENTED_EDGE ( 'NONE', *, *, #33916, .F. ) ;
#2367 = DIRECTION ( 'NONE',  ( 0.000000000000000000, -1.000000000000000000, 5.297542245118643184E-16 ) ) ;
#2368 = AXIS2_PLACEMENT_3D ( 'NONE', #22260, #29856, #16319 ) ;
#2369 = DIRECTION ( 'NONE',  ( 0.000000000000000000, 0.000000000000000000, 1.000000000000000000 ) ) ;
#2370 = EDGE_CURVE ( 'NONE', #29797, #28903, #35701, .T. ) ;
#2372 = AXIS2_PLACEMENT_3D ( 'NONE', #18751, #25705, #32006 ) ;
#2371 = DIRECTION ( 'NONE',  ( 3.009274222672345096E-17, 1.000000000000000000, -2.455023325076454960E-18 ) ) ;
#2373 = CARTESIAN_POINT ( 'NONE',  ( 3.763366191185776088, 31.00000000000000355, 57.39583333449059666 ) ) ;
#2374 = ORIENTED_EDGE ( 'NONE', *, *, #16195, .F. ) ;
#2375 = DIRECTION ( 'NONE',  ( 0.000000000000000000, 0.000000000000000000, 1.000000000000000000 ) ) ;
#2376 = EDGE_CURVE ( 'NONE', #16211, #42312, #7336, .T. ) ;
#2377 = EDGE_LOOP ( 'NONE', ( #38231, #17944, #6084, #2912 ) ) ;
#2378 = CARTESIAN_POINT ( 'NONE',  ( -59.82155519081633344, 40.00000000000000711, -7.874468279900277423 ) ) ;
#2379 = CIRCLE ( 'NONE', #26804, 20.00000000000000711 ) ;
#2380 = CARTESIAN_POINT ( 'NONE',  ( 17.99999999999999645, 30.74337109795219547, -8.695908345466218492 ) ) ;
#2381 = FACE_OUTER_BOUND ( 'NONE', #41664, .T. ) ;
#2382 = FACE_OUTER_BOUND ( 'NONE', #35047, .T. ) ;
#2383 = EDGE_CURVE ( 'NONE', #27751, #5537, #31391, .T. ) ;
#2384 = CIRCLE ( 'NONE', #12196, 116.0000000000000000 ) ;
#2385 = CARTESIAN_POINT ( 'NONE',  ( 17.99999999999999645, -3.996885678773838713, 120.4346956066681713 ) ) ;
#2386 = AXIS2_PLACEMENT_3D ( 'NONE', #30735, #14166, #17017 ) ;
#2387 = ORIENTED_EDGE ( 'NONE', *, *, #25882, .T. ) ;
#2388 = CARTESIAN_POINT ( 'NONE',  ( 11.12085686420672381, 40.00000000000000000, -41.54537790535560760 ) ) ;
#2389 = CARTESIAN_POINT ( 'NONE',  ( 18.00000000000000355, 46.11014828289844303, -9.022736828080878624 ) ) ;
#2390 = DIRECTION ( 'NONE',  ( 0.000000000000000000, 0.1253332335643046747, -0.9921147013144777649 ) ) ;
#2391 = CIRCLE ( 'NONE', #35810, 120.5010000000000190 ) ;
#2392 = EDGE_LOOP ( 'NONE', ( #15895, #35412, #42434, #41583 ) ) ;
#2393 = DIRECTION ( 'NONE',  ( 0.000000000000000000, 0.000000000000000000, 1.000000000000000000 ) ) ;
#2394 = VERTEX_POINT ( 'NONE', #1693 ) ;
#2395 = DIRECTION ( 'NONE',  ( -1.000000000000000000, 0.000000000000000000, -0.000000000000000000 ) ) ;
#2396 = ORIENTED_EDGE ( 'NONE', *, *, #28334, .F. ) ;
#2397 = VECTOR ( 'NONE', #29588, 1000.000000000000000 ) ;
#2398 = ORIENTED_EDGE ( 'NONE', *, *, #14492, .T. ) ;
#2399 = DIRECTION ( 'NONE',  ( 0.000000000000000000, 0.000000000000000000, 1.000000000000000000 ) ) ;
#2400 = CARTESIAN_POINT ( 'NONE',  ( 76.16439905407254685, 31.00000000000000000, 44.11546174421767574 ) ) ;
#2401 = VERTEX_POINT ( 'NONE', #14827 ) ;
#2402 = DIRECTION ( 'NONE',  ( 0.000000000000000000, 0.000000000000000000, 1.000000000000000000 ) ) ;
#2403 = EDGE_CURVE ( 'NONE', #28151, #34294, #15047, .T. ) ;
#2404 = LINE ( 'NONE', #15771, #10100 ) ;
#2405 = VERTEX_POINT ( 'NONE', #8261 ) ;
#2407 = AXIS2_PLACEMENT_3D ( 'NONE', #8361, #21518, #15163 ) ;
#2406 = LINE ( 'NONE', #8773, #18968 ) ;
#2408 = PRODUCT_DEFINITION ( 'UNKNOWN', '', #17747, #5868 ) ;
#2409 = CARTESIAN_POINT ( 'NONE',  ( 43.66223835209735427, 40.00000000000000000, 88.82794485019093145 ) ) ;
#2410 = CYLINDRICAL_SURFACE ( 'NONE', #11679, 116.0000000000000000 ) ;
#2412 = DIRECTION ( 'NONE',  ( 0.000000000000000000, -0.5076658003388292428, -0.8615540813938123987 ) ) ;
#2411 = DIRECTION ( 'NONE',  ( 0.000000000000000000, 0.000000000000000000, 1.000000000000000000 ) ) ;
#2413 = EDGE_CURVE ( 'NONE', #6459, #6927, #34865, .T. ) ;
#2414 = CIRCLE ( 'NONE', #26838, 59.00000000000001421 ) ;
#2415 = CARTESIAN_POINT ( 'NONE',  ( 17.99999999999999645, 0.000000000000000000, 0.000000000000000000 ) ) ;
#2416 = VECTOR ( 'NONE', #25982, 1000.000000000000000 ) ;
#2417 = CARTESIAN_POINT ( 'NONE',  ( 9.000000000000001776, -41.60679253225837471, 108.2814610871944581 ) ) ;
#2418 = AXIS2_PLACEMENT_3D ( 'NONE', #9197, #9403, #38866 ) ;
#2419 = ORIENTED_EDGE ( 'NONE', *, *, #37837, .T. ) ;
#2420 = EDGE_CURVE ( 'NONE', #35898, #31916, #1910, .T. ) ;
#2421 = CARTESIAN_POINT ( 'NONE',  ( 33.47591237148697729, 31.00000000000000355, -8.973542178613062248 ) ) ;
#2422 = ORIENTED_EDGE ( 'NONE', *, *, #24709, .F. ) ;
#2423 = VECTOR ( 'NONE', #3623, 1000.000000000000000 ) ;
#2424 = DIRECTION ( 'NONE',  ( 0.000000000000000000, 0.000000000000000000, 1.000000000000000000 ) ) ;
#2425 = EDGE_CURVE ( 'NONE', #32233, #39191, #15048, .T. ) ;
#2426 = DIRECTION ( 'NONE',  ( -1.000000000000000000, 0.000000000000000000, 0.000000000000000000 ) ) ;
#2427 = VERTEX_POINT ( 'NONE', #8674 ) ;
#2428 = CIRCLE ( 'NONE', #20624, 11.00000000000023803 ) ;
#2429 = CARTESIAN_POINT ( 'NONE',  ( 24.63052733448982323, 40.00000000000000000, -3.251868155982907904 ) ) ;
#2430 = CARTESIAN_POINT ( 'NONE',  ( 36.95980244579788376, 40.00000000000000000, 4.931273285801174744 ) ) ;
#2431 = CIRCLE ( 'NONE', #14318, 59.00000000000000711 ) ;
#2432 = VERTEX_POINT ( 'NONE', #5411 ) ;
#2433 = ORIENTED_EDGE ( 'NONE', *, *, #41200, .T. ) ;
#2434 = PLANE ( 'NONE',  #33908 ) ;
#2435 = CARTESIAN_POINT ( 'NONE',  ( 0.000000000000000000, 24.70533337038260768, -26.18485254986667243 ) ) ;
#2436 = CARTESIAN_POINT ( 'NONE',  ( 0.000000000000000000, 0.7408941433508176022, -1.199999999999999956 ) ) ;
#2437 = CARTESIAN_POINT ( 'NONE',  ( -10.00000000000000000, 0.000000000000000000, 0.000000000000000000 ) ) ;
#2438 = CARTESIAN_POINT ( 'NONE',  ( 0.000000000000000000, 34.03109950475887047, -115.5957406979046596 ) ) ;
#2439 = DIRECTION ( 'NONE',  ( -1.000000000000000000, -0.000000000000000000, -0.000000000000000000 ) ) ;
#2440 = VERTEX_POINT ( 'NONE', #11777 ) ;
#2441 = CARTESIAN_POINT ( 'NONE',  ( -105.3367680159044966, 40.00000000000000000, 2.032994142711228136 ) ) ;
#2442 = ORIENTED_EDGE ( 'NONE', *, *, #12993, .F. ) ;
#2443 = CARTESIAN_POINT ( 'NONE',  ( 0.000000000000000000, -58.30069736313598128, -100.2847380560572930 ) ) ;
#2444 = EDGE_CURVE ( 'NONE', #5962, #11572, #18779, .T. ) ;
#2445 = CARTESIAN_POINT ( 'NONE',  ( -24.83242019125695421, 113.3108596183312216, 2.000000000000327738 ) ) ;
#2446 = EDGE_CURVE ( 'NONE', #10863, #6408, #42035, .T. ) ;
#2447 = CIRCLE ( 'NONE', #29651, 13.59999999999999964 ) ;
#2448 = CARTESIAN_POINT ( 'NONE',  ( 17.99999999999999645, 21.56073507908678977, -23.57770962728541875 ) ) ;
#2449 = DIRECTION ( 'NONE',  ( 0.000000000000000000, 0.9957341762950348008, -0.09226835946329869920 ) ) ;
#2450 = ORIENTED_EDGE ( 'NONE', *, *, #18500, .T. ) ;
#2451 = CARTESIAN_POINT ( 'NONE',  ( -90.10416666596678681, 40.00000000000000711, -5.890486217120279200 ) ) ;
#2452 = ORIENTED_EDGE ( 'NONE', *, *, #8968, .F. ) ;
#2453 = CIRCLE ( 'NONE', #15744, 120.5010000000000190 ) ;
#2454 = FACE_OUTER_BOUND ( 'NONE', #22799, .T. ) ;
#2455 = VECTOR ( 'NONE', #11395, 1000.000000000000000 ) ;
#2456 = ORIENTED_EDGE ( 'NONE', *, *, #10369, .F. ) ;
#2457 = AXIS2_PLACEMENT_3D ( 'NONE', #27437, #40709, #40935 ) ;
#2459 = VERTEX_POINT ( 'NONE', #29845 ) ;
#2458 = LINE ( 'NONE', #36273, #2724 ) ;
#2460 = CARTESIAN_POINT ( 'NONE',  ( -17.30549157494827384, 31.00000000000000355, -51.24895740946764988 ) ) ;
#2461 = AXIS2_PLACEMENT_3D ( 'NONE', #39829, #23101, #19398 ) ;
#2462 = ORIENTED_EDGE ( 'NONE', *, *, #11129, .T. ) ;
#2463 = CARTESIAN_POINT ( 'NONE',  ( 0.000000000000000000, 18.25486108452625089, 25.66996392254279868 ) ) ;
#2464 = AXIS2_PLACEMENT_3D ( 'NONE', #28481, #11026, #17805 ) ;
#2465 = EDGE_CURVE ( 'NONE', #28601, #37599, #42175, .T. ) ;
#2466 = DIRECTION ( 'NONE',  ( 0.000000000000000000, 0.000000000000000000, 1.000000000000000000 ) ) ;
#2467 = AXIS2_PLACEMENT_3D ( 'NONE', #19428, #19850, #29227 ) ;
#2468 = ORIENTED_EDGE ( 'NONE', *, *, #17099, .F. ) ;
#2469 = CARTESIAN_POINT ( 'NONE',  ( 67.48878131082858545, 39.99999999999999289, 39.09986611101696496 ) ) ;
#2471 = CARTESIAN_POINT ( 'NONE',  ( 1.411581201560190495E-15, 4.862606272033091592, -3.745885042887436622 ) ) ;
#2470 = CARTESIAN_POINT ( 'NONE',  ( 0.000000000000000000, 0.000000000000000000, 0.000000000000000000 ) ) ;
#2472 = CARTESIAN_POINT ( 'NONE',  ( 12.50000000000000000, 0.000000000000000000, -25.00000000000000000 ) ) ;
#2473 = ORIENTED_EDGE ( 'NONE', *, *, #35565, .F. ) ;
#2474 = CARTESIAN_POINT ( 'NONE',  ( 0.000000000000000000, 0.000000000000000000, 0.000000000000000000 ) ) ;
#2475 = VERTEX_POINT ( 'NONE', #2950 ) ;
#2476 = ADVANCED_FACE ( 'NONE', ( #33309 ), #6256, .F. ) ;
#2477 =( REPRESENTATION_RELATIONSHIP ('NONE','NONE', #330, #16840 ) REPRESENTATION_RELATIONSHIP_WITH_TRANSFORMATION ( #27263 )SHAPE_REPRESENTATION_RELATIONSHIP( ) );
#2478 = DIRECTION ( 'NONE',  ( -3.996523416598930318E-16, 2.658563593772947863E-15, 1.000000000000000000 ) ) ;
#2479 = DIRECTION ( 'NONE',  ( -1.000000000000000000, -0.000000000000000000, 0.000000000000000000 ) ) ;
#2480 = CARTESIAN_POINT ( 'NONE',  ( 57.76613438074698337, 31.00000000000000000, -28.48799604501563110 ) ) ;
#2482 = CARTESIAN_POINT ( 'NONE',  ( 17.99999999999999645, 58.30069736313667050, 100.2847380560568951 ) ) ;
#2481 = CARTESIAN_POINT ( 'NONE',  ( 18.00000000000000355, -36.34385289850609979, 29.77717097092063270 ) ) ;
#2483 = AXIS2_PLACEMENT_3D ( 'NONE', #16919, #30201, #24108 ) ;
#2484 = ORIENTED_EDGE ( 'NONE', *, *, #36161, .F. ) ;
#2485 = CIRCLE ( 'NONE', #31081, 59.00000000000000000 ) ;
#2486 = CIRCLE ( 'NONE', #34555, 13.60000000000000142 ) ;
#2487 = CARTESIAN_POINT ( 'NONE',  ( -6.600000000000001421, 3.469446951953649688E-15, 0.000000000000000000 ) ) ;
#2488 = AXIS2_PLACEMENT_3D ( 'NONE', #1385, #25416, #38035 ) ;
#2489 = ORIENTED_EDGE ( 'NONE', *, *, #34849, .T. ) ;
#2491 = VECTOR ( 'NONE', #15224, 1000.000000000000000 ) ;
#2490 = DIRECTION ( 'NONE',  ( 0.000000000000000000, 0.000000000000000000, -1.000000000000000000 ) ) ;
#2492 = CARTESIAN_POINT ( 'NONE',  ( 18.00000000000000355, -18.53613841426756537, -48.58406706613921955 ) ) ;
#2493 = CARTESIAN_POINT ( 'NONE',  ( 92.49871336439160530, 31.00000000000000000, 31.53380891771210415 ) ) ;
#2494 = CARTESIAN_POINT ( 'NONE',  ( 59.96221986557397088, 40.00000000000000000, 78.35452998770438171 ) ) ;
#2495 = AXIS2_PLACEMENT_3D ( 'NONE', #29498, #2634, #9203 ) ;
#2496 = LINE ( 'NONE', #9066, #24736 ) ;
#2497 = AXIS2_PLACEMENT_3D ( 'NONE', #42016, #15457, #9517 ) ;
#2498 = ORIENTED_EDGE ( 'NONE', *, *, #30840, .T. ) ;
#2499 = CARTESIAN_POINT ( 'NONE',  ( -105.9879088449591933, 31.00000000000000355, -2.880719929157669945 ) ) ;
#2500 = ORIENTED_EDGE ( 'NONE', *, *, #39057, .T. ) ;
#2501 = EDGE_CURVE ( 'NONE', #21981, #21881, #35917, .T. ) ;
#2502 = DIRECTION ( 'NONE',  ( 0.000000000000000000, 0.7525707698561353576, 0.6585113790650422017 ) ) ;
#2503 = ADVANCED_FACE ( 'NONE', ( #12612 ), #26556, .F. ) ;
#2504 = DIRECTION ( 'NONE',  ( 1.836909530733573776E-16, -1.000000000000000000, 0.000000000000000000 ) ) ;
#2505 = CYLINDRICAL_SURFACE ( 'NONE', #3072, 2.649999999999999467 ) ;
#2506 = ORIENTED_EDGE ( 'NONE', *, *, #36381, .T. ) ;
#2507 = DIRECTION ( 'NONE',  ( 1.000000000000000000, -0.000000000000000000, 0.000000000000000000 ) ) ;
#2508 = CARTESIAN_POINT ( 'NONE',  ( 17.99999999999999645, -100.6739960869714139, -49.52796165323368172 ) ) ;
#2509 = CARTESIAN_POINT ( 'NONE',  ( 17.99999999999999645, -56.51398178981889941, 96.92493144647428949 ) ) ;
#2510 = ORIENTED_EDGE ( 'NONE', *, *, #37505, .F. ) ;
#2511 = CARTESIAN_POINT ( 'NONE',  ( 12.72035051019680729, 31.00000000000000355, 25.87482915247129611 ) ) ;
#2512 = DIRECTION ( 'NONE',  ( 0.000000000000000000, -0.7164567402983066380, -0.6976315211349933820 ) ) ;
#2513 = AXIS2_PLACEMENT_3D ( 'NONE', #9564, #2763, #35520 ) ;
#2514 = ADVANCED_FACE ( 'NONE', ( #36555 ), #40036, .F. ) ;
#2515 = AXIS2_PLACEMENT_3D ( 'NONE', #13950, #27245, #24216 ) ;
#2516 = VECTOR ( 'NONE', #22247, 1000.000000000000000 ) ;
#2517 = AXIS2_PLACEMENT_3D ( 'NONE', #4483, #1223, #25066 ) ;
#2518 = EDGE_CURVE ( 'NONE', #2965, #40561, #27577, .T. ) ;
#2520 = ORIENTED_EDGE ( 'NONE', *, *, #10182, .F. ) ;
#2519 = FACE_OUTER_BOUND ( 'NONE', #5497, .T. ) ;
#2521 = ORIENTED_EDGE ( 'NONE', *, *, #14490, .F. ) ;
#2522 = DIRECTION ( 'NONE',  ( -1.000000000000000000, 0.000000000000000000, 0.000000000000000000 ) ) ;
#2523 = DIRECTION ( 'NONE',  ( 0.000000000000000000, 0.9618256431728199329, -0.2736629900720799480 ) ) ;
#2524 = CARTESIAN_POINT ( 'NONE',  ( 14.57966847436756019, 40.00000000000000000, -42.69519604897453036 ) ) ;
#2525 = STYLED_ITEM ( 'NONE', ( #13382 ), #14024 ) ;
#2526 = DIRECTION ( 'NONE',  ( 0.000000000000000000, 0.000000000000000000, 1.000000000000000000 ) ) ;
#2527 = AXIS2_PLACEMENT_3D ( 'NONE', #31144, #349, #3621 ) ;
#2528 = CARTESIAN_POINT ( 'NONE',  ( 9.000000000000001776, 25.18647942089742031, 113.2326863338528824 ) ) ;
#2529 = DIRECTION ( 'NONE',  ( -1.000000000000000000, -0.000000000000000000, 0.000000000000000000 ) ) ;
#2530 = VERTEX_POINT ( 'NONE', #9543 ) ;
#2531 = CARTESIAN_POINT ( 'NONE',  ( 2.500000000000000000, 2.357898499370431722, -2.818925648462311528E-15 ) ) ;
#2533 = ORIENTED_EDGE ( 'NONE', *, *, #36863, .F. ) ;
#2532 = AXIS2_PLACEMENT_3D ( 'NONE', #18376, #11584, #18814 ) ;
#2534 = EDGE_CURVE ( 'NONE', #13079, #18333, #22034, .T. ) ;
#2535 = DIRECTION ( 'NONE',  ( 0.000000000000000000, 0.8747630845319623871, -0.4845508703326481537 ) ) ;
#2536 = FACE_OUTER_BOUND ( 'NONE', #7477, .T. ) ;
#2537 = AXIS2_PLACEMENT_3D ( 'NONE', #41329, #11482, #24817 ) ;
#2538 = ADVANCED_FACE ( 'NONE', ( #9312 ), #16766, .F. ) ;
#2539 = CARTESIAN_POINT ( 'NONE',  ( 24.02862666965263116, 31.00000000000000355, 27.38392887651082575 ) ) ;
#2540 = DIRECTION ( 'NONE',  ( 0.000000000000000000, -0.4132121857683668242, -0.9106347728549183396 ) ) ;
#2541 = ORIENTED_EDGE ( 'NONE', *, *, #32242, .T. ) ;
#2542 = VECTOR ( 'NONE', #36090, 1000.000000000000000 ) ;
#2543 = PRODUCT_DEFINITION_SHAPE ( 'NONE', 'NONE',  #15380 ) ;
#2544 = CARTESIAN_POINT ( 'NONE',  ( -24.74979319748359785, -2.055254544495722868, 2.972870684497277427 ) ) ;
#2545 = CARTESIAN_POINT ( 'NONE',  ( 52.74436945453300041, 31.00000000000000355, 68.73989242669851762 ) ) ;
#2546 = DIRECTION ( 'NONE',  ( 1.000000000000000000, 0.000000000000000000, 0.000000000000000000 ) ) ;
#2548 = ORIENTED_EDGE ( 'NONE', *, *, #27711, .F. ) ;
#2547 = AXIS2_PLACEMENT_3D ( 'NONE', #18749, #8435, #1007 ) ;
#2549 = CARTESIAN_POINT ( 'NONE',  ( -38.62815422673675414, 31.00000000000000355, -50.51519254952904703 ) ) ;
#2550 = CARTESIAN_POINT ( 'NONE',  ( -46.76215110880508519, 40.00000000000000000, 53.15211786533807725 ) ) ;
#2551 = CARTESIAN_POINT ( 'NONE',  ( 17.99999999999999645, -76.48293397876204835, -82.08917884620389316 ) ) ;
#2552 = CIRCLE ( 'NONE', #1159, 20.00000000000000711 ) ;
#2553 = ORIENTED_EDGE ( 'NONE', *, *, #2795, .T. ) ;
#2554 = CIRCLE ( 'NONE', #13041, 59.00000000000000711 ) ;
#2555 = ADVANCED_FACE ( 'NONE', ( #2743 ), #9953, .F. ) ;
#2556 = LINE ( 'NONE', #43131, #13851 ) ;
#2557 = DIRECTION ( 'NONE',  ( 1.000000000000000000, 0.000000000000000000, 0.000000000000000000 ) ) ;
#2558 = EDGE_CURVE ( 'NONE', #32077, #37206, #42892, .T. ) ;
#2559 = CIRCLE ( 'NONE', #26982, 52.00000000000000000 ) ;
#2560 = EDGE_CURVE ( 'NONE', #6569, #3149, #21658, .T. ) ;
#2561 = ADVANCED_FACE ( 'NONE', ( #6461 ), #19815, .T. ) ;
#2563 = EDGE_LOOP ( 'NONE', ( #37489, #5883, #11625, #20473 ) ) ;
#2562 = CYLINDRICAL_SURFACE ( 'NONE', #12309, 10.99999999999998934 ) ;
#2564 = CARTESIAN_POINT ( 'NONE',  ( 17.99999999999999645, 83.58328028049660929, 80.43528614701352808 ) ) ;
#2565 = DIRECTION ( 'NONE',  ( 0.000000000000000000, 0.000000000000000000, 1.000000000000000000 ) ) ;
#2566 = CIRCLE ( 'NONE', #40187, 120.5010000000000332 ) ;
#2567 = VERTEX_POINT ( 'NONE', #16107 ) ;
#2568 = CARTESIAN_POINT ( 'NONE',  ( 5.072363130230502115, 40.00000000000000000, 77.39583333421907696 ) ) ;
#2569 = DIRECTION ( 'NONE',  ( 1.000000000000000000, 0.000000000000000000, 0.000000000000000000 ) ) ;
#2570 = CIRCLE ( 'NONE', #24948, 116.0000000000000000 ) ;
#2571 = EDGE_LOOP ( 'NONE', ( #11773, #3935, #14039, #27082 ) ) ;
#2572 = FACE_OUTER_BOUND ( 'NONE', #34341, .T. ) ;
#2573 = LINE ( 'NONE', #23132, #39850 ) ;
#2574 = ORIENTED_EDGE ( 'NONE', *, *, #25288, .F. ) ;
#2575 = EDGE_LOOP ( 'NONE', ( #10483, #23882, #32202, #22823 ) ) ;
#2576 = CARTESIAN_POINT ( 'NONE',  ( -6.999999999999995559, -18.77999999999999048, 2.299886688798728717E-15 ) ) ;
#2577 = VERTEX_POINT ( 'NONE', #29407 ) ;
#2578 = CARTESIAN_POINT ( 'NONE',  ( 0.000000000000000000, -76.48293397876315680, 82.08917884620285577 ) ) ;
#2579 = FACE_OUTER_BOUND ( 'NONE', #11382, .T. ) ;
#2580 = DIRECTION ( 'NONE',  ( 1.000000000000000000, 0.000000000000000000, 0.000000000000000000 ) ) ;
#2581 = DIRECTION ( 'NONE',  ( -1.000000000000000000, -0.000000000000000000, 0.000000000000000000 ) ) ;
#2582 = VERTEX_POINT ( 'NONE', #3169 ) ;
#2583 = AXIS2_PLACEMENT_3D ( 'NONE', #14238, #27543, #34284 ) ;
#2584 = CARTESIAN_POINT ( 'NONE',  ( 0.000000000000000000, -150.5000000000000284, 6.999999999999998224 ) ) ;
#2585 = VECTOR ( 'NONE', #39909, 1000.000000000000000 ) ;
#2586 = VERTEX_POINT ( 'NONE', #26765 ) ;
#2587 = EDGE_CURVE ( 'NONE', #27036, #40970, #5967, .T. ) ;
#2588 = AXIS2_PLACEMENT_3D ( 'NONE', #33198, #16207, #6791 ) ;
#2589 = CIRCLE ( 'NONE', #3988, 31.49900000000000233 ) ;
#2590 = DIRECTION ( 'NONE',  ( 0.000000000000000000, 0.000000000000000000, 1.000000000000000000 ) ) ;
#2591 = EDGE_LOOP ( 'NONE', ( #15301, #13878, #36634, #3742 ) ) ;
#2592 = DIRECTION ( 'NONE',  ( -1.000000000000000000, -0.000000000000000000, -0.000000000000000000 ) ) ;
#2593 = AXIS2_PLACEMENT_3D ( 'NONE', #4389, #34942, #14474 ) ;
#2594 = CARTESIAN_POINT ( 'NONE',  ( -104.2750351721725650, 39.99999999999999289, -4.541977405098627685 ) ) ;
#2595 = APPLICATION_PROTOCOL_DEFINITION ( 'draft international standard', 'automotive_design', 1998, #3308 ) ;
#2596 = CARTESIAN_POINT ( 'NONE',  ( 9.000000000000001776, -52.88069566989523906, 103.2454939717367211 ) ) ;
#2597 = CARTESIAN_POINT ( 'NONE',  ( 8.201713468707295007, 31.00000000000000355, -62.30543997111072940 ) ) ;
#2598 = DIRECTION ( 'NONE',  ( 1.000000000000000000, 0.000000000000000000, 0.000000000000000000 ) ) ;
#2599 = ORIENTED_EDGE ( 'NONE', *, *, #41735, .T. ) ;
#2600 = CARTESIAN_POINT ( 'NONE',  ( -27.06829236441750552, 31.00000000000000355, 15.58100167312263018 ) ) ;
#2601 = CARTESIAN_POINT ( 'NONE',  ( -68.16583574478268304, 40.00000000000000711, -18.25112749842637427 ) ) ;
#2602 = DIRECTION ( 'NONE',  ( 0.000000000000000000, -0.3140767120219556952, 0.9493976084683790617 ) ) ;
#2603 = DIRECTION ( 'NONE',  ( -1.000000000000000000, -0.000000000000000000, 0.000000000000000000 ) ) ;
#2604 = AXIS2_PLACEMENT_3D ( 'NONE', #18901, #12109, #12325 ) ;
#2605 = ADVANCED_FACE ( 'NONE', ( #2536 ), #22894, .F. ) ;
#2606 = ADVANCED_FACE ( 'NONE', ( #23946 ), #40475, .F. ) ;
#2607 = CARTESIAN_POINT ( 'NONE',  ( -10.00000000000000000, 0.000000000000000000, 0.000000000000000000 ) ) ;
#2608 = DIRECTION ( 'NONE',  ( -1.000000000000000000, 0.000000000000000000, 0.000000000000000000 ) ) ;
#2609 = AXIS2_PLACEMENT_3D ( 'NONE', #37508, #17926, #14407 ) ;
#2610 = EDGE_CURVE ( 'NONE', #12969, #19737, #14345, .T. ) ;
#2611 = ORIENTED_EDGE ( 'NONE', *, *, #15356, .F. ) ;
#2612 = CARTESIAN_POINT ( 'NONE',  ( -12.41726970680908515, 40.00000000000000000, 46.38546114896210071 ) ) ;
#2613 = DIRECTION ( 'NONE',  ( 0.000000000000000000, 0.000000000000000000, 1.000000000000000000 ) ) ;
#2614 = CARTESIAN_POINT ( 'NONE',  ( 9.000000000000001776, 7.162210897275726573, 51.50439529848830489 ) ) ;
#2615 = AXIS2_PLACEMENT_3D ( 'NONE', #7940, #20878, #10365 ) ;
#2616 = ORIENTED_EDGE ( 'NONE', *, *, #32720, .T. ) ;
#2617 = LINE ( 'NONE', #29275, #23163 ) ;
#2618 = CIRCLE ( 'NONE', #40972, 116.0000000000000000 ) ;
#2619 = DIRECTION ( 'NONE',  ( 0.000000000000000000, -0.9048270524660145808, -0.4257792915650830956 ) ) ;
#2620 = ORIENTED_EDGE ( 'NONE', *, *, #30859, .F. ) ;
#2621 = CARTESIAN_POINT ( 'NONE',  ( -10.00000000000000000, 0.000000000000000000, 0.000000000000000000 ) ) ;
#2622 = VERTEX_POINT ( 'NONE', #24167 ) ;
#2623 = VERTEX_POINT ( 'NONE', #36786 ) ;
#2624 = DIRECTION ( 'NONE',  ( -1.000000000000000000, -0.000000000000000000, -0.000000000000000000 ) ) ;
#2625 = EDGE_CURVE ( 'NONE', #39096, #26320, #10610, .T. ) ;
#2626 = CARTESIAN_POINT ( 'NONE',  ( 56.68048384767583769, 31.00000000000000000, -64.44707192207098956 ) ) ;
#2627 = EDGE_LOOP ( 'NONE', ( #39846, #23283, #6339, #35435 ) ) ;
#2628 = DIRECTION ( 'NONE',  ( 1.000000000000000000, 0.000000000000000000, 0.000000000000000000 ) ) ;
#2629 =( NAMED_UNIT ( * ) PLANE_ANGLE_UNIT ( ) SI_UNIT ( $, .RADIAN. ) );
#2630 = CARTESIAN_POINT ( 'NONE',  ( 0.000000000000000000, -114.8812324315176312, 16.07179003769107339 ) ) ;
#2631 = ORIENTED_EDGE ( 'NONE', *, *, #21746, .T. ) ;
#2632 = DIRECTION ( 'NONE',  ( -0.9979848074931935153, 0.000000000000000000, -0.06345332152672163162 ) ) ;
#2633 = CARTESIAN_POINT ( 'NONE',  ( 12.87762912549411354, 40.00000000000000000, 98.66289914827740404 ) ) ;
#2634 = DIRECTION ( 'NONE',  ( -1.000000000000000000, 0.000000000000000000, 0.000000000000000000 ) ) ;
#2635 = VECTOR ( 'NONE', #15550, 1000.000000000000000 ) ;
#2637 = CYLINDRICAL_SURFACE ( 'NONE', #16500, 36.00000000000000000 ) ;
#2636 = CYLINDRICAL_SURFACE ( 'NONE', #18326, 158.4999999999992042 ) ;
#2638 = EDGE_CURVE ( 'NONE', #38278, #24835, #38702, .T. ) ;
#2639 = FACE_OUTER_BOUND ( 'NONE', #15345, .T. ) ;
#2640 = AXIS2_PLACEMENT_3D ( 'NONE', #29871, #16124, #40056 ) ;
#2641 = VERTEX_POINT ( 'NONE', #26992 ) ;
#2642 = CIRCLE ( 'NONE', #36076, 58.99999999999999289 ) ;
#2643 = CARTESIAN_POINT ( 'NONE',  ( -9.022452542771789652, 31.00000000000000355, 26.59230923919664491 ) ) ;
#2644 = AXIS2_PLACEMENT_3D ( 'NONE', #16680, #42385, #39105 ) ;
#2645 = ORIENTED_EDGE ( 'NONE', *, *, #16879, .F. ) ;
#2646 = DIRECTION ( 'NONE',  ( -1.000000000000000000, 0.000000000000000000, -0.000000000000000000 ) ) ;
#2647 = FACE_OUTER_BOUND ( 'NONE', #897, .T. ) ;
#2648 = VERTEX_POINT ( 'NONE', #30896 ) ;
#2649 = CARTESIAN_POINT ( 'NONE',  ( -2.454369252093152376, 40.00000000000000000, 37.60416666486730009 ) ) ;
#2650 = CARTESIAN_POINT ( 'NONE',  ( 31.41502175087570947, 40.00000000000000000, -18.07270130326806523 ) ) ;
#2651 = ORIENTED_EDGE ( 'NONE', *, *, #27048, .T. ) ;
#2652 = ORIENTED_EDGE ( 'NONE', *, *, #6192, .T. ) ;
#2653 = CARTESIAN_POINT ( 'NONE',  ( 0.000000000000000000, 0.000000000000000000, 0.000000000000000000 ) ) ;
#2654 = FACE_OUTER_BOUND ( 'NONE', #11047, .T. ) ;
#2655 = EDGE_CURVE ( 'NONE', #26427, #7766, #40912, .T. ) ;
#2656 = CARTESIAN_POINT ( 'NONE',  ( 17.99999999999999645, -29.36437154452078246, 116.8684075565134890 ) ) ;
#2657 = CARTESIAN_POINT ( 'NONE',  ( 2.600000000000000533, -12.75000000000000000, -1.199999999999999956 ) ) ;
#2658 = DIRECTION ( 'NONE',  ( -1.000000000000000000, -0.000000000000000000, -0.000000000000000000 ) ) ;
#2659 = ORIENTED_EDGE ( 'NONE', *, *, #25976, .F. ) ;
#2660 = CARTESIAN_POINT ( 'NONE',  ( -19.99999999999999645, 40.00000000000000000, 0.000000000000000000 ) ) ;
#2661 = ORIENTED_EDGE ( 'NONE', *, *, #8849, .T. ) ;
#2662 = DIRECTION ( 'NONE',  ( 0.000000000000000000, 0.000000000000000000, 1.000000000000000000 ) ) ;
#2663 = CARTESIAN_POINT ( 'NONE',  ( -10.00000000000000000, 0.000000000000000000, 0.000000000000000000 ) ) ;
#2664 = AXIS2_PLACEMENT_3D ( 'NONE', #30080, #22922, #32692 ) ;
#2665 = DIRECTION ( 'NONE',  ( 1.000000000000000000, -1.373900992973642263E-15, 0.000000000000000000 ) ) ;
#2666 = CARTESIAN_POINT ( 'NONE',  ( 0.000000000000000000, 98.39501399267960835, 53.91376164787712355 ) ) ;
#2667 = VERTEX_POINT ( 'NONE', #557 ) ;
#2668 = DIRECTION ( 'NONE',  ( -1.000000000000000000, 0.000000000000000000, 0.000000000000000000 ) ) ;
#2669 = ORIENTED_EDGE ( 'NONE', *, *, #12932, .T. ) ;
#2670 = LINE ( 'NONE', #6184, #2329 ) ;
#2671 = ADVANCED_FACE ( 'NONE', ( #16973 ), #30257, .T. ) ;
#2672 = ORIENTED_EDGE ( 'NONE', *, *, #42069, .T. ) ;
#2674 = ORIENTED_EDGE ( 'NONE', *, *, #26231, .F. ) ;
#2673 = CYLINDRICAL_SURFACE ( 'NONE', #25111, 19.99999999999989342 ) ;
#2675 = EDGE_CURVE ( 'NONE', #39824, #23529, #13912, .T. ) ;
#2676 = CARTESIAN_POINT ( 'NONE',  ( -42.11670055801651102, 31.00000000000000355, -32.42481051985740237 ) ) ;
#2677 = EDGE_LOOP ( 'NONE', ( #35857, #1584, #37806, #13347 ) ) ;
#2678 = CARTESIAN_POINT ( 'NONE',  ( 17.99999999999999645, -94.83915810436441518, 59.94836581341558457 ) ) ;
#2679 = ADVANCED_FACE ( 'NONE', ( #33725 ), #21125, .F. ) ;
#2680 = ORIENTED_EDGE ( 'NONE', *, *, #12143, .T. ) ;
#2681 = PLANE ( 'NONE',  #26554 ) ;
#2682 = ORIENTED_EDGE ( 'NONE', *, *, #23317, .T. ) ;
#2683 = CARTESIAN_POINT ( 'NONE',  ( 9.885896071376818028, 40.00000000000000000, -74.20985814143865866 ) ) ;
#2685 = CARTESIAN_POINT ( 'NONE',  ( 0.000000000000000000, -8.053585752062225822, 46.81126742072019908 ) ) ;
#2684 = CYLINDRICAL_SURFACE ( 'NONE', #5681, 20.00000000000000711 ) ;
#2686 = LINE ( 'NONE', #3338, #40792 ) ;
#2687 = ORIENTED_EDGE ( 'NONE', *, *, #23226, .F. ) ;
#2688 = DIRECTION ( 'NONE',  ( -1.000000000000000000, 0.000000000000000000, 0.000000000000000000 ) ) ;
#2689 = EDGE_LOOP ( 'NONE', ( #27212, #33679, #22248, #7737, #33947 ) ) ;
#2690 = SURFACE_SIDE_STYLE ('',( #2062 ) ) ;
#2691 = EDGE_CURVE ( 'NONE', #14749, #35045, #34529, .T. ) ;
#2692 = CYLINDRICAL_SURFACE ( 'NONE', #35754, 2.649999999999979039 ) ;
#2693 = CARTESIAN_POINT ( 'NONE',  ( 17.99999999999999645, 0.000000000000000000, 0.000000000000000000 ) ) ;
#2694 = CARTESIAN_POINT ( 'NONE',  ( -64.44063486737354651, 31.00000000000000711, -49.42892067282641477 ) ) ;
#2695 = AXIS2_PLACEMENT_3D ( 'NONE', #14541, #21548, #27844 ) ;
#2697 = CYLINDRICAL_SURFACE ( 'NONE', #34608, 20.00000000000000711 ) ;
#2696 = CARTESIAN_POINT ( 'NONE',  ( 17.99999999999999645, 47.58001226230686598, -110.7096808509478763 ) ) ;
#2698 = VERTEX_POINT ( 'NONE', #24393 ) ;
#2699 = AXIS2_PLACEMENT_3D ( 'NONE', #10312, #23223, #3953 ) ;
#2700 = CARTESIAN_POINT ( 'NONE',  ( 0.000000000000000000, 17.08890430202814059, -43.76671000081927332 ) ) ;
#2701 = ORIENTED_EDGE ( 'NONE', *, *, #26748, .F. ) ;
#2702 = CARTESIAN_POINT ( 'NONE',  ( 9.000000000000001776, 19.12429268481714217, 114.4126803693779948 ) ) ;
#2703 = LINE ( 'NONE', #11940, #28336 ) ;
#2704 = CARTESIAN_POINT ( 'NONE',  ( -46.83686391397709770, 31.00000000000000355, -81.34213072392142863 ) ) ;
#2705 = CARTESIAN_POINT ( 'NONE',  ( -91.59543978412355614, 40.00000000000000711, -12.18496625897608254 ) ) ;
#2706 = FACE_OUTER_BOUND ( 'NONE', #26574, .T. ) ;
#2707 = EDGE_CURVE ( 'NONE', #1738, #25968, #37641, .T. ) ;
#2708 = ORIENTED_EDGE ( 'NONE', *, *, #33060, .F. ) ;
#2709 = DIRECTION ( 'NONE',  ( -1.000000000000000000, 0.000000000000000000, 0.000000000000000000 ) ) ;
#2710 = VERTEX_POINT ( 'NONE', #34374 ) ;
#2711 = CARTESIAN_POINT ( 'NONE',  ( 17.99999999999999645, 8.827181066045881153, 120.1772519049559662 ) ) ;
#2712 = DIRECTION ( 'NONE',  ( 0.000000000000000000, 0.000000000000000000, 1.000000000000000000 ) ) ;
#2713 = DIRECTION ( 'NONE',  ( -0.000000000000000000, -0.000000000000000000, 1.000000000000000000 ) ) ;
#2714 = EDGE_LOOP ( 'NONE', ( #26003, #5036, #29046, #42550 ) ) ;
#2715 = DIRECTION ( 'NONE',  ( -1.000000000000000000, -0.000000000000000000, -0.000000000000000000 ) ) ;
#2716 = DIRECTION ( 'NONE',  ( 0.000000000000000000, -1.000000000000000000, 1.287488025362403787E-15 ) ) ;
#2717 = EDGE_CURVE ( 'NONE', #34186, #20139, #30371, .T. ) ;
#2718 = CARTESIAN_POINT ( 'NONE',  ( 8.919999999999999929, 0.000000000000000000, 11.08000000000000007 ) ) ;
#2719 = AXIS2_PLACEMENT_3D ( 'NONE', #20295, #30300, #20509 ) ;
#2721 = ORIENTED_EDGE ( 'NONE', *, *, #75, .T. ) ;
#2720 = DIRECTION ( 'NONE',  ( -1.000000000000000000, -0.000000000000000000, -0.000000000000000000 ) ) ;
#2722 = EDGE_CURVE ( 'NONE', #5323, #34842, #4473, .T. ) ;
#2723 = CARTESIAN_POINT ( 'NONE',  ( 17.99999999999999645, -22.66088087769164972, -21.87856208362581256 ) ) ;
#2724 = VECTOR ( 'NONE', #15407, 1000.000000000000000 ) ;
#2725 = CARTESIAN_POINT ( 'NONE',  ( 17.99999999999999645, -53.40478689619801145, 108.0204598100363711 ) ) ;
#2726 = AXIS2_PLACEMENT_3D ( 'NONE', #36677, #33628, #26456 ) ;
#2727 = EDGE_CURVE ( 'NONE', #2740, #5428, #13659, .T. ) ;
#2729 = ORIENTED_EDGE ( 'NONE', *, *, #39408, .T. ) ;
#2728 = CARTESIAN_POINT ( 'NONE',  ( -80.96080130434580724, -34.05525454449571043, 14.45886780445738395 ) ) ;
#2730 = ORIENTED_EDGE ( 'NONE', *, *, #30580, .F. ) ;
#2731 = CYLINDRICAL_SURFACE ( 'NONE', #26813, 12.49999999999993427 ) ;
#2732 = CYLINDRICAL_SURFACE ( 'NONE', #23156, 20.00000000000000355 ) ;
#2733 = CARTESIAN_POINT ( 'NONE',  ( 34.59698569361206211, 40.00000000000000000, -30.23997570423562209 ) ) ;
#2734 = CARTESIAN_POINT ( 'NONE',  ( 0.000000000000000000, -18.25486108452643208, 25.66996392254267079 ) ) ;
#2735 =( REPRESENTATION_RELATIONSHIP ('NONE','NONE', #330, #15194 ) REPRESENTATION_RELATIONSHIP_WITH_TRANSFORMATION ( #25978 )SHAPE_REPRESENTATION_RELATIONSHIP( ) );
#2736 = DIRECTION ( 'NONE',  ( -1.000000000000000000, 0.000000000000000000, 0.000000000000000000 ) ) ;
#2737 = CARTESIAN_POINT ( 'NONE',  ( 4.000000000000000000, -2.309401076758514915, -3.433295621305383349 ) ) ;
#2738 = VERTEX_POINT ( 'NONE', #7551 ) ;
#2739 = CARTESIAN_POINT ( 'NONE',  ( -0.3198814748697807464, -4.434118497892185040, -0.3507732604232532969 ) ) ;
#2740 = VERTEX_POINT ( 'NONE', #40265 ) ;
#2741 = EDGE_CURVE ( 'NONE', #2623, #4572, #34158, .T. ) ;
#2742 = DIRECTION ( 'NONE',  ( -1.000000000000000000, -0.000000000000000000, -0.000000000000000000 ) ) ;
#2743 = FACE_OUTER_BOUND ( 'NONE', #9885, .T. ) ;
#2745 = EDGE_CURVE ( 'NONE', #39003, #32420, #28311, .T. ) ;
#2744 = CARTESIAN_POINT ( 'NONE',  ( -45.59965607524345899, 31.00000000000000355, -22.47439267160796916 ) ) ;
#2746 = DIRECTION ( 'NONE',  ( -3.009274222672345096E-17, -1.000000000000000000, 2.455023325076455345E-18 ) ) ;
#2747 = VERTEX_POINT ( 'NONE', #33518 ) ;
#2748 = CARTESIAN_POINT ( 'NONE',  ( 17.99999999999999645, -11.65176648921111635, 115.4133282497342066 ) ) ;
#2749 = CARTESIAN_POINT ( 'NONE',  ( 5.726861599741335240, 31.00000000000000355, 87.39583333411552246 ) ) ;
#2750 = CIRCLE ( 'NONE', #37594, 120.5010000000000190 ) ;
#2751 = AXIS2_PLACEMENT_3D ( 'NONE', #7124, #33328, #26779 ) ;
#2752 = EDGE_CURVE ( 'NONE', #13070, #7249, #7372, .T. ) ;
#2753 = AXIS2_PLACEMENT_3D ( 'NONE', #15765, #39265, #32744 ) ;
#2754 = DIRECTION ( 'NONE',  ( -1.000000000000000000, -0.000000000000000000, -0.000000000000000000 ) ) ;
#2755 = ORIENTED_EDGE ( 'NONE', *, *, #4486, .F. ) ;
#2756 = CARTESIAN_POINT ( 'NONE',  ( 22.12550800842194931, 31.00000000000000355, 65.48657384636695156 ) ) ;
#2757 = CARTESIAN_POINT ( 'NONE',  ( -61.81085491475939619, 40.00000000000000711, 35.57109242552864004 ) ) ;
#2758 = CARTESIAN_POINT ( 'NONE',  ( 91.55691129138550366, 39.99999999999999289, -24.53049628908797430 ) ) ;
#2759 = VERTEX_POINT ( 'NONE', #42193 ) ;
#2760 = DIRECTION ( 'NONE',  ( 0.000000000000000000, 0.000000000000000000, 1.000000000000000000 ) ) ;
#2761 = CYLINDRICAL_SURFACE ( 'NONE', #8935, 51.99999999999999289 ) ;
#2762 = DIRECTION ( 'NONE',  ( -1.058513553088275437E-16, -1.000000000000000000, 8.813324511995299047E-17 ) ) ;
#2764 = ORIENTED_EDGE ( 'NONE', *, *, #7843, .F. ) ;
#2763 = DIRECTION ( 'NONE',  ( -1.000000000000000000, -0.000000000000000000, -0.000000000000000000 ) ) ;
#2765 = DIRECTION ( 'NONE',  ( 0.000000000000000000, 0.000000000000000000, 1.000000000000000000 ) ) ;
#2766 = CARTESIAN_POINT ( 'NONE',  ( -10.00000000000000000, 0.000000000000000000, 0.000000000000000000 ) ) ;
#2767 = EDGE_CURVE ( 'NONE', #35289, #2262, #35243, .T. ) ;
#2768 = CARTESIAN_POINT ( 'NONE',  ( -43.59452257625678584, 40.00000000000000000, -56.81327804312699925 ) ) ;
#2769 = CARTESIAN_POINT ( 'NONE',  ( 0.000000000000000000, -45.78515115856033901, -12.64416602183713856 ) ) ;
#2770 = ORIENTED_EDGE ( 'NONE', *, *, #42290, .F. ) ;
#2771 = DIRECTION ( 'NONE',  ( 0.000000000000000000, 0.000000000000000000, 1.000000000000000000 ) ) ;
#2772 = EDGE_CURVE ( 'NONE', #25229, #31096, #24877, .T. ) ;
#2773 = CARTESIAN_POINT ( 'NONE',  ( 9.000000000000000000, 34.45183346761135113, 10.44371441202667761 ) ) ;
#2774 = ORIENTED_EDGE ( 'NONE', *, *, #15826, .T. ) ;
#2775 = EDGE_CURVE ( 'NONE', #32990, #28231, #10885, .T. ) ;
#2776 = EDGE_LOOP ( 'NONE', ( #27954, #37139, #41972, #27995 ) ) ;
#2777 = CYLINDRICAL_SURFACE ( 'NONE', #12164, 59.00000000000000000 ) ;
#2779 = ORIENTED_EDGE ( 'NONE', *, *, #6027, .T. ) ;
#2778 = CIRCLE ( 'NONE', #1400, 59.00000000000000000 ) ;
#2780 = CARTESIAN_POINT ( 'NONE',  ( 0.000000000000000000, -44.61570720899084819, -14.73072383765613047 ) ) ;
#2781 = AXIS2_PLACEMENT_3D ( 'NONE', #13245, #6661, #20025 ) ;
#2782 = CARTESIAN_POINT ( 'NONE',  ( 0.000000000000000000, 0.000000000000000000, 0.000000000000000000 ) ) ;
#2783 = AXIS2_PLACEMENT_3D ( 'NONE', #2780, #15513, #25962 ) ;
#2784 = CARTESIAN_POINT ( 'NONE',  ( 17.99999999999999645, 23.87611429743691360, -20.54551452399595135 ) ) ;
#2785 = AXIS2_PLACEMENT_3D ( 'NONE', #22316, #32940, #3016 ) ;
#2786 = DIRECTION ( 'NONE',  ( -1.000000000000000000, 0.000000000000000000, -0.000000000000000000 ) ) ;
#2787 = ORIENTED_EDGE ( 'NONE', *, *, #5774, .F. ) ;
#2788 = CARTESIAN_POINT ( 'NONE',  ( 0.000000000000000000, 0.000000000000000000, 9.999999999999998224 ) ) ;
#2789 = ORIENTED_EDGE ( 'NONE', *, *, #10317, .T. ) ;
#2790 = DIRECTION ( 'NONE',  ( 0.000000000000000000, 0.000000000000000000, 1.000000000000000000 ) ) ;
#2791 = EDGE_CURVE ( 'NONE', #36354, #9697, #17894, .T. ) ;
#2792 = ADVANCED_FACE ( 'NONE', ( #41337 ), #21776, .F. ) ;
#2793 = EDGE_LOOP ( 'NONE', ( #39259, #22003, #16775, #1803 ) ) ;
#2794 = DIRECTION ( 'NONE',  ( -1.000000000000000000, -0.000000000000000000, -0.000000000000000000 ) ) ;
#2795 = EDGE_CURVE ( 'NONE', #34535, #18339, #15424, .T. ) ;
#2796 = EDGE_CURVE ( 'NONE', #41293, #28005, #41533, .T. ) ;
#2797 = DIRECTION ( 'NONE',  ( 0.000000000000000000, -6.982962677686265922E-15, 1.000000000000000000 ) ) ;
#2798 = CARTESIAN_POINT ( 'NONE',  ( 0.000000000000000000, 0.7408941433508176022, 0.000000000000000000 ) ) ;
#2799 = CARTESIAN_POINT ( 'NONE',  ( -54.58798567973315841, 31.00000000000000355, -26.90590473539369754 ) ) ;
#2800 = CARTESIAN_POINT ( 'NONE',  ( -8.920000000000003482, 1.356908653455267209E-15, -11.08000000000000007 ) ) ;
#2801 = AXIS2_PLACEMENT_3D ( 'NONE', #22721, #9598, #2797 ) ;
#2802 = ORIENTED_EDGE ( 'NONE', *, *, #1862, .T. ) ;
#2803 = CARTESIAN_POINT ( 'NONE',  ( -29.88476798293162418, 31.00000000000000355, 10.10044382456042911 ) ) ;
#2804 = CARTESIAN_POINT ( 'NONE',  ( 48.66231590555653241, 39.99999999999999289, -55.48862040801123641 ) ) ;
#2805 = VECTOR ( 'NONE', #22454, 1000.000000000000000 ) ;
#2806 = AXIS2_PLACEMENT_3D ( 'NONE', #32221, #2097, #15460 ) ;
#2807 = DIRECTION ( 'NONE',  ( 1.000000000000000000, 0.000000000000000000, -0.000000000000000000 ) ) ;
#2808 = DIRECTION ( 'NONE',  ( 0.000000000000000000, 0.000000000000000000, 1.000000000000000000 ) ) ;
#2809 = AXIS2_PLACEMENT_3D ( 'NONE', #26393, #39661, #36387 ) ;
#2810 = AXIS2_PLACEMENT_3D ( 'NONE', #21371, #24630, #4285 ) ;
#2811 = DIRECTION ( 'NONE',  ( -1.000000000000000000, 0.000000000000000000, 0.000000000000000000 ) ) ;
#2812 = DIRECTION ( 'NONE',  ( 0.000000000000000000, 0.000000000000000000, 1.000000000000000000 ) ) ;
#2813 = EDGE_CURVE ( 'NONE', #2738, #35175, #1861, .T. ) ;
#2814 = VERTEX_POINT ( 'NONE', #28725 ) ;
#2815 = CARTESIAN_POINT ( 'NONE',  ( 43.15607885788778475, 40.00000000000000000, -11.56636786368396486 ) ) ;
#2816 = DIRECTION ( 'NONE',  ( 1.000000000000000000, 0.000000000000000000, 0.000000000000000000 ) ) ;
#2817 = DIRECTION ( 'NONE',  ( 1.000000000000000000, 0.000000000000000000, -3.273063162220416457E-16 ) ) ;
#2818 = VECTOR ( 'NONE', #36838, 1000.000000000000000 ) ;
#2819 = ORIENTED_EDGE ( 'NONE', *, *, #10470, .T. ) ;
#2820 = EDGE_CURVE ( 'NONE', #40482, #23547, #8777, .T. ) ;
#2821 = DIRECTION ( 'NONE',  ( -1.000000000000000000, -0.000000000000000000, 0.000000000000000000 ) ) ;
#2822 = FACE_OUTER_BOUND ( 'NONE', #20800, .T. ) ;
#2823 = EDGE_LOOP ( 'NONE', ( #25792, #29092 ) ) ;
#2824 = CARTESIAN_POINT ( 'NONE',  ( -6.473970235329672780E-16, -4.862606272033106691, -3.745885042887442395 ) ) ;
#2825 = ORIENTED_EDGE ( 'NONE', *, *, #10355, .F. ) ;
#2826 = ORIENTED_EDGE ( 'NONE', *, *, #8648, .T. ) ;
#2827 = CARTESIAN_POINT ( 'NONE',  ( 17.99999999999999645, -104.2166695095716591, 60.49278301857773243 ) ) ;
#2828 = CARTESIAN_POINT ( 'NONE',  ( -23.42519174998115616, 31.00000000000000355, 87.00664592748896098 ) ) ;
#2829 = VERTEX_POINT ( 'NONE', #22200 ) ;
#2830 = CARTESIAN_POINT ( 'NONE',  ( -6.004904395537136175, 0.000000000000000000, 0.000000000000000000 ) ) ;
#2831 = DIRECTION ( 'NONE',  ( 1.000000000000000000, 0.000000000000000000, 0.000000000000000000 ) ) ;
#2832 = AXIS2_PLACEMENT_3D ( 'NONE', #35023, #14555, #27862 ) ;
#2833 = FACE_OUTER_BOUND ( 'NONE', #41844, .T. ) ;
#2834 = ORIENTED_EDGE ( 'NONE', *, *, #5212, .T. ) ;
#2835 = DIRECTION ( 'NONE',  ( -1.000000000000000000, 0.000000000000000000, 0.000000000000000000 ) ) ;
#2836 = LINE ( 'NONE', #20515, #32471 ) ;
#2837 = VECTOR ( 'NONE', #8399, 1000.000000000000000 ) ;
#2838 = LINE ( 'NONE', #29941, #29689 ) ;
#2839 = ADVANCED_FACE ( 'NONE', ( #38717 ), #11930, .F. ) ;
#2840 = EDGE_CURVE ( 'NONE', #38342, #12939, #35452, .T. ) ;
#2842 = FACE_BOUND ( 'NONE', #18369, .T. ) ;
#2841 = LINE ( 'NONE', #2210, #7110 ) ;
#2843 = ADVANCED_FACE ( 'NONE', ( #18927, #32184, #37854 ), #28929, .F. ) ;
#2844 = EDGE_CURVE ( 'NONE', #5301, #8980, #31341, .T. ) ;
#2845 = CIRCLE ( 'NONE', #39, 59.00000000000000711 ) ;
#2846 = DIRECTION ( 'NONE',  ( 1.000000000000000000, 0.000000000000000000, 0.000000000000000000 ) ) ;
#2847 = EDGE_LOOP ( 'NONE', ( #27807, #15265 ) ) ;
#2848 = EDGE_CURVE ( 'NONE', #14923, #25035, #4710, .T. ) ;
#2849 = CARTESIAN_POINT ( 'NONE',  ( 7.028922914820973311, 31.00000000000000355, 26.21578750688660264 ) ) ;
#2850 = VECTOR ( 'NONE', #32606, 1000.000000000000000 ) ;
#2851 = EDGE_LOOP ( 'NONE', ( #32167, #18591, #2081, #11622 ) ) ;
#2852 = CARTESIAN_POINT ( 'NONE',  ( -139.4999999999999716, 1.517807346132291325E-13, -40.00000000000005684 ) ) ;
#2853 = DIRECTION ( 'NONE',  ( -1.000000000000000000, -0.000000000000000000, -0.000000000000000000 ) ) ;
#2854 = ORIENTED_EDGE ( 'NONE', *, *, #26962, .F. ) ;
#2855 = DIRECTION ( 'NONE',  ( -1.000000000000000000, -0.000000000000000000, -0.000000000000000000 ) ) ;
#2856 = CARTESIAN_POINT ( 'NONE',  ( 2.781618486875130358, 40.00000000000000000, -42.60416666509636485 ) ) ;
#2857 = CARTESIAN_POINT ( 'NONE',  ( -17.88900094062007184, 40.00000000000000000, 36.12696699726038219 ) ) ;
#2858 = ORIENTED_EDGE ( 'NONE', *, *, #35961, .F. ) ;
#2859 = ORIENTED_EDGE ( 'NONE', *, *, #30376, .F. ) ;
#2860 = CARTESIAN_POINT ( 'NONE',  ( 0.000000000000000000, 0.6819280456844267757, -115.9979955608738607 ) ) ;
#2861 = DIRECTION ( 'NONE',  ( 0.000000000000000000, 0.000000000000000000, 1.000000000000000000 ) ) ;
#2862 = CARTESIAN_POINT ( 'NONE',  ( 17.99999999999999645, 0.000000000000000000, 0.000000000000000000 ) ) ;
#2863 = LINE ( 'NONE', #6584, #20262 ) ;
#2864 = VERTEX_POINT ( 'NONE', #38298 ) ;
#2865 = DIRECTION ( 'NONE',  ( 0.000000000000000000, -0.8183027759081743513, 0.5747874102143993857 ) ) ;
#2866 = ORIENTED_EDGE ( 'NONE', *, *, #18599, .T. ) ;
#2867 = DIRECTION ( 'NONE',  ( 0.000000000000000000, 0.7980172272802408262, -0.6026346363792547400 ) ) ;
#2868 = CIRCLE ( 'NONE', #26589, 20.00000000000000711 ) ;
#2869 = CARTESIAN_POINT ( 'NONE',  ( 17.99999999999999645, 88.00363688980546328, 82.31555682352686176 ) ) ;
#2870 = AXIS2_PLACEMENT_3D ( 'NONE', #12810, #19589, #42458 ) ;
#2871 = CYLINDRICAL_SURFACE ( 'NONE', #42323, 20.00000000000000355 ) ;
#2872 = AXIS2_PLACEMENT_3D ( 'NONE', #31527, #24580, #7523 ) ;
#2873 = DIRECTION ( 'NONE',  ( -1.000000000000000000, 0.000000000000000000, 0.000000000000000000 ) ) ;
#2874 = ORIENTED_EDGE ( 'NONE', *, *, #39352, .F. ) ;
#2875 = CARTESIAN_POINT ( 'NONE',  ( -10.00000000000000000, 0.000000000000000000, 0.000000000000000000 ) ) ;
#2876 = ORIENTED_EDGE ( 'NONE', *, *, #26728, .T. ) ;
#2877 = DIRECTION ( 'NONE',  ( 1.000000000000000000, 0.000000000000000000, 0.000000000000000000 ) ) ;
#2878 = VECTOR ( 'NONE', #18435, 1000.000000000000000 ) ;
#2879 = VERTEX_POINT ( 'NONE', #21569 ) ;
#2881 = VERTEX_POINT ( 'NONE', #38082 ) ;
#2880 = DIRECTION ( 'NONE',  ( 0.000000000000000000, 0.000000000000000000, 1.000000000000000000 ) ) ;
#2882 = CARTESIAN_POINT ( 'NONE',  ( 67.09393615762301977, 31.00000000000000000, 4.495243625008654043 ) ) ;
#2883 = ORIENTED_EDGE ( 'NONE', *, *, #20947, .T. ) ;
#2884 = DIRECTION ( 'NONE',  ( -1.000000000000000000, -0.000000000000000000, 0.000000000000000000 ) ) ;
#2885 = ORIENTED_EDGE ( 'NONE', *, *, #7704, .T. ) ;
#2886 = DIRECTION ( 'NONE',  ( 1.000000000000000000, 0.000000000000000000, 0.000000000000000000 ) ) ;
#2887 = ORIENTED_EDGE ( 'NONE', *, *, #22540, .F. ) ;
#2888 = CARTESIAN_POINT ( 'NONE',  ( -70.49178429274644486, 40.00000000000000711, 40.57739572807859929 ) ) ;
#2890 = CARTESIAN_POINT ( 'NONE',  ( 0.000000000000000000, -36.34385289850609979, 29.77717097092063270 ) ) ;
#2889 = CARTESIAN_POINT ( 'NONE',  ( 0.000000000000000000, -59.07817985938929439, -105.0250430397515089 ) ) ;
#2891 = EDGE_CURVE ( 'NONE', #21142, #13428, #13691, .T. ) ;
#2892 = EDGE_CURVE ( 'NONE', #42055, #36478, #33845, .T. ) ;
#2893 = DIRECTION ( 'NONE',  ( -3.996523416598930318E-16, 2.658563593772947863E-15, 1.000000000000000000 ) ) ;
#2894 = VERTEX_POINT ( 'NONE', #36297 ) ;
#2895 = CYLINDRICAL_SURFACE ( 'NONE', #39069, 59.00000000000000000 ) ;
#2896 = ORIENTED_EDGE ( 'NONE', *, *, #26699, .F. ) ;
#2897 =( NAMED_UNIT ( * ) PLANE_ANGLE_UNIT ( ) SI_UNIT ( $, .RADIAN. ) );
#2898 = EDGE_CURVE ( 'NONE', #24559, #19290, #15079, .T. ) ;
#2899 = AXIS2_PLACEMENT_3D ( 'NONE', #35121, #37961, #5463 ) ;
#2900 = AXIS2_PLACEMENT_3D ( 'NONE', #38184, #31229, #17728 ) ;
#2901 = DIRECTION ( 'NONE',  ( 1.000000000000000000, 0.000000000000000000, 0.000000000000000000 ) ) ;
#2902 = CARTESIAN_POINT ( 'NONE',  ( -80.96080130434580724, -14.05525454449571043, 14.45886780445738395 ) ) ;
#2903 = CARTESIAN_POINT ( 'NONE',  ( -5.072363130230006512, 31.00000000000000355, 77.60416666578095146 ) ) ;
#2905 = DIRECTION ( 'NONE',  ( 1.000000000000000000, 0.000000000000000000, 0.000000000000000000 ) ) ;
#2904 = DIRECTION ( 'NONE',  ( -0.000000000000000000, -0.000000000000000000, -1.000000000000000000 ) ) ;
#2906 = EDGE_LOOP ( 'NONE', ( #9783, #11514, #36033, #10931 ) ) ;
#2907 = AXIS2_PLACEMENT_3D ( 'NONE', #14203, #27079, #6977 ) ;
#2908 = ADVANCED_FACE ( 'NONE', ( #22406 ), #15841, .T. ) ;
#2909 = FACE_OUTER_BOUND ( 'NONE', #3989, .T. ) ;
#2910 = CIRCLE ( 'NONE', #14123, 116.0000000000000000 ) ;
#2911 = EDGE_CURVE ( 'NONE', #38131, #41436, #35861, .T. ) ;
#2912 = ORIENTED_EDGE ( 'NONE', *, *, #9169, .T. ) ;
#2913 = CARTESIAN_POINT ( 'NONE',  ( 17.99999999999999645, 103.5682682299982673, 43.14958040911701431 ) ) ;
#2914 = CYLINDRICAL_SURFACE ( 'NONE', #35975, 59.00000000000000000 ) ;
#2915 = CARTESIAN_POINT ( 'NONE',  ( -79.17211737996690601, 31.00000000000000711, 45.58486055166099504 ) ) ;
#2916 = CARTESIAN_POINT ( 'NONE',  ( 6.309545988805658645, 40.00000000000000000, -94.59213238963913284 ) ) ;
#2917 = CARTESIAN_POINT ( 'NONE',  ( 0.000000000000000000, 31.11570115861495367, 4.898994019976747438 ) ) ;
#2918 = DIRECTION ( 'NONE',  ( -1.000000000000000000, 0.000000000000000000, 0.000000000000000000 ) ) ;
#2919 = ORIENTED_EDGE ( 'NONE', *, *, #4989, .T. ) ;
#2920 = CARTESIAN_POINT ( 'NONE',  ( 0.000000000000000000, 2.418575551220858877, 120.4767259403369053 ) ) ;
#2921 = EDGE_LOOP ( 'NONE', ( #3255, #21732, #7590, #19568 ) ) ;
#2922 = CARTESIAN_POINT ( 'NONE',  ( 0.000000000000000000, 88.56657216608705596, -68.87840567545838155 ) ) ;
#2923 = CARTESIAN_POINT ( 'NONE',  ( 17.99999999999999645, 106.6051926090976991, -45.73109345704713036 ) ) ;
#2924 = CARTESIAN_POINT ( 'NONE',  ( -6.259644161404860030E-16, -4.618802153517027165, -3.433295621305388234 ) ) ;
#2925 = VERTEX_POINT ( 'NONE', #36087 ) ;
#2926 = CARTESIAN_POINT ( 'NONE',  ( 5.657435538624008755E-15, 4.615443851143735910E-16, 0.000000000000000000 ) ) ;
#2927 = DIRECTION ( 'NONE',  ( -1.000000000000000000, 0.000000000000000000, -0.000000000000000000 ) ) ;
#2928 = VECTOR ( 'NONE', #11986, 1000.000000000000000 ) ;
#2929 = CARTESIAN_POINT ( 'NONE',  ( 17.99999999999999645, 80.02407177073062883, -78.64108602299866391 ) ) ;
#2930 = AXIS2_PLACEMENT_3D ( 'NONE', #9324, #2963, #35932 ) ;
#2932 = VERTEX_POINT ( 'NONE', #36505 ) ;
#2931 = CARTESIAN_POINT ( 'NONE',  ( -9.000000000000005329, 0.000000000000000000, 0.000000000000000000 ) ) ;
#2933 = CARTESIAN_POINT ( 'NONE',  ( -20.42974159057666483, 31.00000000000000355, -10.07157319949386753 ) ) ;
#2934 = FACE_OUTER_BOUND ( 'NONE', #37750, .T. ) ;
#2936 = ORIENTED_EDGE ( 'NONE', *, *, #29273, .T. ) ;
#2935 = FACE_OUTER_BOUND ( 'NONE', #3580, .T. ) ;
#2937 = UNCERTAINTY_MEASURE_WITH_UNIT (LENGTH_MEASURE( 1.000000000000000082E-05 ), #7508, 'distance_accuracy_value', 'NONE');
#2938 = ORIENTED_EDGE ( 'NONE', *, *, #3217, .F. ) ;
#2939 = DIRECTION ( 'NONE',  ( 0.000000000000000000, 0.000000000000000000, 1.000000000000000000 ) ) ;
#2940 = DIRECTION ( 'NONE',  ( 1.000000000000000000, -0.000000000000000000, -0.000000000000000000 ) ) ;
#2941 = CARTESIAN_POINT ( 'NONE',  ( -41.03896728212566103, 40.00000000000000000, -11.06873348903577892 ) ) ;
#2942 = CARTESIAN_POINT ( 'NONE',  ( 8.919999999999996376, 0.000000000000000000, 14.91999999999999815 ) ) ;
#2943 = DIRECTION ( 'NONE',  ( 1.000000000000000000, 0.000000000000000000, 0.000000000000000000 ) ) ;
#2944 = EDGE_CURVE ( 'NONE', #19475, #30260, #41418, .T. ) ;
#2945 = DIRECTION ( 'NONE',  ( -1.000000000000000000, 0.000000000000000000, -0.000000000000000000 ) ) ;
#2946 = ORIENTED_EDGE ( 'NONE', *, *, #21666, .F. ) ;
#2947 = DIRECTION ( 'NONE',  ( -1.000000000000000000, 0.000000000000000000, 0.000000000000000000 ) ) ;
#2948 = VERTEX_POINT ( 'NONE', #19551 ) ;
#2949 = CARTESIAN_POINT ( 'NONE',  ( 0.000000000000000000, 0.000000000000000000, 0.000000000000000000 ) ) ;
#2950 = CARTESIAN_POINT ( 'NONE',  ( -109.0695705685756138, 106.4195705685752529, 6.999999999999998224 ) ) ;
#2951 = CARTESIAN_POINT ( 'NONE',  ( -6.851565232941113415, 31.00000000000000355, -51.95325991929587417 ) ) ;
#2952 = DIRECTION ( 'NONE',  ( -1.000000000000000000, 0.000000000000000000, -0.000000000000000000 ) ) ;
#2953 = ORIENTED_EDGE ( 'NONE', *, *, #5829, .F. ) ;
#2954 = EDGE_CURVE ( 'NONE', #20442, #13064, #5771, .T. ) ;
#2955 = DIRECTION ( 'NONE',  ( 0.000000000000000000, 0.000000000000000000, 1.000000000000000000 ) ) ;
#2956 = AXIS2_PLACEMENT_3D ( 'NONE', #10609, #37211, #30256 ) ;
#2957 = CARTESIAN_POINT ( 'NONE',  ( 84.66040299356156140, 31.00000000000000000, 11.14692016787551765 ) ) ;
#2958 = EDGE_CURVE ( 'NONE', #27071, #39096, #22663, .T. ) ;
#2959 = DIRECTION ( 'NONE',  ( 0.000000000000000000, 0.000000000000000000, 1.000000000000000000 ) ) ;
#2960 = ORIENTED_EDGE ( 'NONE', *, *, #28767, .T. ) ;
#2961 = CARTESIAN_POINT ( 'NONE',  ( -9.228224334391116557, 31.00000000000000355, 69.24269282083176336 ) ) ;
#2962 = CARTESIAN_POINT ( 'NONE',  ( 30.38134496340388324, 40.00000000000000000, 61.85720693096894252 ) ) ;
#2963 = DIRECTION ( 'NONE',  ( -1.000000000000000000, 0.000000000000000000, 0.000000000000000000 ) ) ;
#2964 = MECHANICAL_DESIGN_GEOMETRIC_PRESENTATION_REPRESENTATION (  '', ( #19081 ), #14178 ) ;
#2965 = VERTEX_POINT ( 'NONE', #39777 ) ;
#2966 = VECTOR ( 'NONE', #36400, 1000.000000000000000 ) ;
#2967 = CARTESIAN_POINT ( 'NONE',  ( -142.5000000000000000, 1.627194001049080943E-13, -45.00000000000004974 ) ) ;
#2968 = DIRECTION ( 'NONE',  ( 0.000000000000000000, -1.000000000000000000, 0.000000000000000000 ) ) ;
#2969 = DIRECTION ( 'NONE',  ( -1.000000000000000000, 0.000000000000000000, 0.000000000000000000 ) ) ;
#2971 = ORIENTED_EDGE ( 'NONE', *, *, #29004, .T. ) ;
#2970 = CARTESIAN_POINT ( 'NONE',  ( 4.154306624731137099, 2.398490048084935822, -3.721999068284414847 ) ) ;
#2972 = CARTESIAN_POINT ( 'NONE',  ( 17.99999999999999645, 109.1131968883998695, -26.12628443611929896 ) ) ;
#2973 = VERTEX_POINT ( 'NONE', #29149 ) ;
#2974 = DIRECTION ( 'NONE',  ( -1.000000000000000000, 0.000000000000000000, 0.000000000000000000 ) ) ;
#2975 = EDGE_CURVE ( 'NONE', #7939, #15282, #32818, .T. ) ;
#2976 = CARTESIAN_POINT ( 'NONE',  ( -10.16518460146908787, 40.00000000000000000, 77.20874865269769316 ) ) ;
#2977 = CARTESIAN_POINT ( 'NONE',  ( 126.0000000000000568, -2.077321393419925476E-13, -39.99999999999992895 ) ) ;
#2978 = EDGE_CURVE ( 'NONE', #33352, #41276, #42416, .T. ) ;
#2979 = APPLICATION_CONTEXT ( 'automotive_design' ) ;
#2980 = VERTEX_POINT ( 'NONE', #29564 ) ;
#2981 = CARTESIAN_POINT ( 'NONE',  ( 17.99999999999999645, 76.48293397876260258, 82.08917884620340999 ) ) ;
#2982 = ADVANCED_FACE ( 'NONE', ( #25881 ), #22837, .T. ) ;
#2983 = DIRECTION ( 'NONE',  ( -1.000000000000000000, 0.000000000000000000, 0.000000000000000000 ) ) ;
#2984 = VECTOR ( 'NONE', #19550, 1000.000000000000000 ) ;
#2985 = ORIENTED_EDGE ( 'NONE', *, *, #29586, .T. ) ;
#2986 = AXIS2_PLACEMENT_3D ( 'NONE', #17045, #20117, #13980 ) ;
#2987 = VERTEX_POINT ( 'NONE', #2902 ) ;
#2988 = CARTESIAN_POINT ( 'NONE',  ( 0.000000000000000000, 112.1702510623870097, 2.471285140324554153 ) ) ;
#2989 = VERTEX_POINT ( 'NONE', #12992 ) ;
#2990 = DIRECTION ( 'NONE',  ( 1.000000000000000000, 0.000000000000000000, 0.000000000000000000 ) ) ;
#2991 = CARTESIAN_POINT ( 'NONE',  ( 18.00000000000000355, 3.840921266750508156, -47.34345070675165346 ) ) ;
#2992 = CARTESIAN_POINT ( 'NONE',  ( 17.99999999999999645, 99.97660604680052643, -67.26937820704789317 ) ) ;
#2993 = CYLINDRICAL_SURFACE ( 'NONE', #22758, 13.60000000000000142 ) ;
#2994 = ORIENTED_EDGE ( 'NONE', *, *, #10680, .F. ) ;
#2996 = CARTESIAN_POINT ( 'NONE',  ( 9.000000000000001776, 13.56094713063571433, 50.20060470671744213 ) ) ;
#2995 =( GEOMETRIC_REPRESENTATION_CONTEXT ( 3 ) GLOBAL_UNCERTAINTY_ASSIGNED_CONTEXT ( ( #35544 ) ) GLOBAL_UNIT_ASSIGNED_CONTEXT ( ( #36447, #2346, #42771 ) ) REPRESENTATION_CONTEXT ( 'NONE', 'WORKASPACE' ) );
#2997 = ADVANCED_FACE ( 'NONE', ( #12356 ), #22615, .F. ) ;
#2998 = EDGE_LOOP ( 'NONE', ( #38993, #21878, #4452, #41577 ) ) ;
#2999 = CARTESIAN_POINT ( 'NONE',  ( 0.000000000000000000, -39.55064067543082018, 25.36340625197346199 ) ) ;
#3000 = ORIENTED_EDGE ( 'NONE', *, *, #12133, .T. ) ;
#3001 = LINE ( 'NONE', #6307, #5089 ) ;
#3002 = FACE_OUTER_BOUND ( 'NONE', #7141, .T. ) ;
#3003 = CIRCLE ( 'NONE', #21217, 120.5010000000000332 ) ;
#3004 = APPLICATION_PROTOCOL_DEFINITION ( 'draft international standard', 'automotive_design', 1998, #39502 ) ;
#3005 = EDGE_CURVE ( 'NONE', #27946, #17810, #34479, .T. ) ;
#3006 = DIRECTION ( 'NONE',  ( 0.000000000000000000, -0.5528000653611835347, -0.8333139190825215037 ) ) ;
#3007 = CARTESIAN_POINT ( 'NONE',  ( 42.30435120181500963, 31.00000000000000355, 37.09784777058769123 ) ) ;
#3008 = EDGE_CURVE ( 'NONE', #23020, #21806, #5211, .T. ) ;
#3009 = VERTEX_POINT ( 'NONE', #12774 ) ;
#3010 = CARTESIAN_POINT ( 'NONE',  ( 36.89914868738900822, 31.00000000000000355, -2.354335741662294534 ) ) ;
#3011 = CARTESIAN_POINT ( 'NONE',  ( -35.92146702467432817, 40.00000000000000000, -62.19081021767443218 ) ) ;
#3012 = VECTOR ( 'NONE', #5209, 1000.000000000000000 ) ;
#3013 = CARTESIAN_POINT ( 'NONE',  ( 18.00000000000000355, 30.93515269692163017, -36.04401931830219752 ) ) ;
#3014 = CARTESIAN_POINT ( 'NONE',  ( 0.000000000000000000, 10.40101730206365716, 120.0512800434971581 ) ) ;
#3015 = DIRECTION ( 'NONE',  ( 0.000000000000000000, 0.000000000000000000, 1.000000000000000000 ) ) ;
#3016 = DIRECTION ( 'NONE',  ( 0.000000000000000000, 0.000000000000000000, 1.000000000000000000 ) ) ;
#3017 = AXIS2_PLACEMENT_3D ( 'NONE', #1323, #10503, #14666 ) ;
#3018 = ORIENTED_EDGE ( 'NONE', *, *, #7101, .F. ) ;
#3019 = CARTESIAN_POINT ( 'NONE',  ( -32.63632984357925437, 40.00000000000000000, -25.02932899672474676 ) ) ;
#3020 = DIRECTION ( 'NONE',  ( -1.000000000000000000, 1.373900992973641868E-15, 3.469446951953632924E-16 ) ) ;
#3021 = CIRCLE ( 'NONE', #21210, 13.59999999999999964 ) ;
#3022 = CARTESIAN_POINT ( 'NONE',  ( 0.000000000000000000, 101.1249659627855806, -48.60055280209454054 ) ) ;
#3023 = ORIENTED_EDGE ( 'NONE', *, *, #28442, .F. ) ;
#3024 = ADVANCED_FACE ( 'NONE', ( #26080 ), #9700, .F. ) ;
#3025 = DIRECTION ( 'NONE',  ( -1.000000000000000000, -0.000000000000000000, 0.000000000000000000 ) ) ;
#3026 = LINE ( 'NONE', #22969, #13149 ) ;
#3027 = PRODUCT_DEFINITION ( 'UNKNOWN', '', #1688, #36991 ) ;
#3028 = ORIENTED_EDGE ( 'NONE', *, *, #8866, .T. ) ;
#3029 = FACE_OUTER_BOUND ( 'NONE', #8660, .T. ) ;
#3030 = EDGE_LOOP ( 'NONE', ( #39867, #18777, #540, #13187 ) ) ;
#3031 = AXIS2_PLACEMENT_3D ( 'NONE', #30092, #22936, #6495 ) ;
#3032 = ORIENTED_EDGE ( 'NONE', *, *, #15639, .F. ) ;
#3033 = VECTOR ( 'NONE', #34781, 1000.000000000000000 ) ;
#3034 = CARTESIAN_POINT ( 'NONE',  ( 17.99999999999999645, -99.97660604679919061, -67.26937820704989690 ) ) ;
#3035 = CARTESIAN_POINT ( 'NONE',  ( 22.98560153734151257, 31.00000000000000355, 86.26083236265422727 ) ) ;
#3036 = ORIENTED_EDGE ( 'NONE', *, *, #35516, .T. ) ;
#3037 = CARTESIAN_POINT ( 'NONE',  ( 5.200000000000002842, 3.061616997868383634E-16, -2.500000000000000444 ) ) ;
#3038 = CIRCLE ( 'NONE', #25419, 120.5010000000000474 ) ;
#3039 = DIRECTION ( 'NONE',  ( -1.000000000000000000, 0.000000000000000000, 0.000000000000000000 ) ) ;
#3040 = DIRECTION ( 'NONE',  ( 1.000000000000000000, 0.000000000000000000, 0.000000000000000000 ) ) ;
#3041 = ORIENTED_EDGE ( 'NONE', *, *, #5596, .F. ) ;
#3042 = FACE_OUTER_BOUND ( 'NONE', #8836, .T. ) ;
#3043 = EDGE_CURVE ( 'NONE', #3310, #14855, #29615, .T. ) ;
#3044 = AXIS2_PLACEMENT_3D ( 'NONE', #14359, #1446, #11296 ) ;
#3045 = CARTESIAN_POINT ( 'NONE',  ( -0.5999999999999996447, -12.75000000000000000, -1.199999999999999956 ) ) ;
#3047 = PLANE ( 'NONE',  #26230 ) ;
#3046 = CYLINDRICAL_SURFACE ( 'NONE', #12012, 14.99999999999999822 ) ;
#3048 = FACE_OUTER_BOUND ( 'NONE', #2199, .T. ) ;
#3049 = ORIENTED_EDGE ( 'NONE', *, *, #26660, .T. ) ;
#3050 = SHAPE_REPRESENTATION_RELATIONSHIP ( 'NONE' , 'NONE' ,  #18009, #29693 ) ;
#3051 = EDGE_CURVE ( 'NONE', #21806, #33051, #29789, .T. ) ;
#3052 = ADVANCED_BREP_SHAPE_REPRESENTATION ( '', ( #27661, #13552 ), #23961 ) ;
#3053 = CARTESIAN_POINT ( 'NONE',  ( -10.31048697494744815, 31.00000000000000355, -30.34325702988586215 ) ) ;
#3054 = AXIS2_PLACEMENT_3D ( 'NONE', #15330, #18184, #28618 ) ;
#3055 = EDGE_LOOP ( 'NONE', ( #39156, #19434 ) ) ;
#3056 = CARTESIAN_POINT ( 'NONE',  ( 18.00000000000000355, 5.667686777402355602, -46.64153600743599526 ) ) ;
#3057 = EDGE_CURVE ( 'NONE', #8971, #16736, #14291, .T. ) ;
#3058 = LINE ( 'NONE', #36899, #31194 ) ;
#3059 = VERTEX_POINT ( 'NONE', #17792 ) ;
#3060 = CARTESIAN_POINT ( 'NONE',  ( 18.00000000000000355, 49.25004636492411692, -16.68630974939707556 ) ) ;
#3061 = CARTESIAN_POINT ( 'NONE',  ( -23.50435451693408950, 40.00000000000000000, 30.64856077952424940 ) ) ;
#3062 = CARTESIAN_POINT ( 'NONE',  ( 20.11321884379431779, 40.00000000000000000, -40.61652209560084259 ) ) ;
#3063 = ORIENTED_EDGE ( 'NONE', *, *, #38288, .T. ) ;
#3064 = VECTOR ( 'NONE', #10682, 1000.000000000000000 ) ;
#3065 = ORIENTED_EDGE ( 'NONE', *, *, #22670, .T. ) ;
#3066 = FACE_BOUND ( 'NONE', #13828, .T. ) ;
#3067 = FACE_OUTER_BOUND ( 'NONE', #30229, .T. ) ;
#3068 = VECTOR ( 'NONE', #11070, 1000.000000000000000 ) ;
#3069 = DIRECTION ( 'NONE',  ( -1.000000000000000000, -0.000000000000000000, -0.000000000000000000 ) ) ;
#3070 = CARTESIAN_POINT ( 'NONE',  ( 0.000000000000000000, -47.31079789947416003, -105.9135893174955783 ) ) ;
#3071 = DIRECTION ( 'NONE',  ( -1.000000000000000000, -0.000000000000000000, 0.000000000000000000 ) ) ;
#3072 = AXIS2_PLACEMENT_3D ( 'NONE', #19367, #2713, #18954 ) ;
#3073 = ORIENTED_EDGE ( 'NONE', *, *, #16811, .F. ) ;
#3074 = DIRECTION ( 'NONE',  ( -1.000000000000000000, -0.000000000000000000, -0.000000000000000000 ) ) ;
#3075 = VERTEX_POINT ( 'NONE', #10561 ) ;
#3076 = CARTESIAN_POINT ( 'NONE',  ( 8.999999999999998224, -42.87700105098536341, -107.7847984684009219 ) ) ;
#3077 = FACE_OUTER_BOUND ( 'NONE', #3567, .T. ) ;
#3078 = EDGE_CURVE ( 'NONE', #4859, #12278, #2379, .T. ) ;
#3079 = ORIENTED_EDGE ( 'NONE', *, *, #22378, .F. ) ;
#3080 = EDGE_CURVE ( 'NONE', #18124, #23222, #10064, .T. ) ;
#3081 = CARTESIAN_POINT ( 'NONE',  ( 18.00000000000000355, 17.50309955389674954, -43.60271849949345579 ) ) ;
#3082 = ADVANCED_FACE ( 'NONE', ( #24343 ), #10350, .T. ) ;
#3083 = EDGE_CURVE ( 'NONE', #20671, #14903, #40427, .T. ) ;
#3084 = EDGE_CURVE ( 'NONE', #11761, #34450, #26130, .T. ) ;
#3085 = PLANE ( 'NONE',  #20630 ) ;
#3086 = ORIENTED_EDGE ( 'NONE', *, *, #5442, .T. ) ;
#3087 = CARTESIAN_POINT ( 'NONE',  ( 17.99999999999999645, 72.00556975657703163, 86.04342158279412445 ) ) ;
#3088 = ORIENTED_EDGE ( 'NONE', *, *, #34298, .T. ) ;
#3089 = CARTESIAN_POINT ( 'NONE',  ( -9.000000000000005329, 0.000000000000000000, 0.000000000000000000 ) ) ;
#3090 = AXIS2_PLACEMENT_3D ( 'NONE', #25677, #7270, #26935 ) ;
#3091 = VERTEX_POINT ( 'NONE', #36947 ) ;
#3093 = VERTEX_POINT ( 'NONE', #34116 ) ;
#3092 = CARTESIAN_POINT ( 'NONE',  ( 0.000000000000000000, -27.83061035787035564, 117.2431154827796576 ) ) ;
#3094 = CARTESIAN_POINT ( 'NONE',  ( -58.36801134197498442, 31.00000000000000711, 19.71467013092928866 ) ) ;
#3095 = ORIENTED_EDGE ( 'NONE', *, *, #13067, .T. ) ;
#3096 = DIRECTION ( 'NONE',  ( 0.000000000000000000, -0.3140767120219362663, -0.9493976084683853900 ) ) ;
#3097 = CIRCLE ( 'NONE', #15714, 10.99999999999998934 ) ;
#3098 = AXIS2_PLACEMENT_3D ( 'NONE', #18010, #26754, #1141 ) ;
#3099 = EDGE_LOOP ( 'NONE', ( #10824, #21270, #1500, #32852 ) ) ;
#3100 = LINE ( 'NONE', #19538, #37682 ) ;
#3101 = VERTEX_POINT ( 'NONE', #509 ) ;
#3102 = CARTESIAN_POINT ( 'NONE',  ( 83.01093309090690298, 39.99999999999999289, 28.30804032753857058 ) ) ;
#3103 = VECTOR ( 'NONE', #9563, 1000.000000000000000 ) ;
#3104 = AXIS2_PLACEMENT_3D ( 'NONE', #18981, #25101, #21827 ) ;
#3106 = CARTESIAN_POINT ( 'NONE',  ( 17.99999999999999645, 24.22031524825977300, 109.5520369638038289 ) ) ;
#3105 = FACE_OUTER_BOUND ( 'NONE', #2067, .T. ) ;
#3107 = AXIS2_PLACEMENT_3D ( 'NONE', #7065, #60, #20214 ) ;
#3108 = CARTESIAN_POINT ( 'NONE',  ( 150.5000000000000284, 1.576403824487674918E-12, 10.00000000000000000 ) ) ;
#3109 = ORIENTED_EDGE ( 'NONE', *, *, #32690, .T. ) ;
#3110 = DIRECTION ( 'NONE',  ( 0.000000000000000000, 0.2631025642275218179, -0.9647678688145158166 ) ) ;
#3111 = EDGE_LOOP ( 'NONE', ( #33066, #27584 ) ) ;
#3112 = FILL_AREA_STYLE ('',( #265 ) ) ;
#3113 = VECTOR ( 'NONE', #19786, 1000.000000000000000 ) ;
#3114 = DIRECTION ( 'NONE',  ( -1.000000000000000000, -0.000000000000000000, -0.000000000000000000 ) ) ;
#3115 = DIRECTION ( 'NONE',  ( -1.000000000000000000, -0.000000000000000000, -0.000000000000000000 ) ) ;
#3116 = CARTESIAN_POINT ( 'NONE',  ( -68.69954721042445556, 31.00000000000000711, 39.68009708086182741 ) ) ;
#3118 = CARTESIAN_POINT ( 'NONE',  ( 17.99999999999999645, 0.000000000000000000, 0.000000000000000000 ) ) ;
#3117 = DIRECTION ( 'NONE',  ( 0.000000000000000000, 0.000000000000000000, 1.000000000000000000 ) ) ;
#3119 = EDGE_LOOP ( 'NONE', ( #30945, #2669, #1670, #1288 ) ) ;
#3120 = DIRECTION ( 'NONE',  ( -3.996523416598930318E-16, 2.658563593772947863E-15, 1.000000000000000000 ) ) ;
#3121 = ORIENTED_EDGE ( 'NONE', *, *, #24456, .F. ) ;
#3122 = DIRECTION ( 'NONE',  ( -1.000000000000000000, 0.000000000000000000, 0.000000000000000000 ) ) ;
#3123 = CARTESIAN_POINT ( 'NONE',  ( 17.99999999999999645, -0.5156212287287311735, 112.1962860721878172 ) ) ;
#3125 = CARTESIAN_POINT ( 'NONE',  ( 94.26586287999620595, 31.00000000000000000, 25.37251369639959364 ) ) ;
#3124 = AXIS2_PLACEMENT_3D ( 'NONE', #7971, #20904, #31115 ) ;
#3126 = CIRCLE ( 'NONE', #5254, 20.00000000000000711 ) ;
#3127 = LINE ( 'NONE', #29163, #268 ) ;
#3128 = AXIS2_PLACEMENT_3D ( 'NONE', #19236, #2598, #39464 ) ;
#3129 = CIRCLE ( 'NONE', #5257, 13.60000000000000320 ) ;
#3130 = VECTOR ( 'NONE', #9319, 1000.000000000000000 ) ;
#3131 = DIRECTION ( 'NONE',  ( -3.996523416598930318E-16, 2.658563593772947863E-15, 1.000000000000000000 ) ) ;
#3132 = VERTEX_POINT ( 'NONE', #16925 ) ;
#3133 = DIRECTION ( 'NONE',  ( -1.000000000000000000, 0.000000000000000000, -0.000000000000000000 ) ) ;
#3134 = ORIENTED_EDGE ( 'NONE', *, *, #22481, .T. ) ;
#3135 = CARTESIAN_POINT ( 'NONE',  ( 0.000000000000000000, 115.9750404417044081, 2.406240749597859718 ) ) ;
#3136 = AXIS2_PLACEMENT_3D ( 'NONE', #40057, #20708, #4063 ) ;
#3137 = CIRCLE ( 'NONE', #41502, 12.55910585664918422 ) ;
#3138 = CARTESIAN_POINT ( 'NONE',  ( 18.00000000000000355, 9.744342220503391161, 46.48873837489801275 ) ) ;
#3139 = EDGE_CURVE ( 'NONE', #33598, #38342, #38650, .T. ) ;
#3140 = ADVANCED_FACE ( 'NONE', ( #27588 ), #30208, .F. ) ;
#3141 = CARTESIAN_POINT ( 'NONE',  ( 18.00000000000000355, 0.000000000000000000, 0.000000000000000000 ) ) ;
#3142 = ORIENTED_EDGE ( 'NONE', *, *, #31170, .T. ) ;
#3143 = FACE_OUTER_BOUND ( 'NONE', #34090, .T. ) ;
#3144 = LINE ( 'NONE', #32642, #18684 ) ;
#3145 = ADVANCED_FACE ( 'NONE', ( #17367 ), #17578, .T. ) ;
#3146 = CIRCLE ( 'NONE', #7342, 59.00000000000000000 ) ;
#3147 = DIRECTION ( 'NONE',  ( 0.000000000000000000, -0.9574220383620022368, -0.2886919473396314384 ) ) ;
#3149 = VERTEX_POINT ( 'NONE', #925 ) ;
#3148 = CARTESIAN_POINT ( 'NONE',  ( 17.99999999999999645, 0.000000000000000000, 0.000000000000000000 ) ) ;
#3150 = CARTESIAN_POINT ( 'NONE',  ( -13.43146050690766380, 31.00000000000000355, 27.15249184975281693 ) ) ;
#3151 = DIRECTION ( 'NONE',  ( -3.469446951953614682E-16, 1.000000000000000000, 0.000000000000000000 ) ) ;
#3153 = EDGE_LOOP ( 'NONE', ( #6838, #19531, #20948, #13257 ) ) ;
#3152 = CARTESIAN_POINT ( 'NONE',  ( 17.99999999999999645, -58.30069736313598128, -100.2847380560572930 ) ) ;
#3154 = VERTEX_POINT ( 'NONE', #14279 ) ;
#3155 = DIRECTION ( 'NONE',  ( -3.009274222672345096E-17, -1.000000000000000000, 2.455023325076454960E-18 ) ) ;
#3156 = CARTESIAN_POINT ( 'NONE',  ( -19.99999999999998934, -6.025457873503454466E-14, -26.00000000000001066 ) ) ;
#3157 = CARTESIAN_POINT ( 'NONE',  ( 24.31498657911848227, 40.00000000000000000, 42.27453502171530175 ) ) ;
#3158 = CARTESIAN_POINT ( 'NONE',  ( 17.99999999999999645, 0.000000000000000000, 0.000000000000000000 ) ) ;
#3159 = EDGE_CURVE ( 'NONE', #7094, #4717, #13866, .T. ) ;
#3160 = AXIS2_PLACEMENT_3D ( 'NONE', #23041, #39772, #5766 ) ;
#3161 = DIRECTION ( 'NONE',  ( 1.000000000000000000, -0.000000000000000000, -0.000000000000000000 ) ) ;
#3162 = DIRECTION ( 'NONE',  ( -1.000000000000000000, 0.000000000000000000, 0.000000000000000000 ) ) ;
#3164 = VERTEX_POINT ( 'NONE', #40215 ) ;
#3163 = TOROIDAL_SURFACE ( 'NONE', #8769, 19.59999999999999076, 0.4000000000000001887 ) ;
#3165 = DIRECTION ( 'NONE',  ( 1.000000000000000000, 0.000000000000000000, -0.000000000000000000 ) ) ;
#3166 = AXIS2_PLACEMENT_3D ( 'NONE', #30269, #27218, #33093 ) ;
#3167 = ORIENTED_EDGE ( 'NONE', *, *, #18450, .F. ) ;
#3168 = CARTESIAN_POINT ( 'NONE',  ( -105.9879088449591933, 39.99999999999999289, -4.880719929157669945 ) ) ;
#3169 = CARTESIAN_POINT ( 'NONE',  ( 103.7695705685763556, -106.4195705685744855, 6.999999999999998224 ) ) ;
#3170 = AXIS2_PLACEMENT_3D ( 'NONE', #25052, #18077, #31766 ) ;
#3171 = CARTESIAN_POINT ( 'NONE',  ( 42.20483333784007840, 31.00000000000000355, -14.33818270462009359 ) ) ;
#3172 = DIRECTION ( 'NONE',  ( 0.000000000000000000, 0.000000000000000000, 1.000000000000000000 ) ) ;
#3174 = ORIENTED_EDGE ( 'NONE', *, *, #31855, .T. ) ;
#3173 = CIRCLE ( 'NONE', #11576, 58.99999999999999289 ) ;
#3175 = VECTOR ( 'NONE', #16415, 1000.000000000000000 ) ;
#3177 = AXIS2_PLACEMENT_3D ( 'NONE', #25955, #9574, #39214 ) ;
#3176 = CARTESIAN_POINT ( 'NONE',  ( 0.000000000000000000, -47.00885577955416039, 6.806061952192135500 ) ) ;
#3178 = EDGE_LOOP ( 'NONE', ( #37082, #26865, #38253, #32350 ) ) ;
#3179 = CARTESIAN_POINT ( 'NONE',  ( -86.05617919112455638, 31.00000000000000711, 49.70311056393224192 ) ) ;
#3180 = CYLINDRICAL_SURFACE ( 'NONE', #12967, 47.49900000000000233 ) ;
#3181 = VERTEX_POINT ( 'NONE', #27161 ) ;
#3182 = CARTESIAN_POINT ( 'NONE',  ( -62.09442273006147417, 31.00000000000000711, -4.163950221635984938 ) ) ;
#3183 = CARTESIAN_POINT ( 'NONE',  ( -31.21560191380782712, 40.00000000000000000, 63.07420938637471863 ) ) ;
#3184 = CARTESIAN_POINT ( 'NONE',  ( -99.89583333318432778, 40.00000000000000711, 6.544984695199788760 ) ) ;
#3185 = ORIENTED_EDGE ( 'NONE', *, *, #3193, .T. ) ;
#3186 = ORIENTED_EDGE ( 'NONE', *, *, #42578, .F. ) ;
#3187 = DIRECTION ( 'NONE',  ( 0.000000000000000000, -0.4817536741017223179, 0.8763066800438596982 ) ) ;
#3188 = DIRECTION ( 'NONE',  ( 0.000000000000000000, 0.6736956436465532105, 0.7390089172206626422 ) ) ;
#3189 = CARTESIAN_POINT ( 'NONE',  ( 0.000000000000000000, -5.871425383721176061, -51.66745943012289644 ) ) ;
#3190 = AXIS2_PLACEMENT_3D ( 'NONE', #42358, #6738, #5715 ) ;
#3192 = VERTEX_POINT ( 'NONE', #26715 ) ;
#3191 = DIRECTION ( 'NONE',  ( 3.009274222672345096E-17, 1.000000000000000000, -2.455023325076455345E-18 ) ) ;
#3193 = EDGE_CURVE ( 'NONE', #909, #17108, #12888, .T. ) ;
#3194 = DIRECTION ( 'NONE',  ( -1.000000000000000000, 0.000000000000000000, 0.000000000000000000 ) ) ;
#3196 = ORIENTED_EDGE ( 'NONE', *, *, #35724, .T. ) ;
#3195 = AXIS2_PLACEMENT_3D ( 'NONE', #8025, #24433, #814 ) ;
#3197 = CARTESIAN_POINT ( 'NONE',  ( 3.680118525130245732, -2.494084732383344605, -0.3507732604232533524 ) ) ;
#3198 = PRODUCT_RELATED_PRODUCT_CATEGORY ( 'part', '', ( #30486 ) ) ;
#3199 = CARTESIAN_POINT ( 'NONE',  ( 24.81019160154284720, 40.00000000000000000, 73.04493173762017477 ) ) ;
#3200 = CARTESIAN_POINT ( 'NONE',  ( 18.00000000000000355, 47.00885577955412487, 6.806061952192453468 ) ) ;
#3201 = CIRCLE ( 'NONE', #22097, 36.00000000000000000 ) ;
#3202 = ORIENTED_EDGE ( 'NONE', *, *, #24497, .F. ) ;
#3203 = VECTOR ( 'NONE', #36022, 1000.000000000000000 ) ;
#3204 = FACE_OUTER_BOUND ( 'NONE', #38418, .T. ) ;
#3205 = CARTESIAN_POINT ( 'NONE',  ( 0.000000000000000000, 44.61570720899074161, 14.73072383765644133 ) ) ;
#3206 = AXIS2_PLACEMENT_3D ( 'NONE', #34230, #836, #7398 ) ;
#3207 = EDGE_CURVE ( 'NONE', #42394, #35006, #40858, .T. ) ;
#3208 = ORIENTED_EDGE ( 'NONE', *, *, #25808, .F. ) ;
#3209 = EDGE_CURVE ( 'NONE', #21160, #38331, #18501, .T. ) ;
#3210 = VECTOR ( 'NONE', #11095, 1000.000000000000000 ) ;
#3211 = VERTEX_POINT ( 'NONE', #34325 ) ;
#3212 = FACE_BOUND ( 'NONE', #31827, .T. ) ;
#3213 = ORIENTED_EDGE ( 'NONE', *, *, #4490, .F. ) ;
#3214 = CARTESIAN_POINT ( 'NONE',  ( -15.43003214871520434, 40.00000000000000000, -17.59684744742188300 ) ) ;
#3215 = DIRECTION ( 'NONE',  ( 1.000000000000000000, 0.000000000000000000, 0.000000000000000000 ) ) ;
#3216 = DIRECTION ( 'NONE',  ( 0.000000000000000000, 9.408669700213191589E-16, -1.000000000000000000 ) ) ;
#3217 = EDGE_CURVE ( 'NONE', #28773, #11934, #1018, .T. ) ;
#3218 = AXIS2_PLACEMENT_3D ( 'NONE', #42628, #39144, #9485 ) ;
#3219 = CARTESIAN_POINT ( 'NONE',  ( 17.99999999999999645, 0.000000000000000000, 0.000000000000000000 ) ) ;
#3220 = DIRECTION ( 'NONE',  ( 1.000000000000000000, 0.000000000000000000, -0.000000000000000000 ) ) ;
#3221 = ORIENTED_EDGE ( 'NONE', *, *, #28772, .T. ) ;
#3222 = CARTESIAN_POINT ( 'NONE',  ( 17.99999999999999645, 110.1579703617969130, -21.29539948940136540 ) ) ;
#3223 = VERTEX_POINT ( 'NONE', #23468 ) ;
#3224 = DIRECTION ( 'NONE',  ( 0.000000000000000000, -0.7525707698561440173, 0.6585113790650322096 ) ) ;
#3225 = LINE ( 'NONE', #33785, #10904 ) ;
#3227 = ORIENTED_EDGE ( 'NONE', *, *, #38286, .T. ) ;
#3226 = AXIS2_PLACEMENT_3D ( 'NONE', #4499, #35044, #4735 ) ;
#3228 = CARTESIAN_POINT ( 'NONE',  ( 17.99999999999999645, 0.000000000000000000, 0.000000000000000000 ) ) ;
#3229 = DIRECTION ( 'NONE',  ( 1.000000000000000000, 0.000000000000000000, 0.000000000000000000 ) ) ;
#3230 = AXIS2_PLACEMENT_3D ( 'NONE', #28717, #38493, #11925 ) ;
#3231 = AXIS2_PLACEMENT_3D ( 'NONE', #12731, #26035, #16224 ) ;
#3232 = DIRECTION ( 'NONE',  ( -1.000000000000000000, 0.000000000000000000, 0.000000000000000000 ) ) ;
#3233 = CARTESIAN_POINT ( 'NONE',  ( 4.090615425948669781, 31.00000000000000355, -62.60416666561555132 ) ) ;
#3234 = ADVANCED_FACE ( 'NONE', ( #6850 ), #20204, .T. ) ;
#3235 = AXIS2_PLACEMENT_3D ( 'NONE', #9171, #42099, #38840 ) ;
#3236 = VERTEX_POINT ( 'NONE', #34767 ) ;
#3238 = CARTESIAN_POINT ( 'NONE',  ( 23.59836588145513048, 31.00000000000000355, -26.81698947917456266 ) ) ;
#3237 = AXIS2_PLACEMENT_3D ( 'NONE', #37023, #7129, #30713 ) ;
#3239 = CARTESIAN_POINT ( 'NONE',  ( -30.22953878324074495, 40.00000000000000000, 61.32923288305941867 ) ) ;
#3240 = AXIS2_PLACEMENT_3D ( 'NONE', #12229, #24926, #42295 ) ;
#3241 = DIRECTION ( 'NONE',  ( 0.000000000000000000, 0.000000000000000000, 1.000000000000000000 ) ) ;
#3242 = CIRCLE ( 'NONE', #8242, 47.49899999999999523 ) ;
#3243 = CARTESIAN_POINT ( 'NONE',  ( 17.99999999999999645, -93.26762629039376407, -76.29967815892449323 ) ) ;
#3244 = DIRECTION ( 'NONE',  ( 0.000000000000000000, 0.000000000000000000, -1.000000000000000000 ) ) ;
#3245 = DIRECTION ( 'NONE',  ( 0.000000000000000000, 0.000000000000000000, -1.000000000000000000 ) ) ;
#3246 = EDGE_CURVE ( 'NONE', #11411, #1814, #14507, .T. ) ;
#3247 = PRODUCT_DEFINITION_SHAPE ( 'NONE', 'NONE',  #43191 ) ;
#3248 = ORIENTED_EDGE ( 'NONE', *, *, #42169, .T. ) ;
#3249 = CARTESIAN_POINT ( 'NONE',  ( -29.60425243605831724, 40.00000000000000000, 38.59963703562669934 ) ) ;
#3250 = DIRECTION ( 'NONE',  ( 0.000000000000000000, 0.000000000000000000, 1.000000000000000000 ) ) ;
#3251 = DIRECTION ( 'NONE',  ( -0.000000000000000000, 0.000000000000000000, -1.000000000000000000 ) ) ;
#3252 = ORIENTED_EDGE ( 'NONE', *, *, #35087, .F. ) ;
#3253 = DIRECTION ( 'NONE',  ( -1.000000000000000000, 0.000000000000000000, 0.000000000000000000 ) ) ;
#3254 = DIRECTION ( 'NONE',  ( 1.000000000000000000, 1.836909530733573776E-16, 0.000000000000000000 ) ) ;
#3255 = ORIENTED_EDGE ( 'NONE', *, *, #35440, .T. ) ;
#3256 = DIRECTION ( 'NONE',  ( 0.000000000000000000, 0.000000000000000000, 1.000000000000000000 ) ) ;
#3257 = ORIENTED_EDGE ( 'NONE', *, *, #20791, .F. ) ;
#3258 = AXIS2_PLACEMENT_3D ( 'NONE', #36683, #6809, #23424 ) ;
#3259 = EDGE_CURVE ( 'NONE', #26405, #39386, #36552, .T. ) ;
#3260 = CIRCLE ( 'NONE', #40212, 12.50000000000000000 ) ;
#3261 = EDGE_LOOP ( 'NONE', ( #474, #40185, #26790, #9231 ) ) ;
#3262 = VECTOR ( 'NONE', #4727, 1000.000000000000000 ) ;
#3263 = CARTESIAN_POINT ( 'NONE',  ( -105.9879088449591933, 40.00000000000000000, -2.880719929157669945 ) ) ;
#3264 = AXIS2_PLACEMENT_3D ( 'NONE', #13667, #24140, #3577 ) ;
#3265 = B_SPLINE_CURVE_WITH_KNOTS ( 'NONE', 3,
 ( #18482, #14547, #1848, #17829, #31536, #31104, #34801, #15210 ),
 .UNSPECIFIED., .F., .F.,
 ( 4, 2, 2, 4 ),
 ( 0.005725059856848641743, 0.006314084072593626612, 0.006903108288338611481, 0.008081156719828581220 ),
 .UNSPECIFIED. ) ;
#3266 = CARTESIAN_POINT ( 'NONE',  ( -46.83686391397709770, 31.00000000000000355, -81.34213072392142863 ) ) ;
#3267 = ORIENTED_EDGE ( 'NONE', *, *, #28812, .F. ) ;
#3268 = CARTESIAN_POINT ( 'NONE',  ( 17.99999999999999645, 75.03166794516924654, -94.29071961951432002 ) ) ;
#3269 = VECTOR ( 'NONE', #19363, 1000.000000000000000 ) ;
#3270 = LINE ( 'NONE', #16648, #20612 ) ;
#3271 = EDGE_CURVE ( 'NONE', #1962, #5566, #4874, .T. ) ;
#3272 = CARTESIAN_POINT ( 'NONE',  ( 5.991980000000000750, 0.000000000000000000, 0.000000000000000000 ) ) ;
#3273 = ORIENTED_EDGE ( 'NONE', *, *, #40965, .F. ) ;
#3274 = CARTESIAN_POINT ( 'NONE',  ( 0.000000000000000000, 0.000000000000000000, 0.000000000000000000 ) ) ;
#3275 = AXIS2_PLACEMENT_3D ( 'NONE', #14499, #27811, #4643 ) ;
#3276 = CARTESIAN_POINT ( 'NONE',  ( 126.0000000000000284, 1.589209405437102375E-14, -20.00000000000001776 ) ) ;
#3278 = DIRECTION ( 'NONE',  ( -1.000000000000000000, 0.000000000000000000, -0.000000000000000000 ) ) ;
#3277 = DIRECTION ( 'NONE',  ( -1.000000000000000000, 0.000000000000000000, -0.000000000000000000 ) ) ;
#3279 = CARTESIAN_POINT ( 'NONE',  ( 17.99999999999999645, -21.56073507908629594, -23.57770962728587705 ) ) ;
#3280 = EDGE_LOOP ( 'NONE', ( #4077, #12239, #21262, #32611 ) ) ;
#3281 = CARTESIAN_POINT ( 'NONE',  ( -29.59829689555773058, 31.00000000000000355, 3.906358533625565954 ) ) ;
#3282 = EDGE_CURVE ( 'NONE', #28903, #844, #15676, .T. ) ;
#3283 = ORIENTED_EDGE ( 'NONE', *, *, #33246, .F. ) ;
#3284 = LINE ( 'NONE', #1537, #32337 ) ;
#3285 = EDGE_CURVE ( 'NONE', #41485, #38794, #40001, .T. ) ;
#3286 = AXIS2_PLACEMENT_3D ( 'NONE', #23435, #16453, #43031 ) ;
#3287 = ORIENTED_EDGE ( 'NONE', *, *, #27542, .F. ) ;
#3288 = DIRECTION ( 'NONE',  ( 0.000000000000000000, 0.000000000000000000, 1.000000000000000000 ) ) ;
#3289 = CARTESIAN_POINT ( 'NONE',  ( 33.47591237148697729, 40.00000000000000000, -8.973542178613062248 ) ) ;
#3290 = AXIS2_PLACEMENT_3D ( 'NONE', #14630, #27488, #30761 ) ;
#3291 = CARTESIAN_POINT ( 'NONE',  ( -52.09564885855072447, 40.00000000000000000, -3.498939618562995513 ) ) ;
#3292 = AXIS2_PLACEMENT_3D ( 'NONE', #38380, #35105, #1942 ) ;
#3293 = CIRCLE ( 'NONE', #10303, 59.00000000000000000 ) ;
#3294 = VECTOR ( 'NONE', #28045, 1000.000000000000000 ) ;
#3295 = ORIENTED_EDGE ( 'NONE', *, *, #42552, .T. ) ;
#3296 = ORIENTED_EDGE ( 'NONE', *, *, #6501, .F. ) ;
#3297 = DIRECTION ( 'NONE',  ( 0.000000000000000000, 0.000000000000000000, -1.000000000000000000 ) ) ;
#3298 = CYLINDRICAL_SURFACE ( 'NONE', #19370, 59.00000000000000000 ) ;
#3299 = CIRCLE ( 'NONE', #4699, 11.00000000000023448 ) ;
#3300 = CARTESIAN_POINT ( 'NONE',  ( 0.000000000000000000, 0.000000000000000000, 0.000000000000000000 ) ) ;
#3301 = DIRECTION ( 'NONE',  ( -1.000000000000000000, -0.000000000000000000, -0.000000000000000000 ) ) ;
#3302 = CARTESIAN_POINT ( 'NONE',  ( 17.99999999999999645, 0.000000000000000000, 0.000000000000000000 ) ) ;
#3303 = ORIENTED_EDGE ( 'NONE', *, *, #8562, .T. ) ;
#3304 = FACE_OUTER_BOUND ( 'NONE', #5848, .T. ) ;
#3305 = EDGE_LOOP ( 'NONE', ( #11083, #15228, #7574, #14144 ) ) ;
#3306 = CARTESIAN_POINT ( 'NONE',  ( -10.00000000000000000, 0.000000000000000000, 0.000000000000000000 ) ) ;
#3307 = CARTESIAN_POINT ( 'NONE',  ( 17.99999999999999645, 26.29521155129873833, -17.34211205339320117 ) ) ;
#3308 = APPLICATION_CONTEXT ( 'automotive_design' ) ;
#3309 = AXIS2_PLACEMENT_3D ( 'NONE', #11976, #18330, #18122 ) ;
#3310 = VERTEX_POINT ( 'NONE', #2014 ) ;
#3311 = DIRECTION ( 'NONE',  ( 0.000000000000000000, 0.000000000000000000, 1.000000000000000000 ) ) ;
#3312 = DIRECTION ( 'NONE',  ( 0.000000000000000000, -0.9213119778704165208, 0.3888241754733123834 ) ) ;
#3313 = ORIENTED_EDGE ( 'NONE', *, *, #25017, .T. ) ;
#3314 = DIRECTION ( 'NONE',  ( 0.000000000000000000, 0.000000000000000000, 1.000000000000000000 ) ) ;
#3315 = ORIENTED_EDGE ( 'NONE', *, *, #30009, .F. ) ;
#3316 = DIRECTION ( 'NONE',  ( 0.000000000000000000, 0.000000000000000000, 1.000000000000000000 ) ) ;
#3317 = EDGE_CURVE ( 'NONE', #2232, #40785, #4511, .T. ) ;
#3318 = ORIENTED_EDGE ( 'NONE', *, *, #18428, .T. ) ;
#3320 = VERTEX_POINT ( 'NONE', #1588 ) ;
#3319 = DIRECTION ( 'NONE',  ( 3.009274222672345096E-17, 1.000000000000000000, -2.455023325076455345E-18 ) ) ;
#3321 = CARTESIAN_POINT ( 'NONE',  ( -61.79211991636739754, 31.00000000000000711, -8.240724169199884486 ) ) ;
#3322 = EDGE_CURVE ( 'NONE', #291, #30171, #8788, .T. ) ;
#3323 = ORIENTED_EDGE ( 'NONE', *, *, #21761, .F. ) ;
#3324 = DIRECTION ( 'NONE',  ( 0.2604563316218754254, 5.114700905345146860E-16, 0.9654856287475623855 ) ) ;
#3325 = AXIS2_PLACEMENT_3D ( 'NONE', #28846, #12269, #28437 ) ;
#3326 = EDGE_CURVE ( 'NONE', #25336, #12545, #35405, .T. ) ;
#3327 = AXIS2_PLACEMENT_3D ( 'NONE', #21633, #1929, #15290 ) ;
#3328 = ORIENTED_EDGE ( 'NONE', *, *, #31058, .T. ) ;
#3329 = AXIS2_PLACEMENT_3D ( 'NONE', #11939, #28527, #38091 ) ;
#3330 = DIRECTION ( 'NONE',  ( -1.000000000000000000, -0.000000000000000000, -0.000000000000000000 ) ) ;
#3331 = VERTEX_POINT ( 'NONE', #31935 ) ;
#3332 = AXIS2_PLACEMENT_3D ( 'NONE', #9001, #22142, #31927 ) ;
#3333 = CARTESIAN_POINT ( 'NONE',  ( 11.20008397363331198, 40.00000000000000000, -84.14439686172906363 ) ) ;
#3334 = AXIS2_PLACEMENT_3D ( 'NONE', #3087, #22807, #26692 ) ;
#3335 = CIRCLE ( 'NONE', #8230, 116.0000000000000000 ) ;
#3337 = CARTESIAN_POINT ( 'NONE',  ( 4.999999999999997335, 0.000000000000000000, 0.000000000000000000 ) ) ;
#3336 = DIRECTION ( 'NONE',  ( 0.000000000000000000, 0.6736956436465584286, -0.7390089172206579793 ) ) ;
#3338 = CARTESIAN_POINT ( 'NONE',  ( 8.999999999999998224, -94.52951811191512377, -67.23221107124996365 ) ) ;
#3339 = ORIENTED_EDGE ( 'NONE', *, *, #32072, .F. ) ;
#3340 = CARTESIAN_POINT ( 'NONE',  ( 17.99999999999999645, 27.24480646643607074, 15.80846360676594564 ) ) ;
#3341 = ORIENTED_EDGE ( 'NONE', *, *, #3008, .T. ) ;
#3342 = FILL_AREA_STYLE ('',( #15222 ) ) ;
#3343 = DIRECTION ( 'NONE',  ( -1.000000000000000000, 0.000000000000000000, -0.000000000000000000 ) ) ;
#3344 = EDGE_CURVE ( 'NONE', #1751, #29967, #21275, .T. ) ;
#3345 = CARTESIAN_POINT ( 'NONE',  ( -26.42126989340051324, 31.00000000000000355, -77.78956226056263290 ) ) ;
#3346 = EDGE_CURVE ( 'NONE', #24569, #21049, #5887, .T. ) ;
#3348 = DIRECTION ( 'NONE',  ( 1.000000000000000000, 0.000000000000000000, 0.000000000000000000 ) ) ;
#3347 = CARTESIAN_POINT ( 'NONE',  ( -10.00000000000000000, 0.000000000000000000, 0.000000000000000000 ) ) ;
#3349 = ORIENTED_EDGE ( 'NONE', *, *, #5609, .T. ) ;
#3350 = ADVANCED_FACE ( 'NONE', ( #41290 ), #31067, .F. ) ;
#3351 = EDGE_CURVE ( 'NONE', #13484, #36189, #21307, .T. ) ;
#3352 = EDGE_CURVE ( 'NONE', #14329, #18075, #37967, .T. ) ;
#3353 = CARTESIAN_POINT ( 'NONE',  ( -22.00000000000000711, 40.00000000000000000, 0.000000000000000000 ) ) ;
#3354 = EDGE_LOOP ( 'NONE', ( #2825, #40400, #8127, #15878 ) ) ;
#3355 = DIRECTION ( 'NONE',  ( 0.000000000000000000, 0.8477344278896686847, 0.5304209081197459597 ) ) ;
#3356 = DIRECTION ( 'NONE',  ( 0.000000000000000000, 0.8747630845319590565, 0.4845508703326540934 ) ) ;
#3357 = AXIS2_PLACEMENT_3D ( 'NONE', #30775, #30570, #27732 ) ;
#3358 = CARTESIAN_POINT ( 'NONE',  ( -91.07534658258107640, 31.00000000000000711, 44.76935032132903558 ) ) ;
#3359 = CARTESIAN_POINT ( 'NONE',  ( 0.000000000000000000, -36.34385289850569478, -29.77717097092114429 ) ) ;
#3360 = CIRCLE ( 'NONE', #40302, 20.00000000000000711 ) ;
#3361 = ORIENTED_EDGE ( 'NONE', *, *, #28288, .F. ) ;
#3362 = DIRECTION ( 'NONE',  ( -1.000000000000000000, 0.000000000000000000, 0.000000000000000000 ) ) ;
#3363 = EDGE_LOOP ( 'NONE', ( #11749, #25000 ) ) ;
#3364 = DIRECTION ( 'NONE',  ( 1.000000000000000000, -0.000000000000000000, -0.000000000000000000 ) ) ;
#3365 = CARTESIAN_POINT ( 'NONE',  ( 17.99999999999999645, 97.97378550988226209, 62.10585602713792497 ) ) ;
#3366 = CARTESIAN_POINT ( 'NONE',  ( 17.99999999999999645, -31.81777574834303124, 10.70123563439434733 ) ) ;
#3367 = EDGE_LOOP ( 'NONE', ( #15088, #41066, #31064, #1389 ) ) ;
#3368 = ORIENTED_EDGE ( 'NONE', *, *, #14557, .F. ) ;
#3369 = DIRECTION ( 'NONE',  ( 0.000000000000000000, 0.000000000000000000, 1.000000000000000000 ) ) ;
#3370 = CARTESIAN_POINT ( 'NONE',  ( 0.000000000000000000, -115.6826031496112677, 8.575274253897077870 ) ) ;
#3371 = EDGE_CURVE ( 'NONE', #10707, #17317, #8013, .T. ) ;
#3372 = FACE_OUTER_BOUND ( 'NONE', #28907, .T. ) ;
#3374 = ORIENTED_EDGE ( 'NONE', *, *, #38041, .F. ) ;
#3373 = CYLINDRICAL_SURFACE ( 'NONE', #11096, 20.00000000000000355 ) ;
#3375 = CARTESIAN_POINT ( 'NONE',  ( -1.974796425974089331, 31.00000000000000355, 29.60085432090884439 ) ) ;
#3376 = EDGE_CURVE ( 'NONE', #40002, #17054, #320, .T. ) ;
#3377 = DIRECTION ( 'NONE',  ( 0.000000000000000000, 0.000000000000000000, -1.000000000000000000 ) ) ;
#3379 = ORIENTED_EDGE ( 'NONE', *, *, #31376, .T. ) ;
#3378 = FACE_OUTER_BOUND ( 'NONE', #6020, .T. ) ;
#3380 = ORIENTED_EDGE ( 'NONE', *, *, #1979, .F. ) ;
#3381 = CARTESIAN_POINT ( 'NONE',  ( 17.99999999999999645, -108.8684555192048435, 27.12806418649580564 ) ) ;
#3382 = DIRECTION ( 'NONE',  ( -1.000000000000000000, -0.000000000000000000, -0.000000000000000000 ) ) ;
#3383 = CARTESIAN_POINT ( 'NONE',  ( 12.64472494877221997, 40.00000000000000000, 47.53373494968590762 ) ) ;
#3384 = CARTESIAN_POINT ( 'NONE',  ( 17.99999999999999645, 40.13512380273970592, 113.6206972269522737 ) ) ;
#3385 = AXIS2_PLACEMENT_3D ( 'NONE', #3579, #83, #747 ) ;
#3386 = CIRCLE ( 'NONE', #38964, 20.00000000000000355 ) ;
#3387 = CYLINDRICAL_SURFACE ( 'NONE', #34669, 59.00000000000000000 ) ;
#3388 = CARTESIAN_POINT ( 'NONE',  ( 150.0000507999999968, 0.000000000000000000, 0.000000000000000000 ) ) ;
#3389 = ORIENTED_EDGE ( 'NONE', *, *, #33819, .F. ) ;
#3390 = AXIS2_PLACEMENT_3D ( 'NONE', #15975, #32107, #19470 ) ;
#3391 = CARTESIAN_POINT ( 'NONE',  ( 17.99999999999999645, 0.000000000000000000, 0.000000000000000000 ) ) ;
#3392 = ORIENTED_EDGE ( 'NONE', *, *, #27091, .T. ) ;
#3393 = CARTESIAN_POINT ( 'NONE',  ( 0.000000000000000000, 0.000000000000000000, 0.000000000000000000 ) ) ;
#3394 = CARTESIAN_POINT ( 'NONE',  ( 0.000000000000000000, -16.86122981692037825, 27.13802899033285954 ) ) ;
#3395 = CARTESIAN_POINT ( 'NONE',  ( -48.80550277073417931, 31.00000000000000355, -13.06547612810710035 ) ) ;
#3396 = EDGE_CURVE ( 'NONE', #12907, #10944, #26834, .T. ) ;
#3397 = DIRECTION ( 'NONE',  ( -1.000000000000000000, -0.000000000000000000, -0.000000000000000000 ) ) ;
#3398 = ORIENTED_EDGE ( 'NONE', *, *, #21737, .F. ) ;
#3399 = ADVANCED_FACE ( 'NONE', ( #22147 ), #5520, .T. ) ;
#3400 = EDGE_CURVE ( 'NONE', #18706, #36637, #1154, .T. ) ;
#3401 = EDGE_CURVE ( 'NONE', #8016, #22923, #4651, .T. ) ;
#3402 = DIRECTION ( 'NONE',  ( -1.000000000000000000, -0.000000000000000000, -0.000000000000000000 ) ) ;
#3403 = VERTEX_POINT ( 'NONE', #29731 ) ;
#3404 = CARTESIAN_POINT ( 'NONE',  ( 48.45023387855729879, 31.00000000000000355, 83.88660019351674180 ) ) ;
#3405 = ORIENTED_EDGE ( 'NONE', *, *, #38798, .T. ) ;
#3406 = DIRECTION ( 'NONE',  ( 0.000000000000000000, 0.000000000000000000, -1.000000000000000000 ) ) ;
#3407 = CARTESIAN_POINT ( 'NONE',  ( 67.48878131082855703, 31.00000000000000000, 39.09986611101695786 ) ) ;
#3408 = CARTESIAN_POINT ( 'NONE',  ( -35.65230965300054322, 40.00000000000000000, 72.05959145982365044 ) ) ;
#3409 = EDGE_CURVE ( 'NONE', #38711, #28617, #26241, .T. ) ;
#3410 = DIRECTION ( 'NONE',  ( 1.000000000000000000, 0.000000000000000000, -6.546126324440850663E-16 ) ) ;
#3411 = EDGE_LOOP ( 'NONE', ( #37180, #20080, #41185, #14364 ) ) ;
#3412 = ORIENTED_EDGE ( 'NONE', *, *, #5313, .F. ) ;
#3413 = CARTESIAN_POINT ( 'NONE',  ( 0.000000000000000000, 29.09613215194482549, 21.19941258140333673 ) ) ;
#3414 = ADVANCED_FACE ( 'NONE', ( #32975 ), #15577, .F. ) ;
#3415 = CARTESIAN_POINT ( 'NONE',  ( 17.99999999999999645, 0.000000000000000000, 0.000000000000000000 ) ) ;
#3416 = CARTESIAN_POINT ( 'NONE',  ( 0.000000000000000000, -26.29521155129861398, 17.34211205339337880 ) ) ;
#3417 = AXIS2_PLACEMENT_3D ( 'NONE', #7248, #39965, #30186 ) ;
#3418 = CIRCLE ( 'NONE', #13214, 36.00000000000000000 ) ;
#3420 = EDGE_LOOP ( 'NONE', ( #6082, #14662, #24472, #30443 ) ) ;
#3419 = CARTESIAN_POINT ( 'NONE',  ( -26.14979319748359643, 5.944745455504278020, 2.972870684497277427 ) ) ;
#3421 = CARTESIAN_POINT ( 'NONE',  ( 0.000000000000000000, 0.000000000000000000, 0.000000000000000000 ) ) ;
#3422 = ORIENTED_EDGE ( 'NONE', *, *, #3879, .T. ) ;
#3423 = DIRECTION ( 'NONE',  ( 0.000000000000000000, 0.000000000000000000, 1.000000000000000000 ) ) ;
#3424 = AXIS2_PLACEMENT_3D ( 'NONE', #17051, #23172, #13551 ) ;
#3425 = CARTESIAN_POINT ( 'NONE',  ( -44.26264085331523290, 40.00000000000000711, 76.66224561666088277 ) ) ;
#3426 = CARTESIAN_POINT ( 'NONE',  ( 9.000000000000001776, -49.65209126885773827, 15.44894276735532834 ) ) ;
#3427 = ORIENTED_EDGE ( 'NONE', *, *, #31055, .T. ) ;
#3428 = DIRECTION ( 'NONE',  ( -1.000000000000000000, 0.000000000000000000, 0.000000000000000000 ) ) ;
#3429 = FACE_OUTER_BOUND ( 'NONE', #4282, .T. ) ;
#3430 = VERTEX_POINT ( 'NONE', #39512 ) ;
#3431 = EDGE_CURVE ( 'NONE', #9950, #42699, #11557, .T. ) ;
#3432 = ORIENTED_EDGE ( 'NONE', *, *, #42431, .T. ) ;
#3433 = CARTESIAN_POINT ( 'NONE',  ( 3.983177536951266529, -13.66651769228263191, -1.199999999999999956 ) ) ;
#3434 = ORIENTED_EDGE ( 'NONE', *, *, #3548, .T. ) ;
#3435 = DIRECTION ( 'NONE',  ( -1.000000000000000000, -0.000000000000000000, -0.000000000000000000 ) ) ;
#3436 = DIRECTION ( 'NONE',  ( -1.000000000000000000, -0.000000000000000000, 0.000000000000000000 ) ) ;
#3437 = CARTESIAN_POINT ( 'NONE',  ( 17.99999999999999645, 29.09613215194512748, -21.19941258140292462 ) ) ;
#3438 = DIRECTION ( 'NONE',  ( 0.000000000000000000, -0.1062934856473523731, -0.9943348002101385363 ) ) ;
#3439 = DIRECTION ( 'NONE',  ( -1.000000000000000000, -0.000000000000000000, -0.000000000000000000 ) ) ;
#3440 = VERTEX_POINT ( 'NONE', #29093 ) ;
#3441 = CARTESIAN_POINT ( 'NONE',  ( -8.920000000000003482, 0.000000000000000000, 0.000000000000000000 ) ) ;
#3442 = ORIENTED_EDGE ( 'NONE', *, *, #42111, .F. ) ;
#3443 = AXIS2_PLACEMENT_3D ( 'NONE', #2942, #10158, #19591 ) ;
#3444 =( NAMED_UNIT ( * ) SI_UNIT ( $, .STERADIAN. ) SOLID_ANGLE_UNIT ( ) );
#3445 = DIRECTION ( 'NONE',  ( 0.000000000000000000, 0.000000000000000000, 1.000000000000000000 ) ) ;
#3446 = AXIS2_PLACEMENT_3D ( 'NONE', #33041, #16278, #25692 ) ;
#3448 = CYLINDRICAL_SURFACE ( 'NONE', #35268, 120.5010000000000190 ) ;
#3447 = VECTOR ( 'NONE', #13140, 1000.000000000000000 ) ;
#3449 = VERTEX_POINT ( 'NONE', #9422 ) ;
#3450 = DIRECTION ( 'NONE',  ( 0.000000000000000000, 0.000000000000000000, -1.000000000000000000 ) ) ;
#3451 = EDGE_CURVE ( 'NONE', #29515, #32794, #15034, .T. ) ;
#3452 = CARTESIAN_POINT ( 'NONE',  ( 17.99999999999999645, 109.1131968883995000, 26.12628443612074847 ) ) ;
#3453 = ITEM_DEFINED_TRANSFORMATION ( 'NONE', 'NONE', #29548,  #13552 ) ;
#3454 = CARTESIAN_POINT ( 'NONE',  ( 17.99999999999999645, -21.48775762007876367, 23.64423737150130478 ) ) ;
#3455 = CARTESIAN_POINT ( 'NONE',  ( 64.78932475141161262, 31.00000000000000000, 8.528958657501300777 ) ) ;
#3456 = ORIENTED_EDGE ( 'NONE', *, *, #4256, .T. ) ;
#3457 = CARTESIAN_POINT ( 'NONE',  ( -30.58448433907586761, 31.00000000000000355, 8.146263651248247584 ) ) ;
#3458 = CARTESIAN_POINT ( 'NONE',  ( 75.10416666583130052, 39.99999999999999289, 4.908738512847474311 ) ) ;
#3459 = ADVANCED_FACE ( 'NONE', ( #5721 ), #35603, .F. ) ;
#3460 = DIRECTION ( 'NONE',  ( -1.000000000000000000, -0.000000000000000000, -0.000000000000000000 ) ) ;
#3461 = EDGE_CURVE ( 'NONE', #12095, #30629, #19918, .T. ) ;
#3462 = FACE_OUTER_BOUND ( 'NONE', #12214, .T. ) ;
#3463 = VERTEX_POINT ( 'NONE', #12514 ) ;
#3464 = PLANE ( 'NONE',  #37863 ) ;
#3465 = CARTESIAN_POINT ( 'NONE',  ( 17.99999999999999645, 116.4607004671432406, -30.94182036827089632 ) ) ;
#3466 = ORIENTED_EDGE ( 'NONE', *, *, #6025, .F. ) ;
#3467 = CARTESIAN_POINT ( 'NONE',  ( -18.68892229297488683, 40.00000000000000000, 55.06009237583231197 ) ) ;
#3468 = DIRECTION ( 'NONE',  ( 1.000000000000000000, 0.000000000000000000, 0.000000000000000000 ) ) ;
#3470 = CARTESIAN_POINT ( 'NONE',  ( 0.000000000000000000, 0.000000000000000000, 0.000000000000000000 ) ) ;
#3469 = VECTOR ( 'NONE', #12213, 1000.000000000000000 ) ;
#3471 = AXIS2_PLACEMENT_3D ( 'NONE', #7304, #20895, #16746 ) ;
#3472 = VERTEX_POINT ( 'NONE', #25827 ) ;
#3473 = DIRECTION ( 'NONE',  ( 0.000000000000000000, 0.5963673585384969833, 0.8027116379309670036 ) ) ;
#3474 = DIRECTION ( 'NONE',  ( 1.000000000000000000, -1.373900992973641868E-15, -4.017254365419995317E-16 ) ) ;
#3475 = VECTOR ( 'NONE', #5005, 1000.000000000000000 ) ;
#3476 = EDGE_LOOP ( 'NONE', ( #18282, #15572, #12571, #5791 ) ) ;
#3477 = CARTESIAN_POINT ( 'NONE',  ( -6.600000000000004974, 19.59999999999999787, 0.000000000000000000 ) ) ;
#3478 = EDGE_LOOP ( 'NONE', ( #7369, #39543, #10566, #17396 ) ) ;
#3479 = VERTEX_POINT ( 'NONE', #42142 ) ;
#3480 = CARTESIAN_POINT ( 'NONE',  ( 0.000000000000000000, 7.220349212960450735, 35.26849241522667455 ) ) ;
#3481 = CARTESIAN_POINT ( 'NONE',  ( 84.84057271803867195, 31.00000000000000000, 49.13019966417499518 ) ) ;
#3482 = ORIENTED_EDGE ( 'NONE', *, *, #2076, .F. ) ;
#3483 = CARTESIAN_POINT ( 'NONE',  ( 17.99999999999999645, 0.000000000000000000, 0.000000000000000000 ) ) ;
#3484 = DIRECTION ( 'NONE',  ( -1.000000000000000000, -0.000000000000000000, -0.000000000000000000 ) ) ;
#3485 = CARTESIAN_POINT ( 'NONE',  ( 0.000000000000000000, 0.000000000000000000, 0.000000000000000000 ) ) ;
#3486 = ORIENTED_EDGE ( 'NONE', *, *, #29791, .F. ) ;
#3487 = DIRECTION ( 'NONE',  ( -3.009274222672345096E-17, -1.000000000000000000, 2.455023325076454960E-18 ) ) ;
#3488 = FACE_OUTER_BOUND ( 'NONE', #19442, .T. ) ;
#3489 = CIRCLE ( 'NONE', #18214, 0.7500000000000006661 ) ;
#3491 = LINE ( 'NONE', #21402, #7303 ) ;
#3490 = CARTESIAN_POINT ( 'NONE',  ( 17.99999999999999645, -18.42432724429453472, -30.92804820216021255 ) ) ;
#3492 = ADVANCED_FACE ( 'NONE', ( #38888 ), #2218, .T. ) ;
#3493 = AXIS2_PLACEMENT_3D ( 'NONE', #25301, #31177, #14386 ) ;
#3494 = DIRECTION ( 'NONE',  ( 0.000000000000000000, 0.000000000000000000, 1.000000000000000000 ) ) ;
#3495 = VERTEX_POINT ( 'NONE', #9852 ) ;
#3496 = FILL_AREA_STYLE ('',( #23408 ) ) ;
#3497 = CARTESIAN_POINT ( 'NONE',  ( 33.70925502316616473, 31.00000000000000355, 11.43906998022225707 ) ) ;
#3498 = CIRCLE ( 'NONE', #33483, 2.500000000000002665 ) ;
#3499 = ORIENTED_EDGE ( 'NONE', *, *, #35905, .F. ) ;
#3500 = LINE ( 'NONE', #37329, #22695 ) ;
#3501 = CIRCLE ( 'NONE', #32125, 120.5010000000000332 ) ;
#3502 = CARTESIAN_POINT ( 'NONE',  ( 18.00000000000000355, 24.72041153920732981, 40.55929306992697292 ) ) ;
#3503 = VERTEX_POINT ( 'NONE', #43002 ) ;
#3504 = AXIS2_PLACEMENT_3D ( 'NONE', #10199, #13722, #40503 ) ;
#3505 = DIRECTION ( 'NONE',  ( 0.000000000000000000, 0.000000000000000000, -1.000000000000000000 ) ) ;
#3506 = CARTESIAN_POINT ( 'NONE',  ( 9.621748599878955588, 40.00000000000000000, 35.89595399306684698 ) ) ;
#3507 = CARTESIAN_POINT ( 'NONE',  ( 22.78600399168703916, 40.00000000000000000, -39.30137845373389638 ) ) ;
#3508 = EDGE_CURVE ( 'NONE', #41968, #27228, #31730, .T. ) ;
#3509 = ORIENTED_EDGE ( 'NONE', *, *, #16971, .F. ) ;
#3510 = LINE ( 'NONE', #224, #38080 ) ;
#3511 = ADVANCED_FACE ( 'NONE', ( #29302 ), #12300, .F. ) ;
#3512 = DIRECTION ( 'NONE',  ( 0.000000000000000000, 1.246648735278247733E-14, -1.000000000000000000 ) ) ;
#3513 = CARTESIAN_POINT ( 'NONE',  ( -10.00000000000000000, 0.000000000000000000, 0.000000000000000000 ) ) ;
#3514 = VERTEX_POINT ( 'NONE', #32341 ) ;
#3515 = DIRECTION ( 'NONE',  ( 0.000000000000000000, -0.5076658003388467844, 0.8615540813938020737 ) ) ;
#3516 = VERTEX_POINT ( 'NONE', #26452 ) ;
#3517 = CARTESIAN_POINT ( 'NONE',  ( 9.999999999999998224, 0.000000000000000000, 0.000000000000000000 ) ) ;
#3518 = CARTESIAN_POINT ( 'NONE',  ( 2.000000000000008882, 3.464101615137749945, 0.000000000000000000 ) ) ;
#3519 = ORIENTED_EDGE ( 'NONE', *, *, #40732, .F. ) ;
#3520 = DIRECTION ( 'NONE',  ( -1.000000000000000000, 0.000000000000000000, -0.000000000000000000 ) ) ;
#3521 = CARTESIAN_POINT ( 'NONE',  ( 17.99999999999999645, 88.00363688980654331, -82.31555682352568226 ) ) ;
#3522 = ORIENTED_EDGE ( 'NONE', *, *, #28811, .F. ) ;
#3523 = CARTESIAN_POINT ( 'NONE',  ( 17.99999999999999645, -79.94368240339484544, 90.16373242487880191 ) ) ;
#3524 = ORIENTED_EDGE ( 'NONE', *, *, #40908, .T. ) ;
#3525 = AXIS2_PLACEMENT_3D ( 'NONE', #15837, #12560, #28719 ) ;
#3526 = DIRECTION ( 'NONE',  ( 1.000000000000000000, 0.000000000000000000, 0.000000000000000000 ) ) ;
#3528 = EDGE_CURVE ( 'NONE', #18244, #43150, #35203, .T. ) ;
#3527 = CIRCLE ( 'NONE', #27271, 58.99999999999999289 ) ;
#3529 = ORIENTED_EDGE ( 'NONE', *, *, #39408, .F. ) ;
#3531 = ORIENTED_EDGE ( 'NONE', *, *, #22081, .F. ) ;
#3530 = LINE ( 'NONE', #23669, #14622 ) ;
#3532 = AXIS2_PLACEMENT_3D ( 'NONE', #27090, #40357, #10491 ) ;
#3533 = CARTESIAN_POINT ( 'NONE',  ( 16.92944795086299337, 31.00000000000000355, -62.81076020704204410 ) ) ;
#3535 = ADVANCED_FACE ( 'NONE', ( #23202 ), #16004, .F. ) ;
#3534 = ORIENTED_EDGE ( 'NONE', *, *, #2146, .F. ) ;
#3536 = CARTESIAN_POINT ( 'NONE',  ( 17.99999999999999645, -31.11570115861498920, 4.898994019976531611 ) ) ;
#3537 = CIRCLE ( 'NONE', #16138, 12.59999999999999964 ) ;
#3538 = ORIENTED_EDGE ( 'NONE', *, *, #6523, .T. ) ;
#3539 = DIRECTION ( 'NONE',  ( -3.996523416598930318E-16, 2.658563593772947863E-15, 1.000000000000000000 ) ) ;
#3540 = ORIENTED_EDGE ( 'NONE', *, *, #22669, .T. ) ;
#3541 = CARTESIAN_POINT ( 'NONE',  ( -49.21613380539481142, 40.00000000000000000, 63.96793098899348706 ) ) ;
#3542 = AXIS2_PLACEMENT_3D ( 'NONE', #18125, #30739, #31176 ) ;
#3544 = CARTESIAN_POINT ( 'NONE',  ( 17.99999999999999645, -47.31079789947416003, -105.9135893174955783 ) ) ;
#3543 = DIRECTION ( 'NONE',  ( -1.000000000000000000, 0.000000000000000000, 0.000000000000000000 ) ) ;
#3545 = DIRECTION ( 'NONE',  ( 0.000000000000000000, 0.000000000000000000, 1.000000000000000000 ) ) ;
#3546 = ORIENTED_EDGE ( 'NONE', *, *, #10588, .T. ) ;
#3547 = CARTESIAN_POINT ( 'NONE',  ( 0.000000000000000000, -111.9370513079666409, -44.61600100275288838 ) ) ;
#3548 = EDGE_CURVE ( 'NONE', #36864, #31070, #34513, .T. ) ;
#3549 = VERTEX_POINT ( 'NONE', #2852 ) ;
#3550 = ORIENTED_EDGE ( 'NONE', *, *, #10461, .T. ) ;
#3551 = DIRECTION ( 'NONE',  ( 0.000000000000000000, 0.000000000000000000, 1.000000000000000000 ) ) ;
#3552 = CARTESIAN_POINT ( 'NONE',  ( -71.24862878704732339, 31.00000000000000711, 35.13526414049667324 ) ) ;
#3553 = CARTESIAN_POINT ( 'NONE',  ( 3.540020015735602765, 2.810662092924382627, -3.602146406945867962 ) ) ;
#3554 = ORIENTED_EDGE ( 'NONE', *, *, #18854, .F. ) ;
#3555 = EDGE_CURVE ( 'NONE', #17655, #26722, #40066, .T. ) ;
#3556 = DIRECTION ( 'NONE',  ( 0.000000000000000000, 0.000000000000000000, 1.000000000000000000 ) ) ;
#3557 = ADVANCED_FACE ( 'NONE', ( #12935 ), #23412, .F. ) ;
#3558 = AXIS2_PLACEMENT_3D ( 'NONE', #32123, #22550, #15774 ) ;
#3559 = APPLICATION_CONTEXT ( 'automotive_design' ) ;
#3560 = ORIENTED_EDGE ( 'NONE', *, *, #22818, .T. ) ;
#3561 = CARTESIAN_POINT ( 'NONE',  ( 17.99999999999999645, -112.5220807139885864, 28.19186676675805003 ) ) ;
#3562 = EDGE_CURVE ( 'NONE', #20877, #28679, #3500, .T. ) ;
#3563 = DIRECTION ( 'NONE',  ( -0.000000000000000000, -0.000000000000000000, 1.000000000000000000 ) ) ;
#3564 = LINE ( 'NONE', #26726, #40049 ) ;
#3565 = AXIS2_PLACEMENT_3D ( 'NONE', #39691, #35796, #3473 ) ;
#3566 = CARTESIAN_POINT ( 'NONE',  ( 8.919999999999998153, 0.000000000000000000, 11.00000000000000000 ) ) ;
#3567 = EDGE_LOOP ( 'NONE', ( #27316, #14935, #34912, #26420 ) ) ;
#3568 = LINE ( 'NONE', #36746, #7466 ) ;
#3569 = VERTEX_POINT ( 'NONE', #20806 ) ;
#3570 = CIRCLE ( 'NONE', #11279, 59.00000000000000000 ) ;
#3571 = DIRECTION ( 'NONE',  ( 0.000000000000000000, 0.000000000000000000, 1.000000000000000000 ) ) ;
#3572 = CYLINDRICAL_SURFACE ( 'NONE', #16556, 13.59999999999999964 ) ;
#3573 = DIRECTION ( 'NONE',  ( -1.000000000000000000, 0.000000000000000000, 0.000000000000000000 ) ) ;
#3574 = VERTEX_POINT ( 'NONE', #6567 ) ;
#3575 = ORIENTED_EDGE ( 'NONE', *, *, #20808, .T. ) ;
#3576 = CARTESIAN_POINT ( 'NONE',  ( 17.99999999999999645, 0.000000000000000000, 0.000000000000000000 ) ) ;
#3577 = DIRECTION ( 'NONE',  ( 1.000000000000000000, -1.373900992973642066E-15, -3.854941057726257326E-16 ) ) ;
#3578 = CARTESIAN_POINT ( 'NONE',  ( 18.00000000000000355, 42.03146605346785947, 22.12489237027331512 ) ) ;
#3580 = EDGE_LOOP ( 'NONE', ( #33920, #37527, #3531, #22237 ) ) ;
#3579 = CARTESIAN_POINT ( 'NONE',  ( 17.99999999999999645, -18.35539002514457252, 110.6858262410709273 ) ) ;
#3581 = CARTESIAN_POINT ( 'NONE',  ( 36.95980244579787666, 31.00000000000000355, 4.931273285801173856 ) ) ;
#3582 = EDGE_CURVE ( 'NONE', #10692, #43124, #6632, .T. ) ;
#3583 = DIRECTION ( 'NONE',  ( 0.000000000000000000, -0.2486898871648415832, -0.9685831611286344067 ) ) ;
#3584 = EDGE_CURVE ( 'NONE', #5508, #13710, #31041, .T. ) ;
#3586 = ORIENTED_EDGE ( 'NONE', *, *, #35904, .T. ) ;
#3585 = CARTESIAN_POINT ( 'NONE',  ( 17.99999999999999645, 114.1529630473454944, -38.59523323561318620 ) ) ;
#3587 = ORIENTED_EDGE ( 'NONE', *, *, #35757, .F. ) ;
#3588 = DIRECTION ( 'NONE',  ( 1.000000000000000000, 0.000000000000000000, 0.000000000000000000 ) ) ;
#3589 = AXIS2_PLACEMENT_3D ( 'NONE', #435, #9839, #13802 ) ;
#3590 = DIRECTION ( 'NONE',  ( 0.000000000000000000, 0.000000000000000000, 1.000000000000000000 ) ) ;
#3591 = CARTESIAN_POINT ( 'NONE',  ( 56.43498182459031653, 40.00000000000000000, -7.339809665447900144 ) ) ;
#3592 = AXIS2_PLACEMENT_3D ( 'NONE', #19386, #42240, #13252 ) ;
#3593 = LINE ( 'NONE', #23936, #4743 ) ;
#3594 = CIRCLE ( 'NONE', #22478, 2.649999999999999467 ) ;
#3595 = DIRECTION ( 'NONE',  ( -1.000000000000000000, 0.000000000000000000, 0.000000000000000000 ) ) ;
#3596 = ORIENTED_EDGE ( 'NONE', *, *, #1485, .T. ) ;
#3597 = DIRECTION ( 'NONE',  ( 1.000000000000000000, 0.000000000000000000, 0.000000000000000000 ) ) ;
#3598 = EDGE_CURVE ( 'NONE', #21981, #214, #36591, .T. ) ;
#3599 = ORIENTED_EDGE ( 'NONE', *, *, #18866, .F. ) ;
#3600 = EDGE_CURVE ( 'NONE', #11582, #42604, #23400, .T. ) ;
#3601 = CIRCLE ( 'NONE', #28048, 51.99999999999999289 ) ;
#3602 = DIRECTION ( 'NONE',  ( -1.000000000000000000, -0.000000000000000000, -0.000000000000000000 ) ) ;
#3603 = CARTESIAN_POINT ( 'NONE',  ( 17.99999999999999645, 120.3696465864706937, -5.624871700594833435 ) ) ;
#3604 = CARTESIAN_POINT ( 'NONE',  ( 20.73284993368543638, 31.00000000000000355, 42.03655757353646294 ) ) ;
#3605 = DIRECTION ( 'NONE',  ( -1.000000000000000000, -0.000000000000000000, 0.000000000000000000 ) ) ;
#3606 = ORIENTED_EDGE ( 'NONE', *, *, #27487, .F. ) ;
#3607 = PRODUCT ( 'socket head cap screw_iso_ISO 4762 M5 x 16 - 16N', 'socket head cap screw_iso_ISO 4762 M5 x 16 - 16N', '', ( #18613 ) ) ;
#3608 = DIRECTION ( 'NONE',  ( 0.000000000000000000, -0.9822872507286903865, 0.1873813145857150808 ) ) ;
#3609 = ORIENTED_EDGE ( 'NONE', *, *, #22877, .T. ) ;
#3610 = EDGE_CURVE ( 'NONE', #39678, #29860, #33844, .T. ) ;
#3611 = CARTESIAN_POINT ( 'NONE',  ( -99.99999999999997158, 31.00000000000000711, 2.428179185498535730E-12 ) ) ;
#3612 = VERTEX_POINT ( 'NONE', #34069 ) ;
#3613 = EDGE_CURVE ( 'NONE', #7922, #13471, #24024, .T. ) ;
#3614 = CYLINDRICAL_SURFACE ( 'NONE', #1093, 116.0000000000000000 ) ;
#3615 = CARTESIAN_POINT ( 'NONE',  ( -9.616483412539254871, 31.00000000000000355, -73.82325415884287168 ) ) ;
#3616 = CARTESIAN_POINT ( 'NONE',  ( -32.59403919554602425, 40.00000000000000000, -66.35267222978370683 ) ) ;
#3617 = DIRECTION ( 'NONE',  ( -1.000000000000000000, 0.000000000000000000, 0.000000000000000000 ) ) ;
#3618 = AXIS2_PLACEMENT_3D ( 'NONE', #39453, #7601, #34008 ) ;
#3619 = ORIENTED_EDGE ( 'NONE', *, *, #41115, .T. ) ;
#3620 = EDGE_LOOP ( 'NONE', ( #39500, #12729, #22297, #202 ) ) ;
#3621 = DIRECTION ( 'NONE',  ( 0.000000000000000000, 0.000000000000000000, 1.000000000000000000 ) ) ;
#3622 = AXIS2_PLACEMENT_3D ( 'NONE', #36254, #23426, #36686 ) ;
#3623 = DIRECTION ( 'NONE',  ( -1.000000000000000000, -0.000000000000000000, 0.000000000000000000 ) ) ;
#3624 = CIRCLE ( 'NONE', #4352, 59.00000000000000000 ) ;
#3626 = ORIENTED_EDGE ( 'NONE', *, *, #4639, .T. ) ;
#3625 = DIRECTION ( 'NONE',  ( 1.000000000000000000, 0.000000000000000000, 0.000000000000000000 ) ) ;
#3627 = CARTESIAN_POINT ( 'NONE',  ( 17.99999999999999645, -11.49545354908957862, 29.80986809967256335 ) ) ;
#3628 = ORIENTED_EDGE ( 'NONE', *, *, #14851, .T. ) ;
#3629 = DIRECTION ( 'NONE',  ( -1.000000000000000000, -0.000000000000000000, -0.000000000000000000 ) ) ;
#3630 = CARTESIAN_POINT ( 'NONE',  ( -84.90650804512098659, 40.00000000000000711, 28.83788733109305014 ) ) ;
#3631 = CARTESIAN_POINT ( 'NONE',  ( 9.000000000000001776, 50.95304419620838843, -10.38206564895608786 ) ) ;
#3632 = AXIS2_PLACEMENT_3D ( 'NONE', #11823, #41015, #11162 ) ;
#3633 = EDGE_LOOP ( 'NONE', ( #11787, #36386, #10623, #35076 ) ) ;
#3634 = ADVANCED_FACE ( 'NONE', ( #29950 ), #24291, .F. ) ;
#3635 = CARTESIAN_POINT ( 'NONE',  ( 8.999999999999998224, 13.57797752207971520, -33.34124362422459598 ) ) ;
#3636 = EDGE_CURVE ( 'NONE', #19286, #12767, #12859, .T. ) ;
#3637 = CYLINDRICAL_SURFACE ( 'NONE', #16929, 120.5010000000000190 ) ;
#3638 = EDGE_CURVE ( 'NONE', #11569, #32279, #21241, .T. ) ;
#3639 = ADVANCED_FACE ( 'NONE', ( #13586 ), #26884, .T. ) ;
#3640 = ORIENTED_EDGE ( 'NONE', *, *, #37174, .T. ) ;
#3641 = CARTESIAN_POINT ( 'NONE',  ( 0.000000000000000000, 0.000000000000000000, 0.000000000000000000 ) ) ;
#3642 = ORIENTED_EDGE ( 'NONE', *, *, #35108, .T. ) ;
#3643 = CARTESIAN_POINT ( 'NONE',  ( 17.99999999999999645, -97.97378550988267421, 62.10585602713726416 ) ) ;
#3644 = ORIENTED_EDGE ( 'NONE', *, *, #36823, .F. ) ;
#3645 = CARTESIAN_POINT ( 'NONE',  ( -22.00000000000000711, 40.00000000000000000, 0.000000000000000000 ) ) ;
#3646 = DIRECTION ( 'NONE',  ( -1.058513553088275437E-16, -1.000000000000000000, 8.813324511995299047E-17 ) ) ;
#3647 = DIRECTION ( 'NONE',  ( 0.000000000000000000, 0.000000000000000000, 1.000000000000000000 ) ) ;
#3648 = DIRECTION ( 'NONE',  ( 0.000000000000000000, 0.000000000000000000, 1.000000000000000000 ) ) ;
#3649 = CARTESIAN_POINT ( 'NONE',  ( 18.00000000000000355, 39.78933988720149273, -24.98727647984960498 ) ) ;
#3650 = ORIENTED_EDGE ( 'NONE', *, *, #18105, .F. ) ;
#3652 = DIRECTION ( 'NONE',  ( 0.000000000000000000, 0.000000000000000000, 1.000000000000000000 ) ) ;
#3651 = CARTESIAN_POINT ( 'NONE',  ( 0.000000000000000000, 32.32520163883584274, 34.09746168776050013 ) ) ;
#3653 = EDGE_LOOP ( 'NONE', ( #27977, #6731, #35715, #37933 ) ) ;
#3654 = AXIS2_PLACEMENT_3D ( 'NONE', #39401, #32032, #2114 ) ;
#3655 = DIRECTION ( 'NONE',  ( 1.000000000000000000, 0.000000000000000000, 0.000000000000000000 ) ) ;
#3656 = DIRECTION ( 'NONE',  ( -1.000000000000000000, 0.000000000000000000, 0.000000000000000000 ) ) ;
#3657 = EDGE_LOOP ( 'NONE', ( #35777, #16401, #31053, #6724 ) ) ;
#3658 = DIRECTION ( 'NONE',  ( 1.000000000000000000, 0.000000000000000000, 0.000000000000000000 ) ) ;
#3659 = CARTESIAN_POINT ( 'NONE',  ( 0.000000000000000000, -80.02407177073008882, 78.64108602299921813 ) ) ;
#3660 = LINE ( 'NONE', #825, #35094 ) ;
#3661 = CARTESIAN_POINT ( 'NONE',  ( -70.10416666575086708, 31.00000000000000711, -4.581489278090966621 ) ) ;
#3662 = EDGE_LOOP ( 'NONE', ( #38086, #23873 ) ) ;
#3663 = CARTESIAN_POINT ( 'NONE',  ( -40.32452739092001792, 31.00000000000000355, -13.76986825753265897 ) ) ;
#3664 = CARTESIAN_POINT ( 'NONE',  ( -75.41724699911947027, 40.00000000000000711, 25.61573074746135248 ) ) ;
#3665 = DIRECTION ( 'NONE',  ( -1.000000000000000000, 0.000000000000000000, 0.000000000000000000 ) ) ;
#3666 = CARTESIAN_POINT ( 'NONE',  ( 0.2142857142857142738, -10.49781318335647917, -1.199999999999999956 ) ) ;
#3667 = ORIENTED_EDGE ( 'NONE', *, *, #19953, .T. ) ;
#3668 = CARTESIAN_POINT ( 'NONE',  ( 0.000000000000000000, -36.06787431788649911, -37.45808914225526820 ) ) ;
#3669 = DIRECTION ( 'NONE',  ( 0.000000000000000000, 0.3681245526846786964, -0.9297764858882511252 ) ) ;
#3670 = CIRCLE ( 'NONE', #28125, 59.00000000000000000 ) ;
#3671 = EDGE_LOOP ( 'NONE', ( #19488, #23768 ) ) ;
#3672 = CARTESIAN_POINT ( 'NONE',  ( 6.892732713553924917, 40.00000000000000000, -52.36990085009771434 ) ) ;
#3673 = CARTESIAN_POINT ( 'NONE',  ( 18.00000000000000355, -31.08872492059927595, -41.68322423723131465 ) ) ;
#3674 = CARTESIAN_POINT ( 'NONE',  ( 4.000000000000000000, 0.1981133338132474442, 2.382280164152719704E-17 ) ) ;
#3675 = VERTEX_POINT ( 'NONE', #10293 ) ;
#3676 = DIRECTION ( 'NONE',  ( -1.000000000000000000, -0.000000000000000000, 0.000000000000000000 ) ) ;
#3677 = CARTESIAN_POINT ( 'NONE',  ( 0.000000000000000000, -103.4151313792875158, 61.85306461934376188 ) ) ;
#3678 = ADVANCED_FACE ( 'NONE', ( #30370 ), #10766, .T. ) ;
#3679 = ADVANCED_FACE ( 'NONE', ( #27110 ), #37112, .T. ) ;
#3680 = ORIENTED_EDGE ( 'NONE', *, *, #27734, .F. ) ;
#3681 = DIRECTION ( 'NONE',  ( -1.000000000000000000, 0.000000000000000000, 0.000000000000000000 ) ) ;
#3682 = VERTEX_POINT ( 'NONE', #17318 ) ;
#3683 = EDGE_CURVE ( 'NONE', #37859, #17810, #27317, .T. ) ;
#3684 = AXIS2_PLACEMENT_3D ( 'NONE', #39624, #23104, #30483 ) ;
#3685 = EDGE_LOOP ( 'NONE', ( #20062, #30869, #13628, #17022 ) ) ;
#3686 = DIRECTION ( 'NONE',  ( 0.000000000000000000, -0.4999999999999989453, 0.8660254037844391517 ) ) ;
#3687 = CARTESIAN_POINT ( 'NONE',  ( -91.21105805184879500, 31.00000000000000711, 11.89862498597365104 ) ) ;
#3688 = ORIENTED_EDGE ( 'NONE', *, *, #27487, .T. ) ;
#3689 = CYLINDRICAL_SURFACE ( 'NONE', #1465, 59.00000000000000000 ) ;
#3690 = FACE_OUTER_BOUND ( 'NONE', #37695, .T. ) ;
#3691 = DIRECTION ( 'NONE',  ( -1.000000000000000000, 0.000000000000000000, 0.000000000000000000 ) ) ;
#3693 = EDGE_LOOP ( 'NONE', ( #17942, #8577, #41892, #26605 ) ) ;
#3692 = VECTOR ( 'NONE', #37529, 1000.000000000000000 ) ;
#3694 = CARTESIAN_POINT ( 'NONE',  ( -150.5000000000000284, -5.254679414958916394E-13, 10.00000000000000000 ) ) ;
#3695 = DIRECTION ( 'NONE',  ( -1.000000000000000000, 0.000000000000000000, -0.000000000000000000 ) ) ;
#3696 = EDGE_CURVE ( 'NONE', #42330, #5107, #17780, .T. ) ;
#3697 = AXIS2_PLACEMENT_3D ( 'NONE', #1156, #7929, #18444 ) ;
#3699 = DIRECTION ( 'NONE',  ( -1.000000000000000000, 0.000000000000000000, -0.000000000000000000 ) ) ;
#3698 = CYLINDRICAL_SURFACE ( 'NONE', #23904, 116.0000000000000000 ) ;
#3700 = AXIS2_PLACEMENT_3D ( 'NONE', #34480, #7214, #42833 ) ;
#3701 = DIRECTION ( 'NONE',  ( -1.000000000000000000, -0.000000000000000000, -0.000000000000000000 ) ) ;
#3702 = ORIENTED_EDGE ( 'NONE', *, *, #7845, .T. ) ;
#3703 = DIRECTION ( 'NONE',  ( -4.329780281177489232E-17, 1.000000000000000000, -4.329780281177443626E-17 ) ) ;
#3704 = AXIS2_PLACEMENT_3D ( 'NONE', #7177, #624, #20769 ) ;
#3705 = CARTESIAN_POINT ( 'NONE',  ( 4.888094100070568437, 31.00000000000000355, 37.04995123692341252 ) ) ;
#3706 = ORIENTED_EDGE ( 'NONE', *, *, #5925, .F. ) ;
#3707 = DIRECTION ( 'NONE',  ( 0.000000000000000000, 0.3612416661871537538, -0.9324722294043554793 ) ) ;
#3708 = LINE ( 'NONE', #20575, #27261 ) ;
#3709 = VERTEX_POINT ( 'NONE', #33203 ) ;
#3710 = LINE ( 'NONE', #29307, #4105 ) ;
#3711 = CARTESIAN_POINT ( 'NONE',  ( 35.44578089419255917, 40.00000000000000000, -40.42088417236866604 ) ) ;
#3712 = CARTESIAN_POINT ( 'NONE',  ( -22.33566874673302038, 40.00000000000000000, 45.10700316350094141 ) ) ;
#3713 = CIRCLE ( 'NONE', #34390, 116.0000000000000000 ) ;
#3714 = ORIENTED_EDGE ( 'NONE', *, *, #35671, .F. ) ;
#3715 = DIRECTION ( 'NONE',  ( -1.000000000000000000, 0.000000000000000000, 0.000000000000000000 ) ) ;
#3716 = DIRECTION ( 'NONE',  ( 0.000000000000000000, 0.000000000000000000, 1.000000000000000000 ) ) ;
#3717 = LINE ( 'NONE', #40389, #37065 ) ;
#3718 = ORIENTED_EDGE ( 'NONE', *, *, #26997, .F. ) ;
#3719 = CARTESIAN_POINT ( 'NONE',  ( -5.732510072307491988, 40.00000000000000000, -21.37570426403446078 ) ) ;
#3720 = ORIENTED_EDGE ( 'NONE', *, *, #12746, .T. ) ;
#3721 = CARTESIAN_POINT ( 'NONE',  ( -15.99999999999997691, 40.00000000000000000, -2.499999999999994671 ) ) ;
#3722 = CARTESIAN_POINT ( 'NONE',  ( 147.8499999999987153, 1.396194884625391392E-12, 9.999999999999960920 ) ) ;
#3723 = AXIS2_PLACEMENT_3D ( 'NONE', #1819, #5096, #41523 ) ;
#3724 = ORIENTED_EDGE ( 'NONE', *, *, #20212, .F. ) ;
#3725 = CARTESIAN_POINT ( 'NONE',  ( 17.99999999999999645, -91.51415974874549875, -64.91094698989387268 ) ) ;
#3726 = VECTOR ( 'NONE', #40532, 1000.000000000000000 ) ;
#3727 = EDGE_CURVE ( 'NONE', #37240, #9333, #3284, .T. ) ;
#3728 = DIRECTION ( 'NONE',  ( 0.000000000000000000, 0.000000000000000000, 1.000000000000000000 ) ) ;
#3729 = VERTEX_POINT ( 'NONE', #37758 ) ;
#3730 = DIRECTION ( 'NONE',  ( -1.000000000000000000, -1.836909530733573776E-16, 0.000000000000000000 ) ) ;
#3731 = ORIENTED_EDGE ( 'NONE', *, *, #16995, .F. ) ;
#3732 = CARTESIAN_POINT ( 'NONE',  ( -105.9879088449591933, 17.11489954122026447, 2.119280070842335384 ) ) ;
#3733 = AXIS2_PLACEMENT_3D ( 'NONE', #39429, #9127, #6070 ) ;
#3734 = ORIENTED_EDGE ( 'NONE', *, *, #34726, .T. ) ;
#3736 = ORIENTED_EDGE ( 'NONE', *, *, #30113, .T. ) ;
#3735 = CARTESIAN_POINT ( 'NONE',  ( 0.000000000000000000, -25.18647942089668490, -113.2326863338530245 ) ) ;
#3737 = CARTESIAN_POINT ( 'NONE',  ( -37.00582609755892349, 31.00000000000000355, 48.07482304779467341 ) ) ;
#3738 = ORIENTED_EDGE ( 'NONE', *, *, #11922, .F. ) ;
#3739 = DIRECTION ( 'NONE',  ( -1.000000000000000000, 0.000000000000000000, 0.000000000000000000 ) ) ;
#3740 = EDGE_CURVE ( 'NONE', #23341, #33051, #24724, .T. ) ;
#3741 = AXIS2_PLACEMENT_3D ( 'NONE', #33839, #41448, #5245 ) ;
#3742 = ORIENTED_EDGE ( 'NONE', *, *, #12506, .T. ) ;
#3743 = EDGE_CURVE ( 'NONE', #25070, #38187, #21024, .T. ) ;
#3744 = DIRECTION ( 'NONE',  ( 0.000000000000000000, 0.5528000653611888637, 0.8333139190825179510 ) ) ;
#3745 = ORIENTED_EDGE ( 'NONE', *, *, #21121, .T. ) ;
#3747 = CARTESIAN_POINT ( 'NONE',  ( 39.32569335900156915, 40.00000000000000000, 68.32161714264680086 ) ) ;
#3746 = CIRCLE ( 'NONE', #3054, 120.5010000000000190 ) ;
#3748 = EDGE_CURVE ( 'NONE', #10857, #40564, #22792, .T. ) ;
#3750 = DIRECTION ( 'NONE',  ( -1.000000000000000000, 0.000000000000000000, 0.000000000000000000 ) ) ;
#3749 = CYLINDRICAL_SURFACE ( 'NONE', #21754, 13.59999999999999787 ) ;
#3751 = DIRECTION ( 'NONE',  ( 0.000000000000000000, 0.000000000000000000, 1.000000000000000000 ) ) ;
#3752 = VERTEX_POINT ( 'NONE', #14455 ) ;
#3753 = DIRECTION ( 'NONE',  ( 1.000000000000000000, 0.000000000000000000, 0.000000000000000000 ) ) ;
#3754 = ORIENTED_EDGE ( 'NONE', *, *, #35389, .T. ) ;
#3755 =( LENGTH_UNIT ( ) NAMED_UNIT ( * ) SI_UNIT ( .MILLI., .METRE. ) );
#3756 =( LENGTH_UNIT ( ) NAMED_UNIT ( * ) SI_UNIT ( .MILLI., .METRE. ) );
#3757 = ORIENTED_EDGE ( 'NONE', *, *, #35139, .T. ) ;
#3758 = CIRCLE ( 'NONE', #28208, 51.99999999999999289 ) ;
#3759 = DIRECTION ( 'NONE',  ( 1.000000000000000000, 0.000000000000000000, 0.000000000000000000 ) ) ;
#3760 = CARTESIAN_POINT ( 'NONE',  ( -89.21153162435624040, 31.00000000000000711, 11.76024306507019901 ) ) ;
#3761 = ORIENTED_EDGE ( 'NONE', *, *, #2518, .F. ) ;
#3762 = CIRCLE ( 'NONE', #34438, 13.60000000000000320 ) ;
#3763 = FACE_BOUND ( 'NONE', #19743, .T. ) ;
#3764 = CIRCLE ( 'NONE', #17770, 12.59999999999999964 ) ;
#3765 = ADVANCED_FACE ( 'NONE', ( #41686 ), #18620, .T. ) ;
#3766 = ORIENTED_EDGE ( 'NONE', *, *, #23093, .F. ) ;
#3767 = DIRECTION ( 'NONE',  ( -0.000000000000000000, -0.000000000000000000, -1.000000000000000000 ) ) ;
#3768 = FACE_OUTER_BOUND ( 'NONE', #42830, .T. ) ;
#3769 = CARTESIAN_POINT ( 'NONE',  ( -87.85203729257557370, 31.00000000000000711, 50.59313708110082786 ) ) ;
#3770 = CARTESIAN_POINT ( 'NONE',  ( 0.2142857142857142738, -10.49781318335647917, 0.000000000000000000 ) ) ;
#3771 = EDGE_CURVE ( 'NONE', #32964, #16728, #10031, .T. ) ;
#3772 = AXIS2_PLACEMENT_3D ( 'NONE', #29357, #38933, #26299 ) ;
#3773 = ORIENTED_EDGE ( 'NONE', *, *, #30193, .T. ) ;
#3774 = CYLINDRICAL_SURFACE ( 'NONE', #2615, 20.00000000000000355 ) ;
#3775 = VERTEX_POINT ( 'NONE', #31011 ) ;
#3776 = DIRECTION ( 'NONE',  ( 0.000000000000000000, 0.2486898871648483278, 0.9685831611286327414 ) ) ;
#3777 = CARTESIAN_POINT ( 'NONE',  ( 0.000000000000000000, 0.000000000000000000, 0.000000000000000000 ) ) ;
#3778 = CLOSED_SHELL ( 'NONE', ( #7954, #24081, #17418, #24457, #27680, #30678, #2671, #16076, #28476, #9225, #26608, #42376, #37307, #31574, #5546, #42553, #283, #26396, #18331, #39239, #7829, #16380, #14380, #11847, #11276, #2304, #34821, #38037, #31679, #2982, #9918, #6212, #40968, #22931, #33695, #25396, #13267, #21109, #19532, #27393, #42922, #563, #16597, #15431, #17980, #10109, #29291, #14900, #23573, #12951, #39893, #15630, #33486, #18889, #4184, #25779, #13943, #39286, #15114, #28698, #16842, #33136, #11785, #33174, #31853, #40136, #16028, #40026, #13483, #28829, #23018, #12091, #23135, #23053, #3399, #6296, #23307, #30240, #3492, #32937, #22449, #33340, #11448, #2561, #24265, #3082, #9817, #2908, #20072, #35055, #14937, #41537, #28118, #22490, #531, #25266, #16497, #41096, #17462, #40730, #12025, #26822, #32770, #40985, #13293, #25972, #35332, #35827, #32249, #29799, #24494, #40365, #6575, #16636, #25350, #39529, #32711, #21846, #30865, #28535, #5590, #27656, #3234, #17190, #35867, #6131, #8629, #22174, #16923, #36362, #32186, #23940, #31596, #26335, #9187, #11405, #42607, #20190, #23748, #18714, #3639, #7100, #42844, #13798, #23091, #9250, #23870, #12845, #27801, #10175, #24284, #31200, #12882, #39112, #10546, #28090, #26037, #23126, #33929, #41933, #21955, #39603, #15760, #15959, #17473, #14269, #17026, #13501, #14829, #22057, #14880, #2230, #17925, #42704, #3145, #11491, #42318, #14681, #27420, #25162, #31833, #5522, #20876, #11174, #11945, #40083, #41646, #3765, #33509, #42994, #42097, #812, #7703, #36587, #19934, #32959, #20547, #38095, #108, #35500, #37219, #3916, #26627, #24146, #39629, #15537, #10613, #40556, #24607, #33344 ) ) ;
#3779 = CARTESIAN_POINT ( 'NONE',  ( 18.00000000000000355, 0.000000000000000000, 0.000000000000000000 ) ) ;
#3780 = ORIENTED_EDGE ( 'NONE', *, *, #931, .F. ) ;
#3781 = VERTEX_POINT ( 'NONE', #4827 ) ;
#3782 = DIRECTION ( 'NONE',  ( 0.000000000000000000, 0.000000000000000000, 1.000000000000000000 ) ) ;
#3783 = VECTOR ( 'NONE', #40726, 1000.000000000000000 ) ;
#3784 = ADVANCED_FACE ( 'NONE', ( #8315 ), #11606, .T. ) ;
#3785 = CARTESIAN_POINT ( 'NONE',  ( 17.99999999999999645, 16.77566611177777034, 119.3275660838943111 ) ) ;
#3786 = DIRECTION ( 'NONE',  ( 0.000000000000000000, 0.000000000000000000, 1.000000000000000000 ) ) ;
#3787 = AXIS2_PLACEMENT_3D ( 'NONE', #42274, #12429, #29872 ) ;
#3789 = ORIENTED_EDGE ( 'NONE', *, *, #34107, .F. ) ;
#3788 = CYLINDRICAL_SURFACE ( 'NONE', #29908, 13.60000000000000142 ) ;
#3790 = CARTESIAN_POINT ( 'NONE',  ( -31.59164309906361368, 31.00000000000000355, 4.115917706319392799 ) ) ;
#3791 = AXIS2_PLACEMENT_3D ( 'NONE', #7208, #20567, #17905 ) ;
#3792 = LINE ( 'NONE', #40248, #19571 ) ;
#3793 = CIRCLE ( 'NONE', #9392, 20.00000000000000711 ) ;
#3794 = ADVANCED_FACE ( 'NONE', ( #21234 ), #31884, .F. ) ;
#3796 = VERTEX_POINT ( 'NONE', #34276 ) ;
#3795 = DIRECTION ( 'NONE',  ( 0.000000000000000000, 0.000000000000000000, 1.000000000000000000 ) ) ;
#3797 = VECTOR ( 'NONE', #9925, 1000.000000000000000 ) ;
#3798 = VERTEX_POINT ( 'NONE', #37972 ) ;
#3799 = DIRECTION ( 'NONE',  ( 0.000000000000000000, -0.1062934856473723155, 0.9943348002101364269 ) ) ;
#3800 = DIRECTION ( 'NONE',  ( 0.000000000000000000, -0.8993121301712230231, 0.4373073204588476259 ) ) ;
#3801 = CARTESIAN_POINT ( 'NONE',  ( 56.82522199879618086, 40.00000000000000000, 7.581518937762242949 ) ) ;
#3802 = DIRECTION ( 'NONE',  ( -0.8191520442889875797, 1.003171929053519570E-16, 0.5735764363510522656 ) ) ;
#3803 = PRODUCT_DEFINITION_CONTEXT ( 'detailed design', #33984, 'design' ) ;
#3804 = EDGE_CURVE ( 'NONE', #22071, #8700, #17221, .T. ) ;
#3805 = DIRECTION ( 'NONE',  ( -1.000000000000000000, -0.000000000000000000, -0.000000000000000000 ) ) ;
#3806 = ORIENTED_EDGE ( 'NONE', *, *, #32676, .F. ) ;
#3807 = DIRECTION ( 'NONE',  ( 1.000000000000000000, 0.000000000000000000, 0.000000000000000000 ) ) ;
#3808 = ORIENTED_EDGE ( 'NONE', *, *, #10827, .F. ) ;
#3809 = AXIS2_PLACEMENT_3D ( 'NONE', #452, #6795, #3707 ) ;
#3810 = CARTESIAN_POINT ( 'NONE',  ( -10.00000000000000000, 0.000000000000000000, 0.000000000000000000 ) ) ;
#3811 = DIRECTION ( 'NONE',  ( 0.000000000000000000, 0.5076658003388409002, -0.8615540813938055154 ) ) ;
#3812 = CARTESIAN_POINT ( 'NONE',  ( 54.85378563033546584, 31.00000000000000355, 7.219977902337870290 ) ) ;
#3813 = CARTESIAN_POINT ( 'NONE',  ( 0.000000000000000000, 100.8494052988171035, 65.95368414178945216 ) ) ;
#3814 = EDGE_LOOP ( 'NONE', ( #38003, #26831, #17447, #26161 ) ) ;
#3815 = CIRCLE ( 'NONE', #12224, 31.49899999999999878 ) ;
#3816 = CIRCLE ( 'NONE', #28274, 20.00000000000000355 ) ;
#3817 = DIRECTION ( 'NONE',  ( -1.000000000000000000, -0.000000000000000000, 0.000000000000000000 ) ) ;
#3818 = VERTEX_POINT ( 'NONE', #38406 ) ;
#3819 = CARTESIAN_POINT ( 'NONE',  ( 21.81281596512078025, 40.00000000000000000, -10.76194779073239083 ) ) ;
#3820 = EDGE_CURVE ( 'NONE', #6869, #29181, #27764, .T. ) ;
#3821 = AXIS2_PLACEMENT_3D ( 'NONE', #37877, #7998, #1443 ) ;
#3822 = VERTEX_POINT ( 'NONE', #41241 ) ;
#3823 = CARTESIAN_POINT ( 'NONE',  ( -105.9879088449591933, 31.00000000000000711, 4.119280070842334496 ) ) ;
#3824 = EDGE_CURVE ( 'NONE', #34733, #1839, #21880, .T. ) ;
#3825 = DIRECTION ( 'NONE',  ( -1.000000000000000000, -0.000000000000000000, -0.000000000000000000 ) ) ;
#3826 = CARTESIAN_POINT ( 'NONE',  ( -58.00742674159663892, 31.00000000000000711, -44.63796826975934096 ) ) ;
#3828 = CARTESIAN_POINT ( 'NONE',  ( 25.34170449640226508, 40.00000000000000000, 74.97748276543396173 ) ) ;
#3827 = AXIS2_PLACEMENT_3D ( 'NONE', #23482, #10794, #30219 ) ;
#3829 = DIRECTION ( 'NONE',  ( -1.000000000000000000, 0.000000000000000000, 0.000000000000000000 ) ) ;
#3830 = CIRCLE ( 'NONE', #26180, 20.00000000000000000 ) ;
#3831 = VERTEX_POINT ( 'NONE', #34485 ) ;
#3832 = DIRECTION ( 'NONE',  ( 1.000000000000000000, 0.000000000000000000, 0.000000000000000000 ) ) ;
#3833 = ORIENTED_EDGE ( 'NONE', *, *, #15165, .F. ) ;
#3834 = DIRECTION ( 'NONE',  ( -1.000000000000000000, 0.000000000000000000, -0.000000000000000000 ) ) ;
#3835 = FACE_OUTER_BOUND ( 'NONE', #10840, .T. ) ;
#3837 = EDGE_LOOP ( 'NONE', ( #42775, #25495, #18855, #27797 ) ) ;
#3836 = CARTESIAN_POINT ( 'NONE',  ( -31.75000000000000000, 0.000000000000000000, 0.000000000000000000 ) ) ;
#3838 = FACE_OUTER_BOUND ( 'NONE', #13768, .T. ) ;
#3839 = EDGE_LOOP ( 'NONE', ( #23186, #13408 ) ) ;
#3840 = LINE ( 'NONE', #6922, #23106 ) ;
#3841 = CARTESIAN_POINT ( 'NONE',  ( -58.57471716409879292, 40.00000000000000711, 66.78942258476980953 ) ) ;
#3842 = DIRECTION ( 'NONE',  ( -1.000000000000000000, -0.000000000000000000, -0.000000000000000000 ) ) ;
#3843 = ORIENTED_EDGE ( 'NONE', *, *, #33671, .F. ) ;
#3844 = LINE ( 'NONE', #3635, #12298 ) ;
#3845 = CYLINDRICAL_SURFACE ( 'NONE', #27375, 120.5010000000000190 ) ;
#3846 = CIRCLE ( 'NONE', #28303, 116.0000000000000000 ) ;
#3847 = ORIENTED_EDGE ( 'NONE', *, *, #36443, .T. ) ;
#3848 = AXIS2_PLACEMENT_3D ( 'NONE', #15262, #21383, #38755 ) ;
#3849 = AXIS2_PLACEMENT_3D ( 'NONE', #21216, #34050, #11368 ) ;
#3850 = AXIS2_PLACEMENT_3D ( 'NONE', #40923, #11282, #31135 ) ;
#3851 = EDGE_CURVE ( 'NONE', #16399, #3211, #24715, .T. ) ;
#3852 = CARTESIAN_POINT ( 'NONE',  ( 0.000000000000000000, 0.000000000000000000, 0.000000000000000000 ) ) ;
#3853 = VERTEX_POINT ( 'NONE', #35132 ) ;
#3854 = LINE ( 'NONE', #807, #30305 ) ;
#3855 = EDGE_LOOP ( 'NONE', ( #1743, #18204, #28214, #22067, #41871 ) ) ;
#3856 = CARTESIAN_POINT ( 'NONE',  ( 18.71272080434063056, 40.00000000000000000, 21.38210947162712117 ) ) ;
#3857 = AXIS2_PLACEMENT_3D ( 'NONE', #10349, #14506, #34538 ) ;
#3858 = FACE_OUTER_BOUND ( 'NONE', #37039, .T. ) ;
#3859 = DIRECTION ( 'NONE',  ( -1.000000000000000000, 0.000000000000000000, 0.000000000000000000 ) ) ;
#3860 = VECTOR ( 'NONE', #37212, 1000.000000000000000 ) ;
#3861 = ADVANCED_FACE ( 'NONE', ( #41890 ), #4369, .F. ) ;
#3862 = COLOUR_RGB ( '', 0.31764706, 0.68627451, 0.89019608) ;
#3863 = PLANE ( 'NONE',  #999 ) ;
#3864 = CIRCLE ( 'NONE', #31785, 20.00000000000000711 ) ;
#3865 = CARTESIAN_POINT ( 'NONE',  ( -104.8158553526607477, 31.00000000000000711, 3.963965400206363565 ) ) ;
#3866 = ORIENTED_EDGE ( 'NONE', *, *, #33914, .F. ) ;
#3868 = DIRECTION ( 'NONE',  ( -1.000000000000000000, -0.000000000000000000, -0.000000000000000000 ) ) ;
#3867 = CARTESIAN_POINT ( 'NONE',  ( 0.000000000000000000, -44.47301969247432396, -16.68249143361957465 ) ) ;
#3869 = VERTEX_POINT ( 'NONE', #7660 ) ;
#3870 = LINE ( 'NONE', #27257, #37770 ) ;
#3871 = CARTESIAN_POINT ( 'NONE',  ( -28.96462450050677973, 31.00000000000000355, -9.827991688575851370 ) ) ;
#3872 = ORIENTED_EDGE ( 'NONE', *, *, #29001, .F. ) ;
#3873 = CARTESIAN_POINT ( 'NONE',  ( 17.99999999999999645, 101.8011932243955613, -55.61040422519224791 ) ) ;
#3874 = CYLINDRICAL_SURFACE ( 'NONE', #5633, 20.00000000000000355 ) ;
#3875 = ITEM_DEFINED_TRANSFORMATION ( 'NONE', 'NONE', #3741,  #13552 ) ;
#3876 = DIRECTION ( 'NONE',  ( 1.000000000000000000, 0.000000000000000000, 0.000000000000000000 ) ) ;
#3877 = CARTESIAN_POINT ( 'NONE',  ( -45.35818215263140019, 31.00000000000000355, 51.72168634911185592 ) ) ;
#3878 = EDGE_CURVE ( 'NONE', #5006, #2034, #28269, .T. ) ;
#3879 = EDGE_CURVE ( 'NONE', #39306, #38951, #26166, .T. ) ;
#3881 = ORIENTED_EDGE ( 'NONE', *, *, #27541, .T. ) ;
#3880 = AXIS2_PLACEMENT_3D ( 'NONE', #20307, #16821, #26821 ) ;
#3882 = CARTESIAN_POINT ( 'NONE',  ( -37.12595630542501368, 31.00000000000000355, 18.22532657727797556 ) ) ;
#3883 = EDGE_CURVE ( 'NONE', #42828, #25049, #22701, .T. ) ;
#3884 = EDGE_CURVE ( 'NONE', #8604, #13205, #21463, .T. ) ;
#3885 = AXIS2_PLACEMENT_3D ( 'NONE', #27697, #21171, #18334 ) ;
#3886 = CARTESIAN_POINT ( 'NONE',  ( 34.02738612458995959, 40.00000000000000000, 69.00154638599002510 ) ) ;
#3887 = CIRCLE ( 'NONE', #17187, 36.00000000000000000 ) ;
#3888 = AXIS2_PLACEMENT_3D ( 'NONE', #23696, #30215, #27596 ) ;
#3889 = DIRECTION ( 'NONE',  ( 1.000000000000000000, 0.000000000000000000, 0.000000000000000000 ) ) ;
#3890 = DIRECTION ( 'NONE',  ( -3.009274222672345096E-17, -1.000000000000000000, 2.455023325076454960E-18 ) ) ;
#3891 = CIRCLE ( 'NONE', #23451, 116.0000000000000000 ) ;
#3892 = ORIENTED_EDGE ( 'NONE', *, *, #4926, .T. ) ;
#3893 = LINE ( 'NONE', #43178, #915 ) ;
#3894 = CARTESIAN_POINT ( 'NONE',  ( -2.804994570502171047, -3.229033611042465335, -3.526374918436838701 ) ) ;
#3895 = ORIENTED_EDGE ( 'NONE', *, *, #22492, .F. ) ;
#3896 = CARTESIAN_POINT ( 'NONE',  ( -3.436116956419240864, 40.00000000000000000, -52.39583333462812931 ) ) ;
#3897 = CARTESIAN_POINT ( 'NONE',  ( 17.99999999999999645, 80.02407177073062883, -78.64108602299866391 ) ) ;
#3898 = DIRECTION ( 'NONE',  ( 1.000000000000000000, 0.000000000000000000, 0.000000000000000000 ) ) ;
#3899 = ORIENTED_EDGE ( 'NONE', *, *, #36187, .F. ) ;
#3900 = DIRECTION ( 'NONE',  ( 0.000000000000000000, -0.9714298932647074114, -0.2373266998711251186 ) ) ;
#3901 = DIRECTION ( 'NONE',  ( 1.000000000000000000, 0.000000000000000000, 0.000000000000000000 ) ) ;
#3902 = CIRCLE ( 'NONE', #40852, 116.0000000000000000 ) ;
#3903 = ORIENTED_EDGE ( 'NONE', *, *, #27957, .T. ) ;
#3904 = CARTESIAN_POINT ( 'NONE',  ( 18.00000000000000355, -15.49408907645202937, 44.90087086784588166 ) ) ;
#3905 = ORIENTED_EDGE ( 'NONE', *, *, #18105, .T. ) ;
#3906 = EDGE_CURVE ( 'NONE', #6921, #3091, #31737, .T. ) ;
#3907 = DIRECTION ( 'NONE',  ( -1.000000000000000000, 0.000000000000000000, -0.000000000000000000 ) ) ;
#3908 = ORIENTED_EDGE ( 'NONE', *, *, #42184, .T. ) ;
#3909 = CARTESIAN_POINT ( 'NONE',  ( 0.000000000000000000, 114.8812324315177023, -16.07179003769037351 ) ) ;
#3910 = CARTESIAN_POINT ( 'NONE',  ( 25.57473013255608052, 31.00000000000000355, 95.94174708837350352 ) ) ;
#3911 = VERTEX_POINT ( 'NONE', #12671 ) ;
#3912 = EDGE_CURVE ( 'NONE', #15607, #40494, #30331, .T. ) ;
#3913 = AXIS2_PLACEMENT_3D ( 'NONE', #4064, #26789, #17438 ) ;
#3914 = CARTESIAN_POINT ( 'NONE',  ( 0.000000000000000000, 112.5120133921113563, -43.14554256760899875 ) ) ;
#3915 = AXIS2_PLACEMENT_3D ( 'NONE', #15112, #5250, #28416 ) ;
#3916 = ADVANCED_FACE ( 'NONE', ( #39037 ), #22308, .T. ) ;
#3918 = CARTESIAN_POINT ( 'NONE',  ( 17.99999999999999645, -57.69704296431110890, -105.7900857083235451 ) ) ;
#3917 = AXIS2_PLACEMENT_3D ( 'NONE', #38975, #8254, #35285 ) ;
#3919 = ORIENTED_EDGE ( 'NONE', *, *, #2209, .F. ) ;
#3920 = AXIS2_PLACEMENT_3D ( 'NONE', #6424, #520, #36517 ) ;
#3921 = CARTESIAN_POINT ( 'NONE',  ( 0.000000000000000000, -9.484061862024134371, 30.03730300138978038 ) ) ;
#3922 = AXIS2_PLACEMENT_3D ( 'NONE', #39300, #32351, #3297 ) ;
#3923 = DIRECTION ( 'NONE',  ( 1.000000000000000000, 0.000000000000000000, 0.000000000000000000 ) ) ;
#3924 = CARTESIAN_POINT ( 'NONE',  ( 17.99999999999999645, 76.48293397876373945, -82.08917884620232996 ) ) ;
#3925 = CARTESIAN_POINT ( 'NONE',  ( 0.000000000000000000, -83.58328028049713510, 80.43528614701295965 ) ) ;
#3926 = ORIENTED_EDGE ( 'NONE', *, *, #4610, .T. ) ;
#3927 = CARTESIAN_POINT ( 'NONE',  ( 4.980795538363031681E-31, 19.99999999999998224, 2.775557561562891351E-14 ) ) ;
#3928 = AXIS2_PLACEMENT_3D ( 'NONE', #1953, #22073, #21653 ) ;
#3929 = DIRECTION ( 'NONE',  ( -1.000000000000000000, -0.000000000000000000, -0.000000000000000000 ) ) ;
#3930 = CARTESIAN_POINT ( 'NONE',  ( -33.98628324864968420, 31.00000000000000355, 19.63407011443918293 ) ) ;
#3931 = ORIENTED_EDGE ( 'NONE', *, *, #1573, .T. ) ;
#3932 = DIRECTION ( 'NONE',  ( 0.000000000000000000, 0.000000000000000000, 1.000000000000000000 ) ) ;
#3933 = VECTOR ( 'NONE', #13203, 1000.000000000000000 ) ;
#3934 = CYLINDRICAL_SURFACE ( 'NONE', #23792, 13.59999999999999787 ) ;
#3935 = ORIENTED_EDGE ( 'NONE', *, *, #31959, .T. ) ;
#3936 = EDGE_CURVE ( 'NONE', #300, #8500, #22518, .T. ) ;
#3937 = ADVANCED_FACE ( 'NONE', ( #39240 ), #15738, .F. ) ;
#3938 = DIRECTION ( 'NONE',  ( 0.000000000000000000, 0.000000000000000000, -1.000000000000000000 ) ) ;
#3939 = CARTESIAN_POINT ( 'NONE',  ( 47.00375723443311671, 40.00000000000000000, -27.15133022689256137 ) ) ;
#3940 = CARTESIAN_POINT ( 'NONE',  ( -3.331996295684063636, 40.00000000000000000, 49.59602437329134972 ) ) ;
#3941 = EDGE_CURVE ( 'NONE', #40301, #39732, #29654, .T. ) ;
#3942 = VERTEX_POINT ( 'NONE', #32718 ) ;
#3943 = FACE_OUTER_BOUND ( 'NONE', #12053, .T. ) ;
#3944 = DIRECTION ( 'NONE',  ( -1.000000000000000000, -0.000000000000000000, -0.000000000000000000 ) ) ;
#3945 = CIRCLE ( 'NONE', #31183, 2.649999999999985700 ) ;
#3946 = DIRECTION ( 'NONE',  ( -1.000000000000000000, -0.000000000000000000, 0.000000000000000000 ) ) ;
#3947 = CARTESIAN_POINT ( 'NONE',  ( 6.004904395537136175, 0.000000000000000000, 0.000000000000000000 ) ) ;
#3948 = VECTOR ( 'NONE', #39099, 1000.000000000000000 ) ;
#3949 = AXIS2_PLACEMENT_3D ( 'NONE', #9626, #26214, #23383 ) ;
#3950 = ORIENTED_EDGE ( 'NONE', *, *, #26322, .T. ) ;
#3951 = CARTESIAN_POINT ( 'NONE',  ( -9.654069774896838041, 40.00000000000000000, -19.56573356436190636 ) ) ;
#3952 = ORIENTED_EDGE ( 'NONE', *, *, #5296, .F. ) ;
#3953 = DIRECTION ( 'NONE',  ( 0.000000000000000000, 0.000000000000000000, 1.000000000000000000 ) ) ;
#3954 = CARTESIAN_POINT ( 'NONE',  ( 18.00000000000000355, 34.03046037009303149, -33.13733193845768454 ) ) ;
#3955 = VECTOR ( 'NONE', #11182, 1000.000000000000000 ) ;
#3956 = AXIS2_PLACEMENT_3D ( 'NONE', #23497, #43088, #13236 ) ;
#3957 = EDGE_CURVE ( 'NONE', #5769, #31074, #10841, .T. ) ;
#3958 = ORIENTED_EDGE ( 'NONE', *, *, #18939, .F. ) ;
#3959 = AXIS2_PLACEMENT_3D ( 'NONE', #38952, #39592, #35881 ) ;
#3960 = DIRECTION ( 'NONE',  ( 0.000000000000000000, 0.000000000000000000, 1.000000000000000000 ) ) ;
#3961 = DIRECTION ( 'NONE',  ( 0.000000000000000000, 0.5000000000000011102, 0.8660254037844379305 ) ) ;
#3962 = ORIENTED_EDGE ( 'NONE', *, *, #5095, .T. ) ;
#3963 = DIRECTION ( 'NONE',  ( 0.000000000000000000, 0.000000000000000000, 1.000000000000000000 ) ) ;
#3964 = ORIENTED_EDGE ( 'NONE', *, *, #7020, .F. ) ;
#3965 = CYLINDRICAL_SURFACE ( 'NONE', #21904, 59.00000000000000000 ) ;
#3966 = AXIS2_PLACEMENT_3D ( 'NONE', #25819, #19275, #32754 ) ;
#3967 = ORIENTED_EDGE ( 'NONE', *, *, #18558, .F. ) ;
#3969 = ORIENTED_EDGE ( 'NONE', *, *, #30636, .T. ) ;
#3968 = CARTESIAN_POINT ( 'NONE',  ( -102.9608013043458072, -40.05525454449572464, 14.45886780445738218 ) ) ;
#3970 = VECTOR ( 'NONE', #21919, 1000.000000000000000 ) ;
#3971 = CARTESIAN_POINT ( 'NONE',  ( -36.82253293460209420, 31.00000000000000355, -63.98115709646774718 ) ) ;
#3972 = EDGE_LOOP ( 'NONE', ( #9165, #35992, #22533, #36015 ) ) ;
#3973 = DIRECTION ( 'NONE',  ( 0.000000000000000000, 0.5264321628773507289, 0.8502171357296173237 ) ) ;
#3974 = EDGE_CURVE ( 'NONE', #37158, #39523, #10131, .T. ) ;
#3975 = ORIENTED_EDGE ( 'NONE', *, *, #6023, .F. ) ;
#3976 = LINE ( 'NONE', #26921, #37032 ) ;
#3977 = ORIENTED_EDGE ( 'NONE', *, *, #27373, .T. ) ;
#3978 = CARTESIAN_POINT ( 'NONE',  ( -23.42519174997118014, 40.00000000000000000, 87.00664592748896098 ) ) ;
#3979 = CIRCLE ( 'NONE', #39514, 58.99999999999998579 ) ;
#3981 = CARTESIAN_POINT ( 'NONE',  ( 18.00000000000000355, 0.000000000000000000, 0.000000000000000000 ) ) ;
#3980 = DIRECTION ( 'NONE',  ( -1.000000000000000000, 0.000000000000000000, 0.000000000000000000 ) ) ;
#3982 = CARTESIAN_POINT ( 'NONE',  ( 1.567478505476134606E-15, 4.618802153517012066, -5.000000000000000000 ) ) ;
#3983 = DIRECTION ( 'NONE',  ( -1.000000000000000000, 0.000000000000000000, 0.000000000000000000 ) ) ;
#3984 = ORIENTED_EDGE ( 'NONE', *, *, #4138, .T. ) ;
#3985 = AXIS2_PLACEMENT_3D ( 'NONE', #17943, #852, #27504 ) ;
#3986 =( NAMED_UNIT ( * ) SI_UNIT ( $, .STERADIAN. ) SOLID_ANGLE_UNIT ( ) );
#3987 = VECTOR ( 'NONE', #18870, 1000.000000000000000 ) ;
#3988 = AXIS2_PLACEMENT_3D ( 'NONE', #17432, #4277, #17649 ) ;
#3989 = EDGE_LOOP ( 'NONE', ( #17339, #7233, #33464, #23683 ) ) ;
#3990 = DIRECTION ( 'NONE',  ( -1.000000000000000000, 0.000000000000000000, 0.000000000000000000 ) ) ;
#3991 = CIRCLE ( 'NONE', #24238, 59.00000000000001421 ) ;
#3992 = CARTESIAN_POINT ( 'NONE',  ( 68.41617299536980568, 31.00000000000000000, 52.47886963225217016 ) ) ;
#3993 = FACE_BOUND ( 'NONE', #10577, .T. ) ;
#3994 = ORIENTED_EDGE ( 'NONE', *, *, #30132, .T. ) ;
#3995 = EDGE_CURVE ( 'NONE', #39242, #38361, #26188, .T. ) ;
#3996 = CYLINDRICAL_SURFACE ( 'NONE', #35884, 20.00000000000001066 ) ;
#3997 = VERTEX_POINT ( 'NONE', #5882 ) ;
#3998 = AXIS2_PLACEMENT_3D ( 'NONE', #13953, #17675, #6939 ) ;
#3999 = EDGE_LOOP ( 'NONE', ( #8976, #38022, #35165, #3667 ) ) ;
#4000 = CYLINDRICAL_SURFACE ( 'NONE', #13688, 2.500000000000002665 ) ;
#4001 = CARTESIAN_POINT ( 'NONE',  ( 0.000000000000000000, 35.11945359308111136, 38.34871548466026070 ) ) ;
#4002 = DIRECTION ( 'NONE',  ( -1.000000000000000000, 1.084202172485505420E-16, 0.000000000000000000 ) ) ;
#4003 = DIRECTION ( 'NONE',  ( -1.000000000000000000, 0.000000000000000000, 0.000000000000000000 ) ) ;
#4004 = EDGE_CURVE ( 'NONE', #34488, #6470, #19924, .T. ) ;
#4005 = ORIENTED_EDGE ( 'NONE', *, *, #30689, .F. ) ;
#4006 = DIRECTION ( 'NONE',  ( 1.000000000000000000, 0.000000000000000000, 0.000000000000000000 ) ) ;
#4007 = VERTEX_POINT ( 'NONE', #25359 ) ;
#4008 = LINE ( 'NONE', #10801, #42275 ) ;
#4009 = EDGE_CURVE ( 'NONE', #15839, #35006, #34521, .T. ) ;
#4010 = AXIS2_PLACEMENT_3D ( 'NONE', #40396, #10087, #13393 ) ;
#4011 = CARTESIAN_POINT ( 'NONE',  ( 106.4195705685734623, 106.4195705685780524, 10.00000000000025402 ) ) ;
#4012 = EDGE_CURVE ( 'NONE', #18529, #8193, #11564, .T. ) ;
#4013 = DIRECTION ( 'NONE',  ( -1.000000000000000000, 0.000000000000000000, -0.000000000000000000 ) ) ;
#4014 = ORIENTED_EDGE ( 'NONE', *, *, #12743, .T. ) ;
#4015 = ORIENTED_EDGE ( 'NONE', *, *, #18657, .F. ) ;
#4016 = DIRECTION ( 'NONE',  ( 0.000000000000000000, 0.000000000000000000, 1.000000000000000000 ) ) ;
#4017 = DIRECTION ( 'NONE',  ( -1.000000000000000000, -0.000000000000000000, -0.000000000000000000 ) ) ;
#4018 = VECTOR ( 'NONE', #25260, 1000.000000000000000 ) ;
#4019 = CARTESIAN_POINT ( 'NONE',  ( 4.000000000000000000, -1.700175430507292473, -3.320327275037661785 ) ) ;
#4021 = ORIENTED_EDGE ( 'NONE', *, *, #14218, .F. ) ;
#4020 = DIRECTION ( 'NONE',  ( 0.000000000000000000, -0.9822872507286865007, -0.1873813145857355367 ) ) ;
#4022 = CARTESIAN_POINT ( 'NONE',  ( -20.28213647682921206, 31.00000000000000355, 23.06128528321892546 ) ) ;
#4023 = CARTESIAN_POINT ( 'NONE',  ( -8.920000000000003482, 0.000000000000000000, 0.000000000000000000 ) ) ;
#4024 = CIRCLE ( 'NONE', #38890, 20.00000000000001066 ) ;
#4026 = ORIENTED_EDGE ( 'NONE', *, *, #41534, .T. ) ;
#4025 = LINE ( 'NONE', #30885, #40445 ) ;
#4027 = VERTEX_POINT ( 'NONE', #8959 ) ;
#4028 = ADVANCED_FACE ( 'NONE', ( #5675 ), #19032, .F. ) ;
#4029 = CARTESIAN_POINT ( 'NONE',  ( 0.000000000000000000, -76.48293397876204835, -82.08917884620389316 ) ) ;
#4030 = CARTESIAN_POINT ( 'NONE',  ( -7.015336270754768400, 40.00000000000000000, -53.95087245962636047 ) ) ;
#4031 = VECTOR ( 'NONE', #40676, 1000.000000000000000 ) ;
#4032 = LINE ( 'NONE', #971, #36056 ) ;
#4033 = DIRECTION ( 'NONE',  ( 1.000000000000000000, 0.000000000000000000, 0.000000000000000000 ) ) ;
#4034 = VERTEX_POINT ( 'NONE', #29047 ) ;
#4035 = DIRECTION ( 'NONE',  ( -1.000000000000000000, 0.000000000000000000, 0.000000000000000000 ) ) ;
#4036 = VERTEX_POINT ( 'NONE', #42313 ) ;
#4037 = CARTESIAN_POINT ( 'NONE',  ( 17.99999999999999645, -25.46650492921910924, 19.29328419707777087 ) ) ;
#4038 = CARTESIAN_POINT ( 'NONE',  ( 8.999999999999998224, -95.31344542257689056, -66.11616384574544725 ) ) ;
#4039 = CARTESIAN_POINT ( 'NONE',  ( -38.74991464700507748, 31.00000000000000355, 44.18781823130588293 ) ) ;
#4040 = CIRCLE ( 'NONE', #28492, 116.0000000000000000 ) ;
#4041 = DIRECTION ( 'NONE',  ( -1.000000000000000000, -0.000000000000000000, -0.000000000000000000 ) ) ;
#4042 = CIRCLE ( 'NONE', #28493, 120.5010000000000332 ) ;
#4043 = EDGE_LOOP ( 'NONE', ( #5060, #25425, #21799, #9186 ) ) ;
#4044 = AXIS2_PLACEMENT_3D ( 'NONE', #5844, #28374, #14845 ) ;
#4045 = EDGE_CURVE ( 'NONE', #8548, #33465, #32441, .T. ) ;
#4046 = FACE_OUTER_BOUND ( 'NONE', #37576, .T. ) ;
#4047 = ORIENTED_EDGE ( 'NONE', *, *, #37792, .F. ) ;
#4048 = CARTESIAN_POINT ( 'NONE',  ( -31.57754862722326905, 31.00000000000000355, 93.01713655900283584 ) ) ;
#4049 = CIRCLE ( 'NONE', #34036, 20.00000000000000000 ) ;
#4050 = ORIENTED_EDGE ( 'NONE', *, *, #28300, .T. ) ;
#4051 = CARTESIAN_POINT ( 'NONE',  ( 0.000000000000000000, 0.000000000000000000, 0.000000000000000000 ) ) ;
#4052 = DIRECTION ( 'NONE',  ( 0.000000000000000000, 0.000000000000000000, 1.000000000000000000 ) ) ;
#4053 = CARTESIAN_POINT ( 'NONE',  ( -4.761419979751499554, 31.00000000000000355, -74.40007767863900767 ) ) ;
#4054 = CARTESIAN_POINT ( 'NONE',  ( 67.48878131082858545, 39.99999999999999289, 39.09986611101696496 ) ) ;
#4055 = AXIS2_PLACEMENT_3D ( 'NONE', #23203, #10512, #6363 ) ;
#4056 = CYLINDRICAL_SURFACE ( 'NONE', #4875, 20.00000000000000355 ) ;
#4057 = EDGE_CURVE ( 'NONE', #26713, #31572, #12963, .T. ) ;
#4058 = VERTEX_POINT ( 'NONE', #38535 ) ;
#4059 = LINE ( 'NONE', #24409, #4659 ) ;
#4060 = VERTEX_POINT ( 'NONE', #28338 ) ;
#4061 = CARTESIAN_POINT ( 'NONE',  ( 18.00000000000000355, 15.49408907645172206, 44.90087086784598824 ) ) ;
#4062 = EDGE_CURVE ( 'NONE', #36925, #33209, #31771, .T. ) ;
#4063 = DIRECTION ( 'NONE',  ( 0.000000000000000000, 0.000000000000000000, 1.000000000000000000 ) ) ;
#4065 = ORIENTED_EDGE ( 'NONE', *, *, #9204, .F. ) ;
#4064 = CARTESIAN_POINT ( 'NONE',  ( 17.99999999999999645, 0.000000000000000000, 0.000000000000000000 ) ) ;
#4066 = EDGE_CURVE ( 'NONE', #3320, #2012, #39393, .T. ) ;
#4067 = CARTESIAN_POINT ( 'NONE',  ( 0.000000000000000000, 0.000000000000000000, 0.000000000000000000 ) ) ;
#4068 = VERTEX_POINT ( 'NONE', #21601 ) ;
#4069 = DIRECTION ( 'NONE',  ( 1.000000000000000000, 0.000000000000000000, 0.000000000000000000 ) ) ;
#4070 = CARTESIAN_POINT ( 'NONE',  ( 63.16980243745005907, 39.99999999999999289, -55.41789732285823078 ) ) ;
#4071 = DIRECTION ( 'NONE',  ( 1.000000000000000000, 0.000000000000000000, 0.000000000000000000 ) ) ;
#4072 = ORIENTED_EDGE ( 'NONE', *, *, #1416, .T. ) ;
#4073 = CARTESIAN_POINT ( 'NONE',  ( 17.99999999999999645, 120.4984140710909202, 0.7894348306988416830 ) ) ;
#4074 = VECTOR ( 'NONE', #13344, 1000.000000000000000 ) ;
#4075 = CYLINDRICAL_SURFACE ( 'NONE', #37095, 59.00000000000000000 ) ;
#4076 = CIRCLE ( 'NONE', #11822, 59.00000000000000000 ) ;
#4077 = ORIENTED_EDGE ( 'NONE', *, *, #40367, .F. ) ;
#4078 = CIRCLE ( 'NONE', #2001, 20.00000000000001066 ) ;
#4079 = DIRECTION ( 'NONE',  ( -1.000000000000000000, 0.000000000000000000, 0.000000000000000000 ) ) ;
#4080 = ORIENTED_EDGE ( 'NONE', *, *, #25929, .T. ) ;
#4081 = DIRECTION ( 'NONE',  ( -1.000000000000000000, -0.000000000000000000, -0.000000000000000000 ) ) ;
#4083 = ORIENTED_EDGE ( 'NONE', *, *, #17424, .T. ) ;
#4082 = EDGE_CURVE ( 'NONE', #42446, #3091, #42022, .T. ) ;
#4084 = CARTESIAN_POINT ( 'NONE',  ( -20.42974159057667194, 40.00000000000000000, -10.07157319949504526 ) ) ;
#4085 = DIRECTION ( 'NONE',  ( -1.000000000000000000, 0.000000000000000000, 0.000000000000000000 ) ) ;
#4086 = ADVANCED_FACE ( 'NONE', ( #31583 ), #28757, .F. ) ;
#4087 = DIRECTION ( 'NONE',  ( 0.000000000000000000, 0.9968120070307499025, 0.07978610555308651708 ) ) ;
#4088 = DIRECTION ( 'NONE',  ( -1.836909530733573776E-16, 1.000000000000000000, 0.000000000000000000 ) ) ;
#4089 = VERTEX_POINT ( 'NONE', #31808 ) ;
#4091 = DIRECTION ( 'NONE',  ( -1.000000000000000000, -0.000000000000000000, -0.000000000000000000 ) ) ;
#4090 = CARTESIAN_POINT ( 'NONE',  ( 2.500000000000000000, -1.178949249685214307, 2.042000000000001592 ) ) ;
#4092 = ORIENTED_EDGE ( 'NONE', *, *, #23023, .T. ) ;
#4093 = CARTESIAN_POINT ( 'NONE',  ( 17.99999999999999645, -101.1403355683150096, 56.80345518653453496 ) ) ;
#4094 = EDGE_CURVE ( 'NONE', #34149, #13162, #21379, .T. ) ;
#4095 = CARTESIAN_POINT ( 'NONE',  ( 7.411374251232441424, 31.00000000000000355, -21.84767871671174788 ) ) ;
#4096 = ORIENTED_EDGE ( 'NONE', *, *, #243, .F. ) ;
#4097 = CARTESIAN_POINT ( 'NONE',  ( 18.00000000000000355, 5.667686777401707232, 46.64153600743607342 ) ) ;
#4098 = DIRECTION ( 'NONE',  ( 0.000000000000000000, 0.5963673585385025344, -0.8027116379309628957 ) ) ;
#4099 = ITEM_DEFINED_TRANSFORMATION ( 'NONE', 'NONE', #40659,  #13552 ) ;
#4100 = EDGE_CURVE ( 'NONE', #36343, #5127, #12175, .T. ) ;
#4101 = DIRECTION ( 'NONE',  ( -1.000000000000000000, -0.000000000000000000, 0.000000000000000000 ) ) ;
#4102 = CARTESIAN_POINT ( 'NONE',  ( 57.13603463884887645, 31.00000000000000355, 32.98675068510902264 ) ) ;
#4103 = AXIS2_PLACEMENT_3D ( 'NONE', #14756, #21322, #41318 ) ;
#4104 = EDGE_LOOP ( 'NONE', ( #10081, #5809, #34680, #13639 ) ) ;
#4105 = VECTOR ( 'NONE', #16882, 1000.000000000000000 ) ;
#4106 = CARTESIAN_POINT ( 'NONE',  ( -11.35616125661755937, 31.00000000000000355, -42.69191301634815261 ) ) ;
#4107 = CARTESIAN_POINT ( 'NONE',  ( -10.16518460146908787, 40.00000000000000000, 77.20874865269769316 ) ) ;
#4108 = AXIS2_PLACEMENT_3D ( 'NONE', #41040, #21254, #34504 ) ;
#4109 = ADVANCED_FACE ( 'NONE', ( #31374 ), #31162, .F. ) ;
#4110 = CARTESIAN_POINT ( 'NONE',  ( 17.99999999999999645, 23.10276247328255650, -118.2656051737067600 ) ) ;
#4111 = DIRECTION ( 'NONE',  ( 0.000000000000000000, 0.000000000000000000, 1.000000000000000000 ) ) ;
#4112 = ADVANCED_FACE ( 'NONE', ( #34851 ), #21159, .F. ) ;
#4113 = LINE ( 'NONE', #10915, #17791 ) ;
#4115 = VERTEX_POINT ( 'NONE', #14811 ) ;
#4114 = DIRECTION ( 'NONE',  ( 0.000000000000000000, 0.000000000000000000, 1.000000000000000000 ) ) ;
#4116 = EDGE_CURVE ( 'NONE', #4270, #2710, #25536, .T. ) ;
#4117 = DIRECTION ( 'NONE',  ( -1.000000000000000000, -0.000000000000000000, 0.000000000000000000 ) ) ;
#4118 = CARTESIAN_POINT ( 'NONE',  ( 17.99999999999999645, 111.8797445107943531, 8.437727291344614855 ) ) ;
#4119 = EDGE_LOOP ( 'NONE', ( #27143, #6630, #29121, #38639 ) ) ;
#4120 = CARTESIAN_POINT ( 'NONE',  ( 23.58227068755204314, 40.00000000000000000, -47.84673847638903510 ) ) ;
#4122 = AXIS2_PLACEMENT_3D ( 'NONE', #13531, #13110, #26407 ) ;
#4121 = DIRECTION ( 'NONE',  ( -1.000000000000000000, 0.000000000000000000, 0.000000000000000000 ) ) ;
#4123 = FACE_OUTER_BOUND ( 'NONE', #31546, .T. ) ;
#4124 = ORIENTED_EDGE ( 'NONE', *, *, #23110, .F. ) ;
#4125 = LINE ( 'NONE', #17055, #17625 ) ;
#4126 = CARTESIAN_POINT ( 'NONE',  ( 8.919999999999998153, 0.000000000000000000, 0.000000000000000000 ) ) ;
#4127 = ORIENTED_EDGE ( 'NONE', *, *, #12070, .F. ) ;
#4128 = FACE_OUTER_BOUND ( 'NONE', #11854, .T. ) ;
#4129 = ORIENTED_EDGE ( 'NONE', *, *, #7629, .T. ) ;
#4130 = CARTESIAN_POINT ( 'NONE',  ( 0.000000000000000000, 84.62908780824989208, -85.78116633471202590 ) ) ;
#4132 = ORIENTED_EDGE ( 'NONE', *, *, #931, .T. ) ;
#4131 = AXIS2_PLACEMENT_3D ( 'NONE', #32656, #39305, #32150 ) ;
#4133 = CARTESIAN_POINT ( 'NONE',  ( 17.99999999999999645, 0.000000000000000000, 0.000000000000000000 ) ) ;
#4134 = EDGE_CURVE ( 'NONE', #1451, #35327, #15028, .T. ) ;
#4135 = CARTESIAN_POINT ( 'NONE',  ( 0.000000000000000000, -6.109652351742118626, 46.58570277113506819 ) ) ;
#4136 = ORIENTED_EDGE ( 'NONE', *, *, #8514, .T. ) ;
#4138 = EDGE_CURVE ( 'NONE', #3093, #26484, #28110, .T. ) ;
#4137 = CIRCLE ( 'NONE', #28575, 58.99999999999999289 ) ;
#4139 = ADVANCED_FACE ( 'NONE', ( #5169 ), #4963, .F. ) ;
#4140 = EDGE_CURVE ( 'NONE', #1441, #16, #17883, .T. ) ;
#4141 = DIRECTION ( 'NONE',  ( 0.000000000000000000, 0.000000000000000000, -1.000000000000000000 ) ) ;
#4142 = FACE_OUTER_BOUND ( 'NONE', #25674, .T. ) ;
#4143 = EDGE_LOOP ( 'NONE', ( #3926, #5413, #31657, #7925 ) ) ;
#4144 = DIRECTION ( 'NONE',  ( 0.000000000000000000, 0.7705132427757904745, -0.6374239897486881912 ) ) ;
#4145 = DIRECTION ( 'NONE',  ( 0.000000000000000000, 3.022535141193487712E-14, -1.000000000000000000 ) ) ;
#4146 = FACE_OUTER_BOUND ( 'NONE', #19482, .T. ) ;
#4147 = CARTESIAN_POINT ( 'NONE',  ( 0.000000000000000000, 0.000000000000000000, -1.199999999999999956 ) ) ;
#4148 = EDGE_LOOP ( 'NONE', ( #30828, #26318, #32191, #694 ) ) ;
#4149 = DIRECTION ( 'NONE',  ( 0.000000000000000000, -1.000000000000000000, 0.000000000000000000 ) ) ;
#4150 = LINE ( 'NONE', #30594, #10683 ) ;
#4151 = CARTESIAN_POINT ( 'NONE',  ( 34.89583333524210218, 31.00000000000000355, -2.290744634698907767 ) ) ;
#4152 = ORIENTED_EDGE ( 'NONE', *, *, #37137, .F. ) ;
#4153 = CARTESIAN_POINT ( 'NONE',  ( 18.00000000000000355, 43.83938735307292944, -18.28286404005752175 ) ) ;
#4154 = CYLINDRICAL_SURFACE ( 'NONE', #33265, 59.00000000000000000 ) ;
#4155 = ORIENTED_EDGE ( 'NONE', *, *, #32346, .F. ) ;
#4156 = CARTESIAN_POINT ( 'NONE',  ( 17.99999999999999645, 105.3681574666269256, -38.54638589714782881 ) ) ;
#4157 = CARTESIAN_POINT ( 'NONE',  ( 13.71368254939966036, 40.00000000000000000, -51.22554439249349656 ) ) ;
#4158 = CARTESIAN_POINT ( 'NONE',  ( -19.43072497041043079, 40.00000000000000000, 56.92208038676060511 ) ) ;
#4159 = EDGE_CURVE ( 'NONE', #19198, #23201, #33152, .T. ) ;
#4160 = ADVANCED_BREP_SHAPE_REPRESENTATION ( '', ( #13589, #13552 ), #31631 ) ;
#4161 = AXIS2_PLACEMENT_3D ( 'NONE', #1287, #14635, #11344 ) ;
#4162 = CIRCLE ( 'NONE', #2751, 116.0000000000000000 ) ;
#4163 = CYLINDRICAL_SURFACE ( 'NONE', #39435, 116.0000000000000000 ) ;
#4164 = CARTESIAN_POINT ( 'NONE',  ( 18.00000000000000355, -36.05989434073635636, 30.12041790338605551 ) ) ;
#4165 = EDGE_CURVE ( 'NONE', #19555, #15934, #30362, .T. ) ;
#4166 = VECTOR ( 'NONE', #34515, 1000.000000000000000 ) ;
#4167 = CARTESIAN_POINT ( 'NONE',  ( 0.000000000000000000, 0.000000000000000000, 0.000000000000000000 ) ) ;
#4168 = CYLINDRICAL_SURFACE ( 'NONE', #33577, 20.00000000000000355 ) ;
#4169 = VERTEX_POINT ( 'NONE', #10441 ) ;
#4170 = CARTESIAN_POINT ( 'NONE',  ( -1.472621547668719444, 40.00000000000000000, -22.39583333634585571 ) ) ;
#4171 = ORIENTED_EDGE ( 'NONE', *, *, #21769, .F. ) ;
#4172 = FACE_OUTER_BOUND ( 'NONE', #40555, .T. ) ;
#4173 = DIRECTION ( 'NONE',  ( 1.000000000000000000, 0.000000000000000000, 0.000000000000000000 ) ) ;
#4174 = ORIENTED_EDGE ( 'NONE', *, *, #31497, .F. ) ;
#4175 = DIRECTION ( 'NONE',  ( -1.000000000000000000, 0.000000000000000000, 0.000000000000000000 ) ) ;
#4176 = FACE_OUTER_BOUND ( 'NONE', #36811, .T. ) ;
#4177 = VERTEX_POINT ( 'NONE', #29890 ) ;
#4178 = LINE ( 'NONE', #7473, #1268 ) ;
#4179 = VERTEX_POINT ( 'NONE', #9995 ) ;
#4180 = DIRECTION ( 'NONE',  ( -3.996523416598930318E-16, 2.658563593772947863E-15, 1.000000000000000000 ) ) ;
#4181 = EDGE_LOOP ( 'NONE', ( #12378, #30826, #3773, #26628 ) ) ;
#4183 = ORIENTED_EDGE ( 'NONE', *, *, #854, .T. ) ;
#4182 = FACE_OUTER_BOUND ( 'NONE', #13823, .T. ) ;
#4184 = ADVANCED_FACE ( 'NONE', ( #26600 ), #597, .T. ) ;
#4186 = AXIS2_PLACEMENT_3D ( 'NONE', #12664, #8518, #38607 ) ;
#4185 = CARTESIAN_POINT ( 'NONE',  ( 66.15140951848846385, 31.00000000000000000, -38.07406969931856366 ) ) ;
#4187 = EDGE_LOOP ( 'NONE', ( #28475, #30183, #13933, #34459 ) ) ;
#4188 = DIRECTION ( 'NONE',  ( -1.000000000000000000, -0.000000000000000000, -0.000000000000000000 ) ) ;
#4189 = EDGE_CURVE ( 'NONE', #37469, #10174, #6498, .T. ) ;
#4190 = ADVANCED_FACE ( 'NONE', ( #19858 ), #30733, .T. ) ;
#4191 = ADVANCED_FACE ( 'NONE', ( #148 ), #7148, .T. ) ;
#4192 = AXIS2_PLACEMENT_3D ( 'NONE', #38765, #19394, #35912 ) ;
#4193 = ORIENTED_EDGE ( 'NONE', *, *, #38339, .T. ) ;
#4194 = LINE ( 'NONE', #7484, #39108 ) ;
#4195 = EDGE_CURVE ( 'NONE', #9994, #39678, #22024, .T. ) ;
#4196 = ORIENTED_EDGE ( 'NONE', *, *, #39192, .F. ) ;
#4197 = CARTESIAN_POINT ( 'NONE',  ( -89.42636861580037078, 40.00000000000000711, -24.07434901465519417 ) ) ;
#4198 = VECTOR ( 'NONE', #38327, 1000.000000000000000 ) ;
#4199 = VECTOR ( 'NONE', #30884, 1000.000000000000000 ) ;
#4200 = AXIS2_PLACEMENT_3D ( 'NONE', #6087, #42074, #2156 ) ;
#4202 = DIRECTION ( 'NONE',  ( -1.000000000000000000, -0.000000000000000000, -0.000000000000000000 ) ) ;
#4201 = CARTESIAN_POINT ( 'NONE',  ( 18.00000000000000355, 47.32430374665931794, 21.55018039121543438 ) ) ;
#4203 = AXIS2_PLACEMENT_3D ( 'NONE', #22737, #32303, #3245 ) ;
#4204 = EDGE_CURVE ( 'NONE', #34610, #24569, #5993, .T. ) ;
#4205 = DIRECTION ( 'NONE',  ( -1.000000000000000000, -0.000000000000000000, 0.000000000000000000 ) ) ;
#4206 = DIRECTION ( 'NONE',  ( 0.000000000000000000, 0.9407002666710319039, 0.3392388661180338882 ) ) ;
#4207 = ORIENTED_EDGE ( 'NONE', *, *, #5374, .T. ) ;
#4208 = CYLINDRICAL_SURFACE ( 'NONE', #22731, 47.49900000000000233 ) ;
#4209 = DIRECTION ( 'NONE',  ( 0.000000000000000000, 0.000000000000000000, 1.000000000000000000 ) ) ;
#4210 = CARTESIAN_POINT ( 'NONE',  ( 77.05880969081472642, 31.00000000000000000, 37.98468489477117771 ) ) ;
#4211 = DIRECTION ( 'NONE',  ( 0.000000000000000000, 0.000000000000000000, 1.000000000000000000 ) ) ;
#4212 = ORIENTED_EDGE ( 'NONE', *, *, #40417, .F. ) ;
#4213 = CIRCLE ( 'NONE', #15848, 51.99999999999999289 ) ;
#4214 = CARTESIAN_POINT ( 'NONE',  ( 8.075107282079295956, 40.00000000000000000, -23.73893940452291318 ) ) ;
#4215 = ORIENTED_EDGE ( 'NONE', *, *, #9916, .T. ) ;
#4216 = CIRCLE ( 'NONE', #34194, 59.00000000000000711 ) ;
#4217 = VERTEX_POINT ( 'NONE', #21916 ) ;
#4218 =( NAMED_UNIT ( * ) PLANE_ANGLE_UNIT ( ) SI_UNIT ( $, .RADIAN. ) );
#4219 = DIRECTION ( 'NONE',  ( 1.000000000000000000, 0.000000000000000000, 0.000000000000000000 ) ) ;
#4220 = LINE ( 'NONE', #30863, #26175 ) ;
#4221 = FACE_BOUND ( 'NONE', #10756, .T. ) ;
#4222 = AXIS2_PLACEMENT_3D ( 'NONE', #35229, #5355, #18722 ) ;
#4223 = EDGE_CURVE ( 'NONE', #10476, #21840, #5289, .T. ) ;
#4224 = VERTEX_POINT ( 'NONE', #8996 ) ;
#4225 = DIRECTION ( 'NONE',  ( 0.000000000000000000, 0.3641605752528168094, 0.9313361774523405412 ) ) ;
#4226 = ORIENTED_EDGE ( 'NONE', *, *, #28900, .F. ) ;
#4227 = CARTESIAN_POINT ( 'NONE',  ( 0.000000000000000000, 90.81729652456166946, 72.16798910853647442 ) ) ;
#4228 = CARTESIAN_POINT ( 'NONE',  ( -16.80298683001097260, 31.00000000000000355, 2.367532924972516994 ) ) ;
#4229 = CIRCLE ( 'NONE', #28657, 36.00000000000000000 ) ;
#4230 = DIRECTION ( 'NONE',  ( -1.000000000000000000, 0.000000000000000000, 0.000000000000000000 ) ) ;
#4231 = TOROIDAL_SURFACE ( 'NONE', #31428, 14.91999999999999815, 0.08000000000000020983 ) ;
#4232 = DIRECTION ( 'NONE',  ( -1.000000000000000000, -0.000000000000000000, -0.000000000000000000 ) ) ;
#4233 = EDGE_LOOP ( 'NONE', ( #37828, #38523, #36491, #14282, #3599, #30070, #8392, #9395, #11512, #40219, #19104, #21567, #19961, #35781, #42014, #41297, #19739, #32050, #20009, #17336, #29884, #26607, #26119, #33390, #7628, #26668 ) ) ;
#4234 = ORIENTED_EDGE ( 'NONE', *, *, #18836, .F. ) ;
#4235 = CARTESIAN_POINT ( 'NONE',  ( 18.00000000000001421, 0.000000000000000000, 7.500000000000000000 ) ) ;
#4236 = DIRECTION ( 'NONE',  ( -1.000000000000000000, -0.000000000000000000, -0.000000000000000000 ) ) ;
#4237 = FACE_OUTER_BOUND ( 'NONE', #13780, .T. ) ;
#4238 = VECTOR ( 'NONE', #33566, 1000.000000000000000 ) ;
#4239 = ORIENTED_EDGE ( 'NONE', *, *, #35830, .T. ) ;
#4241 = EDGE_LOOP ( 'NONE', ( #32530, #25409, #4394, #4891 ) ) ;
#4240 = CARTESIAN_POINT ( 'NONE',  ( 0.000000000000000000, -109.4038418350900059, -50.51029986767660773 ) ) ;
#4242 = CARTESIAN_POINT ( 'NONE',  ( -26.91141215548883991, 31.00000000000000355, 30.57553017914614557 ) ) ;
#4243 = DIRECTION ( 'NONE',  ( -1.000000000000000000, 0.000000000000000000, -0.000000000000000000 ) ) ;
#4244 = EDGE_CURVE ( 'NONE', #13499, #20659, #19994, .T. ) ;
#4245 = EDGE_CURVE ( 'NONE', #25151, #20337, #33182, .T. ) ;
#4247 = VERTEX_POINT ( 'NONE', #31696 ) ;
#4246 = CARTESIAN_POINT ( 'NONE',  ( 0.000000000000000000, 80.74349901498408144, 77.90224541347306797 ) ) ;
#4248 = EDGE_CURVE ( 'NONE', #20315, #14728, #5319, .T. ) ;
#4249 = UNCERTAINTY_MEASURE_WITH_UNIT (LENGTH_MEASURE( 1.000000000000000082E-05 ), #41344, 'distance_accuracy_value', 'NONE');
#4250 = ORIENTED_EDGE ( 'NONE', *, *, #34628, .F. ) ;
#4251 = CARTESIAN_POINT ( 'NONE',  ( 63.11376326756305843, 39.99999999999999289, -21.32174659672108774 ) ) ;
#4252 = DIRECTION ( 'NONE',  ( -1.000000000000000000, 0.000000000000000000, 0.000000000000000000 ) ) ;
#4253 = CARTESIAN_POINT ( 'NONE',  ( 0.000000000000000000, -83.49789599728724454, -86.88263557826851979 ) ) ;
#4254 = ORIENTED_EDGE ( 'NONE', *, *, #1513, .T. ) ;
#4255 = CARTESIAN_POINT ( 'NONE',  ( 17.99999999999999645, 2.418575551220858877, 120.4767259403369053 ) ) ;
#4256 = EDGE_CURVE ( 'NONE', #7493, #25155, #38870, .T. ) ;
#4257 = ORIENTED_EDGE ( 'NONE', *, *, #42315, .F. ) ;
#4258 = AXIS2_PLACEMENT_3D ( 'NONE', #19063, #2835, #29080 ) ;
#4259 = CARTESIAN_POINT ( 'NONE',  ( -9.000000000000005329, 1.641026710857453510E-15, 13.40000000000000213 ) ) ;
#4260 = DIRECTION ( 'NONE',  ( -1.000000000000000000, -0.000000000000000000, -0.000000000000000000 ) ) ;
#4261 = VECTOR ( 'NONE', #19912, 1000.000000000000000 ) ;
#4262 = EDGE_CURVE ( 'NONE', #27389, #18211, #33873, .T. ) ;
#4263 = CARTESIAN_POINT ( 'NONE',  ( 3.763366191185776088, 31.00000000000000355, 57.39583333449059666 ) ) ;
#4264 = DIRECTION ( 'NONE',  ( 1.000000000000000000, 0.000000000000000000, 0.000000000000000000 ) ) ;
#4265 = ORIENTED_EDGE ( 'NONE', *, *, #17602, .F. ) ;
#4266 = LINE ( 'NONE', #17202, #10048 ) ;
#4267 = ORIENTED_EDGE ( 'NONE', *, *, #19133, .T. ) ;
#4268 = CARTESIAN_POINT ( 'NONE',  ( -15.87544005811639458, 40.00000000000000000, -27.47754625559162989 ) ) ;
#4269 = CIRCLE ( 'NONE', #5009, 120.5010000000000332 ) ;
#4270 = VERTEX_POINT ( 'NONE', #28654 ) ;
#4271 = CYLINDRICAL_SURFACE ( 'NONE', #36759, 11.00000000000000000 ) ;
#4272 = CARTESIAN_POINT ( 'NONE',  ( 6.075999999999998735, 0.000000000000000000, 15.08402000000000065 ) ) ;
#4273 = CARTESIAN_POINT ( 'NONE',  ( -46.76215110878947456, 31.00000000000000355, 53.15211786535368788 ) ) ;
#4274 = CARTESIAN_POINT ( 'NONE',  ( 74.15939217265263039, 39.99999999999999289, -19.75058139460558237 ) ) ;
#4275 = DIRECTION ( 'NONE',  ( -1.000000000000000000, 0.000000000000000000, 0.000000000000000000 ) ) ;
#4276 = ORIENTED_EDGE ( 'NONE', *, *, #29821, .F. ) ;
#4277 = DIRECTION ( 'NONE',  ( -1.000000000000000000, 0.000000000000000000, 0.000000000000000000 ) ) ;
#4278 = ORIENTED_EDGE ( 'NONE', *, *, #5722, .F. ) ;
#4279 = CARTESIAN_POINT ( 'NONE',  ( 17.99999999999999645, -109.1131968884000258, 26.12628443611856355 ) ) ;
#4280 = FACE_OUTER_BOUND ( 'NONE', #13855, .T. ) ;
#4282 = EDGE_LOOP ( 'NONE', ( #39399, #26149, #25064, #141 ) ) ;
#4281 = DIRECTION ( 'NONE',  ( 0.000000000000000000, 0.000000000000000000, 1.000000000000000000 ) ) ;
#4283 = CARTESIAN_POINT ( 'NONE',  ( 18.00000000000000355, 0.000000000000000000, 0.000000000000000000 ) ) ;
#4284 = EDGE_LOOP ( 'NONE', ( #39949, #32196, #8791, #40838 ) ) ;
#4285 = DIRECTION ( 'NONE',  ( 0.000000000000000000, 0.2631025642275152121, 0.9647678688145175929 ) ) ;
#4286 = CARTESIAN_POINT ( 'NONE',  ( 75.74279358916429317, 39.99999999999999289, -37.35102017232331661 ) ) ;
#4287 = DIRECTION ( 'NONE',  ( -1.000000000000000000, -0.000000000000000000, 0.000000000000000000 ) ) ;
#4288 = AXIS2_PLACEMENT_3D ( 'NONE', #16302, #19168, #6246 ) ;
#4289 = ORIENTED_EDGE ( 'NONE', *, *, #12463, .T. ) ;
#4290 = LINE ( 'NONE', #15025, #22102 ) ;
#4291 = CYLINDRICAL_SURFACE ( 'NONE', #21145, 13.59999999999999964 ) ;
#4292 = CIRCLE ( 'NONE', #21782, 2.649999999999985700 ) ;
#4293 = ADVANCED_FACE ( 'NONE', ( #22133, #38234 ), #15153, .F. ) ;
#4294 = VERTEX_POINT ( 'NONE', #41926 ) ;
#4295 = DIRECTION ( 'NONE',  ( 0.000000000000000000, 0.5877852522924742473, -0.8090169943749466741 ) ) ;
#4296 = VERTEX_POINT ( 'NONE', #12076 ) ;
#4297 = DIRECTION ( 'NONE',  ( -3.996523416598930318E-16, 2.658563593772947863E-15, 1.000000000000000000 ) ) ;
#4298 = ORIENTED_EDGE ( 'NONE', *, *, #28288, .T. ) ;
#4299 = CARTESIAN_POINT ( 'NONE',  ( 23.40755275317130568, 40.00000000000000000, 30.61714766194360848 ) ) ;
#4300 = CARTESIAN_POINT ( 'NONE',  ( -10.00000000000000000, 0.000000000000000000, 0.000000000000000000 ) ) ;
#4301 = EDGE_CURVE ( 'NONE', #18949, #21981, #8803, .T. ) ;
#4302 = CYLINDRICAL_SURFACE ( 'NONE', #2386, 64.99999999999997158 ) ;
#4303 = DIRECTION ( 'NONE',  ( -3.996523416598930318E-16, 2.658563593772947863E-15, 1.000000000000000000 ) ) ;
#4304 = VERTEX_POINT ( 'NONE', #34963 ) ;
#4306 = DIRECTION ( 'NONE',  ( -1.000000000000000000, -0.000000000000000000, -0.000000000000000000 ) ) ;
#4305 = DIRECTION ( 'NONE',  ( 1.000000000000000000, 0.000000000000000000, 0.000000000000000000 ) ) ;
#4307 = EDGE_CURVE ( 'NONE', #22785, #42289, #8122, .T. ) ;
#4308 = VERTEX_POINT ( 'NONE', #11864 ) ;
#4309 = DIRECTION ( 'NONE',  ( -1.000000000000000000, -0.000000000000000000, 0.000000000000000000 ) ) ;
#4310 = EDGE_CURVE ( 'NONE', #1973, #6784, #27464, .T. ) ;
#4311 = CARTESIAN_POINT ( 'NONE',  ( 7.028922914820973311, 31.00000000000000355, 26.21578750688660264 ) ) ;
#4312 = ORIENTED_EDGE ( 'NONE', *, *, #3743, .F. ) ;
#4313 = CARTESIAN_POINT ( 'NONE',  ( -10.00000000000000000, 0.000000000000000000, 0.000000000000000000 ) ) ;
#4314 = ADVANCED_FACE ( 'NONE', ( #40739 ), #20956, .F. ) ;
#4315 = DIRECTION ( 'NONE',  ( 1.000000000000000000, 0.000000000000000000, 0.000000000000000000 ) ) ;
#4316 = DIRECTION ( 'NONE',  ( -0.000000000000000000, 0.000000000000000000, -1.000000000000000000 ) ) ;
#4317 = CIRCLE ( 'NONE', #7824, 130.0000000000000284 ) ;
#4318 = CARTESIAN_POINT ( 'NONE',  ( 23.52215716829092074, 31.00000000000000355, -69.29398394448777765 ) ) ;
#4319 = CIRCLE ( 'NONE', #125, 59.00000000000000711 ) ;
#4320 = ORIENTED_EDGE ( 'NONE', *, *, #4379, .T. ) ;
#4321 = CARTESIAN_POINT ( 'NONE',  ( 46.89968353241609833, 31.00000000000000355, -2.988513402017745513 ) ) ;
#4322 = AXIS2_PLACEMENT_3D ( 'NONE', #42064, #12014, #12222 ) ;
#4323 = CARTESIAN_POINT ( 'NONE',  ( 71.66629920589342362, 39.99999999999999289, 24.32769631419027689 ) ) ;
#4324 = EDGE_CURVE ( 'NONE', #32742, #28827, #30740, .T. ) ;
#4325 = EDGE_CURVE ( 'NONE', #2530, #30690, #31805, .T. ) ;
#4326 = VECTOR ( 'NONE', #35971, 1000.000000000000000 ) ;
#4327 = DIRECTION ( 'NONE',  ( 1.000000000000000000, -0.000000000000000000, 0.000000000000000000 ) ) ;
#4328 = DIRECTION ( 'NONE',  ( 1.000000000000000000, 0.000000000000000000, 0.000000000000000000 ) ) ;
#4329 = EDGE_CURVE ( 'NONE', #16399, #33425, #26222, .T. ) ;
#4330 = FACE_OUTER_BOUND ( 'NONE', #41752, .T. ) ;
#4332 = ORIENTED_EDGE ( 'NONE', *, *, #24391, .F. ) ;
#4331 = CARTESIAN_POINT ( 'NONE',  ( 0.000000000000000000, -7.162210897276078292, 51.50439529848826226 ) ) ;
#4333 = CYLINDRICAL_SURFACE ( 'NONE', #29572, 36.00000000000000000 ) ;
#4334 = FACE_OUTER_BOUND ( 'NONE', #31231, .T. ) ;
#4335 = ORIENTED_EDGE ( 'NONE', *, *, #31361, .F. ) ;
#4336 = CARTESIAN_POINT ( 'NONE',  ( -45.59965607524345899, 40.00000000000000000, -22.47439267160796916 ) ) ;
#4337 = DIRECTION ( 'NONE',  ( 0.000000000000000000, 0.000000000000000000, 1.000000000000000000 ) ) ;
#4338 = CARTESIAN_POINT ( 'NONE',  ( 18.00000000000000355, 0.000000000000000000, 0.000000000000000000 ) ) ;
#4339 = ORIENTED_EDGE ( 'NONE', *, *, #21426, .F. ) ;
#4340 = DIRECTION ( 'NONE',  ( -3.009274222672345096E-17, -1.000000000000000000, 2.455023325076455345E-18 ) ) ;
#4341 = DIRECTION ( 'NONE',  ( 1.000000000000000000, 0.000000000000000000, 0.000000000000000000 ) ) ;
#4342 = ORIENTED_EDGE ( 'NONE', *, *, #25053, .T. ) ;
#4343 = CARTESIAN_POINT ( 'NONE',  ( 17.99999999999999645, 0.000000000000000000, 0.000000000000000000 ) ) ;
#4344 = VERTEX_POINT ( 'NONE', #7599 ) ;
#4345 = EDGE_CURVE ( 'NONE', #6806, #16376, #7157, .T. ) ;
#4346 = VECTOR ( 'NONE', #15678, 1000.000000000000000 ) ;
#4347 = DIRECTION ( 'NONE',  ( -1.000000000000000000, -0.000000000000000000, 0.000000000000000000 ) ) ;
#4348 = ORIENTED_EDGE ( 'NONE', *, *, #5297, .F. ) ;
#4349 = DIRECTION ( 'NONE',  ( 0.000000000000000000, 0.000000000000000000, 1.000000000000000000 ) ) ;
#4350 = DIRECTION ( 'NONE',  ( 0.000000000000000000, 0.000000000000000000, -1.000000000000000000 ) ) ;
#4351 = VERTEX_POINT ( 'NONE', #30102 ) ;
#4352 = AXIS2_PLACEMENT_3D ( 'NONE', #143, #801, #13507 ) ;
#4353 = CYLINDRICAL_SURFACE ( 'NONE', #19923, 2.500000000000002665 ) ;
#4354 = DIRECTION ( 'NONE',  ( 0.000000000000000000, 0.000000000000000000, 1.000000000000000000 ) ) ;
#4355 = ORIENTED_EDGE ( 'NONE', *, *, #13030, .F. ) ;
#4356 = CARTESIAN_POINT ( 'NONE',  ( 9.000000000000001776, -51.19683565102437939, -9.104066087303991139 ) ) ;
#4357 = EDGE_CURVE ( 'NONE', #28923, #17108, #2836, .T. ) ;
#4358 = CIRCLE ( 'NONE', #35716, 2.500000000000000444 ) ;
#4359 = DIRECTION ( 'NONE',  ( -1.000000000000000000, 0.000000000000000000, 0.000000000000000000 ) ) ;
#4360 = EDGE_CURVE ( 'NONE', #3320, #31004, #24157, .T. ) ;
#4361 = DIRECTION ( 'NONE',  ( 1.000000000000000000, 0.000000000000000000, 0.000000000000000000 ) ) ;
#4362 = DIRECTION ( 'NONE',  ( -1.000000000000000000, 0.000000000000000000, 0.000000000000000000 ) ) ;
#4363 = ORIENTED_EDGE ( 'NONE', *, *, #10593, .T. ) ;
#4364 = DIRECTION ( 'NONE',  ( -0.9999999999999998890, -1.040834085586084257E-17, 1.387778780781445676E-17 ) ) ;
#4365 = CARTESIAN_POINT ( 'NONE',  ( 9.000000000000000000, -0.6168405712484084091, -35.99471499692226928 ) ) ;
#4366 = CARTESIAN_POINT ( 'NONE',  ( -9.824444021593908616, 31.00000000000000355, 36.70529466175499778 ) ) ;
#4367 = ORIENTED_EDGE ( 'NONE', *, *, #36129, .F. ) ;
#4369 = CYLINDRICAL_SURFACE ( 'NONE', #4551, 59.00000000000000000 ) ;
#4368 = CARTESIAN_POINT ( 'NONE',  ( -109.0695705685749317, 106.4195705685765603, 10.00000000000033573 ) ) ;
#4370 = CARTESIAN_POINT ( 'NONE',  ( 18.00000000000000355, -46.87740477351715640, 16.82754413119429771 ) ) ;
#4371 = EDGE_LOOP ( 'NONE', ( #33595, #23159, #19710, #31319 ) ) ;
#4372 = CARTESIAN_POINT ( 'NONE',  ( 150.5000000000000284, 1.576403824487674918E-12, 9.999999999999998224 ) ) ;
#4373 = CARTESIAN_POINT ( 'NONE',  ( -36.80126402429788612, 40.00000000000000000, 32.28896105221774349 ) ) ;
#4374 = CARTESIAN_POINT ( 'NONE',  ( 44.54779904932823342, 40.00000000000000000, -34.05916983163054113 ) ) ;
#4375 = CIRCLE ( 'NONE', #9960, 47.49900000000000233 ) ;
#4376 = EDGE_CURVE ( 'NONE', #37783, #10089, #42917, .T. ) ;
#4377 = FACE_OUTER_BOUND ( 'NONE', #2776, .T. ) ;
#4378 = DIRECTION ( 'NONE',  ( 0.000000000000000000, 0.8993121301712174720, 0.4373073204588591723 ) ) ;
#4379 = EDGE_CURVE ( 'NONE', #9315, #19383, #17461, .T. ) ;
#4380 = PRODUCT_DEFINITION ( 'UNKNOWN', '', #37904, #1203 ) ;
#4381 = CARTESIAN_POINT ( 'NONE',  ( 17.99999999999999645, -11.58753559615507100, 29.77419532459258278 ) ) ;
#4382 = DIRECTION ( 'NONE',  ( 0.000000000000000000, -0.9968120070307493474, -0.07978610555309334496 ) ) ;
#4383 = MECHANICAL_DESIGN_GEOMETRIC_PRESENTATION_REPRESENTATION (  '', ( #23250 ), #7887 ) ;
#4384 = ORIENTED_EDGE ( 'NONE', *, *, #15602, .T. ) ;
#4385 = CARTESIAN_POINT ( 'NONE',  ( 19.70274684888802952, 40.00000000000000000, 17.27304525429847359 ) ) ;
#4386 = VERTEX_POINT ( 'NONE', #34212 ) ;
#4387 = CARTESIAN_POINT ( 'NONE',  ( 0.000000000000000000, 0.000000000000000000, 9.999999999999998224 ) ) ;
#4388 = CIRCLE ( 'NONE', #41327, 120.5010000000000474 ) ;
#4389 = CARTESIAN_POINT ( 'NONE',  ( 17.99999999999999645, -11.58753559615507100, 29.77419532459258278 ) ) ;
#4390 = ORIENTED_EDGE ( 'NONE', *, *, #10873, .T. ) ;
#4391 = ADVANCED_FACE ( 'NONE', ( #30948 ), #33778, .F. ) ;
#4392 = CARTESIAN_POINT ( 'NONE',  ( 18.00000000000000355, -27.43636312076348815, 38.14186064215142835 ) ) ;
#4393 = DIRECTION ( 'NONE',  ( -1.000000000000000000, -0.000000000000000000, -0.000000000000000000 ) ) ;
#4394 = ORIENTED_EDGE ( 'NONE', *, *, #24254, .T. ) ;
#4395 = CARTESIAN_POINT ( 'NONE',  ( 0.000000000000000000, 0.000000000000000000, 0.000000000000000000 ) ) ;
#4396 = ORIENTED_EDGE ( 'NONE', *, *, #30179, .F. ) ;
#4397 = EDGE_CURVE ( 'NONE', #13782, #18607, #37354, .T. ) ;
#4398 = ORIENTED_EDGE ( 'NONE', *, *, #30577, .F. ) ;
#4400 = ORIENTED_EDGE ( 'NONE', *, *, #650, .T. ) ;
#4399 = DIRECTION ( 'NONE',  ( 0.000000000000000000, 0.000000000000000000, 1.000000000000000000 ) ) ;
#4401 = CARTESIAN_POINT ( 'NONE',  ( 9.885896071376816252, 31.00000000000000355, -74.20985814147174153 ) ) ;
#4402 = VERTEX_POINT ( 'NONE', #17250 ) ;
#4403 = CARTESIAN_POINT ( 'NONE',  ( 0.000000000000000000, -11.46872990052349550, -45.56340405422456286 ) ) ;
#4404 = VECTOR ( 'NONE', #35127, 1000.000000000000114 ) ;
#4405 = ORIENTED_EDGE ( 'NONE', *, *, #14189, .F. ) ;
#4406 = CARTESIAN_POINT ( 'NONE',  ( 4.211140560182196957, -2.431303136016555122, -3.745885042887436622 ) ) ;
#4407 = EDGE_CURVE ( 'NONE', #1396, #33317, #24863, .T. ) ;
#4408 = ORIENTED_EDGE ( 'NONE', *, *, #33506, .F. ) ;
#4409 = VECTOR ( 'NONE', #22961, 1000.000000000000000 ) ;
#4410 = CARTESIAN_POINT ( 'NONE',  ( -68.52217190868857699, 40.00000000000000711, 59.94826526062049510 ) ) ;
#4411 = EDGE_CURVE ( 'NONE', #40482, #35201, #14171, .T. ) ;
#4413 = FACE_OUTER_BOUND ( 'NONE', #31086, .T. ) ;
#4412 = DIRECTION ( 'NONE',  ( 0.000000000000000000, 0.9826841245925214130, -0.1852887240871113894 ) ) ;
#4414 = CARTESIAN_POINT ( 'NONE',  ( 18.00000000000000355, 0.000000000000000000, 0.000000000000000000 ) ) ;
#4415 = FACE_OUTER_BOUND ( 'NONE', #19079, .T. ) ;
#4416 =( GEOMETRIC_REPRESENTATION_CONTEXT ( 3 ) GLOBAL_UNCERTAINTY_ASSIGNED_CONTEXT ( ( #39027 ) ) GLOBAL_UNIT_ASSIGNED_CONTEXT ( ( #41067, #7495, #34112 ) ) REPRESENTATION_CONTEXT ( 'NONE', 'WORKASPACE' ) );
#4417 = VERTEX_POINT ( 'NONE', #10659 ) ;
#4418 = FACE_OUTER_BOUND ( 'NONE', #13049, .T. ) ;
#4419 = AXIS2_PLACEMENT_3D ( 'NONE', #17524, #39779, #33261 ) ;
#4420 = ORIENTED_EDGE ( 'NONE', *, *, #14189, .T. ) ;
#4421 = DIRECTION ( 'NONE',  ( 1.000000000000000000, -0.000000000000000000, -0.000000000000000000 ) ) ;
#4422 = CARTESIAN_POINT ( 'NONE',  ( 26.74431375183570481, 31.00000000000000355, -78.78324499025107741 ) ) ;
#4423 = DIRECTION ( 'NONE',  ( 1.000000000000000000, 0.000000000000000000, 0.000000000000000000 ) ) ;
#4424 = ORIENTED_EDGE ( 'NONE', *, *, #19959, .T. ) ;
#4425 = CARTESIAN_POINT ( 'NONE',  ( 6.473670811831357064, 40.00000000000000000, -24.11571013580714151 ) ) ;
#4426 = ORIENTED_EDGE ( 'NONE', *, *, #19419, .F. ) ;
#4427 = EDGE_CURVE ( 'NONE', #42118, #10039, #13718, .T. ) ;
#4428 = ORIENTED_EDGE ( 'NONE', *, *, #5908, .F. ) ;
#4429 = CARTESIAN_POINT ( 'NONE',  ( 8.999999999999998224, -106.6051926090974007, 45.73109345704783379 ) ) ;
#4430 = CARTESIAN_POINT ( 'NONE',  ( 0.000000000000000000, 19.47322409167269441, 30.27859877001407796 ) ) ;
#4431 = EDGE_CURVE ( 'NONE', #1632, #1619, #36019, .T. ) ;
#4432 = DIRECTION ( 'NONE',  ( -0.000000000000000000, -1.060184893785364939E-15, -1.000000000000000000 ) ) ;
#4433 = EDGE_CURVE ( 'NONE', #34842, #5268, #40831, .T. ) ;
#4434 = EDGE_CURVE ( 'NONE', #31940, #36886, #10224, .T. ) ;
#4435 = CARTESIAN_POINT ( 'NONE',  ( 8.999999999999998224, -19.47322409167291113, 30.27859877001393230 ) ) ;
#4436 = CIRCLE ( 'NONE', #2339, 58.99999999999999289 ) ;
#4437 = ORIENTED_EDGE ( 'NONE', *, *, #41870, .T. ) ;
#4438 = CARTESIAN_POINT ( 'NONE',  ( 1.598609366639573350E-14, -1.063425437509180407E-13, -40.00000000000000000 ) ) ;
#4439 = ORIENTED_EDGE ( 'NONE', *, *, #3771, .F. ) ;
#4440 = DIRECTION ( 'NONE',  ( 0.000000000000000000, 0.000000000000000000, -1.000000000000000000 ) ) ;
#4441 = DIRECTION ( 'NONE',  ( 0.000000000000000000, 0.000000000000000000, 1.000000000000000000 ) ) ;
#4442 = CARTESIAN_POINT ( 'NONE',  ( 17.99999999999999645, -51.27532863109435368, 99.79535634195110561 ) ) ;
#4443 = CARTESIAN_POINT ( 'NONE',  ( 17.99999999999999645, 0.000000000000000000, 0.000000000000000000 ) ) ;
#4444 = VERTEX_POINT ( 'NONE', #6944 ) ;
#4445 = ORIENTED_EDGE ( 'NONE', *, *, #23810, .F. ) ;
#4446 = DIRECTION ( 'NONE',  ( 0.000000000000000000, 0.000000000000000000, 1.000000000000000000 ) ) ;
#4447 = AXIS2_PLACEMENT_3D ( 'NONE', #30796, #34478, #37325 ) ;
#4448 = DIRECTION ( 'NONE',  ( -1.000000000000000000, -0.000000000000000000, 0.000000000000000000 ) ) ;
#4449 = AXIS2_PLACEMENT_3D ( 'NONE', #40376, #7006, #20157 ) ;
#4450 = CARTESIAN_POINT ( 'NONE',  ( 9.000000000000001776, 13.00789606333630566, -115.2683592318613819 ) ) ;
#4451 = CIRCLE ( 'NONE', #28873, 120.5010000000000190 ) ;
#4452 = ORIENTED_EDGE ( 'NONE', *, *, #42125, .F. ) ;
#4454 = ORIENTED_EDGE ( 'NONE', *, *, #7875, .F. ) ;
#4453 = CYLINDRICAL_SURFACE ( 'NONE', #41743, 59.00000000000000000 ) ;
#4455 = CARTESIAN_POINT ( 'NONE',  ( 46.49836147156941024, 31.00000000000000355, -6.043767708844123732 ) ) ;
#4456 = CARTESIAN_POINT ( 'NONE',  ( -3.983177536951265640, -13.66651769228263191, -1.199999999999999956 ) ) ;
#4457 = AXIS2_PLACEMENT_3D ( 'NONE', #5451, #35110, #42292 ) ;
#4458 = CARTESIAN_POINT ( 'NONE',  ( 0.000000000000000000, 2.123073309835184386, 47.45152853935334747 ) ) ;
#4459 = AXIS2_PLACEMENT_3D ( 'NONE', #16810, #30098, #9998 ) ;
#4460 = ORIENTED_EDGE ( 'NONE', *, *, #6305, .T. ) ;
#4461 = CARTESIAN_POINT ( 'NONE',  ( 64.47787635702036368, 39.99999999999999289, -17.16423577040998438 ) ) ;
#4462 = CIRCLE ( 'NONE', #8651, 116.0000000000000000 ) ;
#4463 = ADVANCED_FACE ( 'NONE', ( #8029 ), #1473, .T. ) ;
#4464 = CARTESIAN_POINT ( 'NONE',  ( -10.00000000000000000, 0.000000000000000000, 36.00000000000000000 ) ) ;
#4465 = EDGE_CURVE ( 'NONE', #40313, #42137, #1689, .T. ) ;
#4466 = DIRECTION ( 'NONE',  ( -1.000000000000000000, 0.000000000000000000, 0.000000000000000000 ) ) ;
#4467 = ORIENTED_EDGE ( 'NONE', *, *, #42735, .F. ) ;
#4468 = DIRECTION ( 'NONE',  ( 0.000000000000000000, 0.000000000000000000, 1.000000000000000000 ) ) ;
#4469 = VERTEX_POINT ( 'NONE', #8670 ) ;
#4470 = SHAPE_REPRESENTATION_RELATIONSHIP ( 'NONE' , 'NONE' ,  #10434, #29166 ) ;
#4471 = AXIS2_PLACEMENT_3D ( 'NONE', #38743, #38955, #42440 ) ;
#4472 = DIRECTION ( 'NONE',  ( -1.000000000000000000, -0.000000000000000000, -0.000000000000000000 ) ) ;
#4473 = LINE ( 'NONE', #6896, #8062 ) ;
#4474 = CARTESIAN_POINT ( 'NONE',  ( 35.44578089419255917, 31.00000000000000355, -40.42088417236866604 ) ) ;
#4475 = CARTESIAN_POINT ( 'NONE',  ( 0.000000000000000000, 0.000000000000000000, 4.000000000000000000 ) ) ;
#4476 = ORIENTED_EDGE ( 'NONE', *, *, #31522, .F. ) ;
#4477 = EDGE_LOOP ( 'NONE', ( #40614, #38803, #13504, #15692 ) ) ;
#4478 = DIRECTION ( 'NONE',  ( -1.000000000000000000, 0.000000000000000000, 0.000000000000000000 ) ) ;
#4479 = ORIENTED_EDGE ( 'NONE', *, *, #35792, .F. ) ;
#4480 = CARTESIAN_POINT ( 'NONE',  ( 25.50046184691807483, 40.00000000000000000, -22.37655979312362931 ) ) ;
#4481 = VERTEX_POINT ( 'NONE', #41620 ) ;
#4482 = CARTESIAN_POINT ( 'NONE',  ( 0.000000000000000000, 36.06787431788731624, -37.45808914225450081 ) ) ;
#4483 = CARTESIAN_POINT ( 'NONE',  ( 0.000000000000000000, 0.000000000000000000, 0.000000000000000000 ) ) ;
#4484 = CARTESIAN_POINT ( 'NONE',  ( -74.30604906370724905, 31.00000000000000711, -36.76128443491435860 ) ) ;
#4485 = CARTESIAN_POINT ( 'NONE',  ( -81.66074000183850501, 40.00000000000000711, -10.87165890510346777 ) ) ;
#4486 = EDGE_CURVE ( 'NONE', #5452, #37135, #38546, .T. ) ;
#4487 = EDGE_CURVE ( 'NONE', #40347, #17666, #17901, .T. ) ;
#4488 = DIRECTION ( 'NONE',  ( -3.996523416598930318E-16, 2.658563593772947863E-15, 1.000000000000000000 ) ) ;
#4489 = AXIS2_PLACEMENT_3D ( 'NONE', #19385, #33299, #6666 ) ;
#4490 = EDGE_CURVE ( 'NONE', #5055, #2401, #17185, .T. ) ;
#4491 = CIRCLE ( 'NONE', #6574, 58.99999999999999289 ) ;
#4492 = ORIENTED_EDGE ( 'NONE', *, *, #6268, .F. ) ;
#4493 = FACE_OUTER_BOUND ( 'NONE', #30512, .T. ) ;
#4494 = EDGE_LOOP ( 'NONE', ( #42346, #32881, #40537, #10585 ) ) ;
#4495 = DIRECTION ( 'NONE',  ( 2.731800627175558911E-17, 1.000000000000000000, -3.170996607629411740E-18 ) ) ;
#4496 = AXIS2_PLACEMENT_3D ( 'NONE', #32148, #22574, #2861 ) ;
#4497 = CARTESIAN_POINT ( 'NONE',  ( -132.0000507999999968, 0.000000000000000000, 7.500000000000000000 ) ) ;
#4498 = VECTOR ( 'NONE', #4478, 1000.000000000000000 ) ;
#4500 = ORIENTED_EDGE ( 'NONE', *, *, #28256, .F. ) ;
#4499 = CARTESIAN_POINT ( 'NONE',  ( 0.000000000000000000, 36.34385289850590794, 29.77717097092089205 ) ) ;
#4501 = CARTESIAN_POINT ( 'NONE',  ( 17.99999999999999645, -107.5680526044917542, -31.89649718262205269 ) ) ;
#4502 = EDGE_LOOP ( 'NONE', ( #15982, #4454 ) ) ;
#4503 = DIRECTION ( 'NONE',  ( -1.000000000000000000, -0.000000000000000000, 0.000000000000000000 ) ) ;
#4504 = AXIS2_PLACEMENT_3D ( 'NONE', #32846, #33283, #16286 ) ;
#4505 = CARTESIAN_POINT ( 'NONE',  ( -89.62817255407412631, 40.00000000000000711, -11.80141054548196422 ) ) ;
#4506 = DIRECTION ( 'NONE',  ( -1.000000000000000000, -0.000000000000000000, -0.000000000000000000 ) ) ;
#4507 = VERTEX_POINT ( 'NONE', #11772 ) ;
#4508 = ADVANCED_FACE ( 'NONE', ( #28123 ), #1906, .F. ) ;
#4509 = DIRECTION ( 'NONE',  ( 0.000000000000000000, -1.000000000000000000, 5.297542245118643184E-16 ) ) ;
#4510 = DIRECTION ( 'NONE',  ( -3.009274222672345712E-17, -1.000000000000000000, 2.455023325076455345E-18 ) ) ;
#4511 = CIRCLE ( 'NONE', #13583, 31.49900000000000233 ) ;
#4513 = DIRECTION ( 'NONE',  ( -1.000000000000000000, 1.373900992973642066E-15, 3.979293995072266947E-16 ) ) ;
#4512 =( NAMED_UNIT ( * ) SI_UNIT ( $, .STERADIAN. ) SOLID_ANGLE_UNIT ( ) );
#4514 = ORIENTED_EDGE ( 'NONE', *, *, #7794, .F. ) ;
#4515 = DIRECTION ( 'NONE',  ( 0.000000000000000000, 0.4132121857683728194, 0.9106347728549155640 ) ) ;
#4516 = ORIENTED_EDGE ( 'NONE', *, *, #39991, .T. ) ;
#4517 = DIRECTION ( 'NONE',  ( -1.000000000000000000, -0.000000000000000000, 0.000000000000000000 ) ) ;
#4518 = CARTESIAN_POINT ( 'NONE',  ( 32.62694724487211317, 40.00000000000000000, -16.02036196159510339 ) ) ;
#4519 = CARTESIAN_POINT ( 'NONE',  ( 17.99999999999999645, -22.66088087769196235, 21.87856208362548571 ) ) ;
#4520 = DIRECTION ( 'NONE',  ( 0.000000000000000000, 0.000000000000000000, 1.000000000000000000 ) ) ;
#4521 = AXIS2_PLACEMENT_3D ( 'NONE', #41107, #37840, #27629 ) ;
#4522 = EDGE_CURVE ( 'NONE', #19733, #30654, #9487, .T. ) ;
#4523 = CARTESIAN_POINT ( 'NONE',  ( 9.000000000000000000, 35.78425302087538995, 3.935382540232920334 ) ) ;
#4524 = ORIENTED_EDGE ( 'NONE', *, *, #5048, .T. ) ;
#4526 = CYLINDRICAL_SURFACE ( 'NONE', #22383, 59.00000000000000000 ) ;
#4525 = DIRECTION ( 'NONE',  ( -1.000000000000000000, 0.000000000000000000, 0.000000000000000000 ) ) ;
#4527 = ORIENTED_EDGE ( 'NONE', *, *, #13395, .T. ) ;
#4528 = AXIS2_PLACEMENT_3D ( 'NONE', #6066, #39204, #42913 ) ;
#4529 = CARTESIAN_POINT ( 'NONE',  ( 109.0695705685756565, -106.4195705685758213, 9.999999999999667821 ) ) ;
#4530 = DIRECTION ( 'NONE',  ( -1.000000000000000000, -0.000000000000000000, -0.000000000000000000 ) ) ;
#4531 = AXIS2_PLACEMENT_3D ( 'NONE', #38981, #9103, #22458 ) ;
#4532 = CARTESIAN_POINT ( 'NONE',  ( -20.72449291656876369, 31.00000000000000355, -23.61699481730619610 ) ) ;
#4533 = ORIENTED_EDGE ( 'NONE', *, *, #36202, .T. ) ;
#4534 = CYLINDRICAL_SURFACE ( 'NONE', #8547, 13.60000000000000142 ) ;
#4535 = CIRCLE ( 'NONE', #8037, 51.99999999999999289 ) ;
#4536 = DIRECTION ( 'NONE',  ( 1.000000000000000000, 0.000000000000000000, 0.000000000000000000 ) ) ;
#4537 = DIRECTION ( 'NONE',  ( 0.000000000000000000, 0.9968120070307504577, -0.07978610555307970309 ) ) ;
#4538 = CARTESIAN_POINT ( 'NONE',  ( -79.69263343296167079, 31.00000000000000711, -10.49242979028127820 ) ) ;
#4539 = ORIENTED_EDGE ( 'NONE', *, *, #32834, .F. ) ;
#4540 = CARTESIAN_POINT ( 'NONE',  ( -26.91141215548883991, 31.00000000000000355, 30.57553017914614557 ) ) ;
#4541 = EDGE_CURVE ( 'NONE', #20905, #30050, #20983, .T. ) ;
#4542 = CARTESIAN_POINT ( 'NONE',  ( 81.71702119589899382, 39.99999999999999289, -47.19735719316410183 ) ) ;
#4543 = AXIS2_PLACEMENT_3D ( 'NONE', #43182, #14019, #36672 ) ;
#4544 = DIRECTION ( 'NONE',  ( -3.009274222672345096E-17, -1.000000000000000000, 2.455023325076455345E-18 ) ) ;
#4545 = DIRECTION ( 'NONE',  ( -1.000000000000000000, -0.000000000000000000, -0.000000000000000000 ) ) ;
#4546 = CARTESIAN_POINT ( 'NONE',  ( 42.80287614962796994, -2.055254544495723756, 69.29271901957280022 ) ) ;
#4547 = VECTOR ( 'NONE', #14119, 1000.000000000000000 ) ;
#4548 = ADVANCED_FACE ( 'NONE', ( #31386 ), #4526, .F. ) ;
#4550 = ORIENTED_EDGE ( 'NONE', *, *, #26397, .F. ) ;
#4549 = CARTESIAN_POINT ( 'NONE',  ( 17.99999999999999645, 101.8011932243948081, 55.61040422519366189 ) ) ;
#4551 = AXIS2_PLACEMENT_3D ( 'NONE', #18185, #24507, #37548 ) ;
#4552 = DIRECTION ( 'NONE',  ( 1.000000000000000000, 0.000000000000000000, 0.000000000000000000 ) ) ;
#4553 = DIRECTION ( 'NONE',  ( 0.000000000000000000, 0.000000000000000000, 1.000000000000000000 ) ) ;
#4554 = EDGE_CURVE ( 'NONE', #42747, #28980, #32795, .T. ) ;
#4555 = CIRCLE ( 'NONE', #28979, 20.00000000000000000 ) ;
#4556 = ORIENTED_EDGE ( 'NONE', *, *, #33158, .T. ) ;
#4557 = CARTESIAN_POINT ( 'NONE',  ( -40.54929543462775143, 40.00000000000000000, -46.21859917192507794 ) ) ;
#4558 = LINE ( 'NONE', #1065, #10428 ) ;
#4559 = DIRECTION ( 'NONE',  ( 0.000000000000000000, 0.000000000000000000, -1.000000000000000000 ) ) ;
#4560 = AXIS2_PLACEMENT_3D ( 'NONE', #27887, #38103, #11744 ) ;
#4561 = EDGE_LOOP ( 'NONE', ( #10273, #28524, #17345, #37937 ) ) ;
#4562 = AXIS2_PLACEMENT_3D ( 'NONE', #5825, #29200, #32666 ) ;
#4563 = DIRECTION ( 'NONE',  ( -1.000000000000000000, 0.000000000000000000, 0.000000000000000000 ) ) ;
#4564 = DIRECTION ( 'NONE',  ( 0.000000000000000000, 0.000000000000000000, 1.000000000000000000 ) ) ;
#4565 = CIRCLE ( 'NONE', #28990, 47.49900000000000233 ) ;
#4566 = ADVANCED_FACE ( 'NONE', ( #25098 ), #24891, .F. ) ;
#4567 = ORIENTED_EDGE ( 'NONE', *, *, #9643, .T. ) ;
#4568 = CYLINDRICAL_SURFACE ( 'NONE', #21513, 59.00000000000001421 ) ;
#4569 = VERTEX_POINT ( 'NONE', #40962 ) ;
#4570 = CIRCLE ( 'NONE', #29692, 1.000000000000000666 ) ;
#4571 = CARTESIAN_POINT ( 'NONE',  ( 18.00000000000000355, 0.000000000000000000, 0.000000000000000000 ) ) ;
#4572 = VERTEX_POINT ( 'NONE', #7813 ) ;
#4573 = DIRECTION ( 'NONE',  ( 0.000000000000000000, 0.000000000000000000, 1.000000000000000000 ) ) ;
#4574 = CARTESIAN_POINT ( 'NONE',  ( -98.36195137685432144, 31.00000000000000711, 26.22212808231157055 ) ) ;
#4575 = EDGE_LOOP ( 'NONE', ( #14731, #14161, #28611, #40835 ) ) ;
#4576 = CARTESIAN_POINT ( 'NONE',  ( 0.000000000000000000, 0.000000000000000000, 0.000000000000000000 ) ) ;
#4577 = FACE_OUTER_BOUND ( 'NONE', #37114, .T. ) ;
#4578 = ORIENTED_EDGE ( 'NONE', *, *, #23142, .T. ) ;
#4579 = CARTESIAN_POINT ( 'NONE',  ( 50.00005079999999680, 1.836970198721029589E-15, -15.00000000000000000 ) ) ;
#4580 = EDGE_CURVE ( 'NONE', #36933, #29613, #39715, .T. ) ;
#4581 = CARTESIAN_POINT ( 'NONE',  ( 9.000000000000001776, -12.30077720129131613, 50.52416135122077634 ) ) ;
#4583 = EDGE_LOOP ( 'NONE', ( #30063, #12227 ) ) ;
#4582 = AXIS2_PLACEMENT_3D ( 'NONE', #40626, #1150, #20199 ) ;
#4584 = CARTESIAN_POINT ( 'NONE',  ( 18.00000000000000355, 29.60891106212788415, 37.14118181634774629 ) ) ;
#4585 = CARTESIAN_POINT ( 'NONE',  ( -9.000000000000007105, 0.000000000000000000, 0.000000000000000000 ) ) ;
#4586 = CIRCLE ( 'NONE', #38723, 58.99999999999999289 ) ;
#4587 = ORIENTED_EDGE ( 'NONE', *, *, #41897, .T. ) ;
#4588 = AXIS2_PLACEMENT_3D ( 'NONE', #32830, #29804, #10127 ) ;
#4589 = DIRECTION ( 'NONE',  ( -1.717248367976097434E-17, 0.9999999999999998890, -2.483356757534101413E-17 ) ) ;
#4590 = CYLINDRICAL_SURFACE ( 'NONE', #21882, 51.99999999999999289 ) ;
#4591 = CARTESIAN_POINT ( 'NONE',  ( -40.58740609958903889, 31.00000000000000355, -31.12922691583434798 ) ) ;
#4592 = ORIENTED_EDGE ( 'NONE', *, *, #13945, .T. ) ;
#4593 = AXIS2_PLACEMENT_3D ( 'NONE', #38661, #21515, #8567 ) ;
#4595 = DIRECTION ( 'NONE',  ( -1.000000000000000000, -0.000000000000000000, 0.000000000000000000 ) ) ;
#4594 = CARTESIAN_POINT ( 'NONE',  ( 17.99999999999999645, -34.74871106919691499, 106.6808302961370600 ) ) ;
#4596 = AXIS2_PLACEMENT_3D ( 'NONE', #35027, #41987, #25251 ) ;
#4597 = CARTESIAN_POINT ( 'NONE',  ( -109.0695705685741785, -106.4195705685773135, 6.999999999999753975 ) ) ;
#4598 = ORIENTED_EDGE ( 'NONE', *, *, #13653, .T. ) ;
#4599 = VECTOR ( 'NONE', #4327, 1000.000000000000000 ) ;
#4600 = VECTOR ( 'NONE', #30152, 1000.000000000000000 ) ;
#4601 = DIRECTION ( 'NONE',  ( 1.000000000000000000, 1.836909530733573776E-16, 0.000000000000000000 ) ) ;
#4602 = CARTESIAN_POINT ( 'NONE',  ( 43.96541952717798551, 40.00000000000000000, 11.76906328551413239 ) ) ;
#4603 = ADVANCED_FACE ( 'NONE', ( #15675 ), #2111, .F. ) ;
#4604 = CARTESIAN_POINT ( 'NONE',  ( -30.31917247939794180, 40.00000000000000000, 52.30862930535366928 ) ) ;
#4605 = AXIS2_PLACEMENT_3D ( 'NONE', #34403, #28550, #30931 ) ;
#4606 = DIRECTION ( 'NONE',  ( 0.000000000000000000, 1.000000000000000000, 0.000000000000000000 ) ) ;
#4607 = CARTESIAN_POINT ( 'NONE',  ( 8.999999999999998224, 95.31344542257733110, 66.11616384574480776 ) ) ;
#4608 = CYLINDRICAL_SURFACE ( 'NONE', #15601, 10.49999999999999467 ) ;
#4609 = CARTESIAN_POINT ( 'NONE',  ( -16.73417733071809721, 31.00000000000000355, -12.82953315787133519 ) ) ;
#4610 = EDGE_CURVE ( 'NONE', #553, #19975, #42669, .T. ) ;
#4611 = ORIENTED_EDGE ( 'NONE', *, *, #34107, .T. ) ;
#4612 = CARTESIAN_POINT ( 'NONE',  ( -29.26739590608564967, 40.00000000000000000, 25.68069354617348665 ) ) ;
#4613 = ORIENTED_EDGE ( 'NONE', *, *, #10470, .F. ) ;
#4614 = FACE_OUTER_BOUND ( 'NONE', #42571, .T. ) ;
#4615 = CARTESIAN_POINT ( 'NONE',  ( 0.02448733951239481094, 4.877042772274728044, -3.751161874094022242 ) ) ;
#4616 = VERTEX_POINT ( 'NONE', #15473 ) ;
#4617 = CIRCLE ( 'NONE', #34583, 59.00000000000000000 ) ;
#4618 = DIRECTION ( 'NONE',  ( 1.000000000000000000, -3.469446951953615421E-17, 0.000000000000000000 ) ) ;
#4619 = CARTESIAN_POINT ( 'NONE',  ( -2.649999999999987477, 150.5000000000000284, 10.00000000000000000 ) ) ;
#4620 = ORIENTED_EDGE ( 'NONE', *, *, #15356, .T. ) ;
#4621 = DIRECTION ( 'NONE',  ( -1.000000000000000000, 0.000000000000000000, 0.000000000000000000 ) ) ;
#4622 = AXIS2_PLACEMENT_3D ( 'NONE', #20731, #3435, #43151 ) ;
#4623 = ORIENTED_EDGE ( 'NONE', *, *, #15965, .F. ) ;
#4624 = VECTOR ( 'NONE', #16100, 1000.000000000000000 ) ;
#4625 = VECTOR ( 'NONE', #9495, 1000.000000000000000 ) ;
#4626 = ORIENTED_EDGE ( 'NONE', *, *, #24773, .T. ) ;
#4627 = AXIS2_PLACEMENT_3D ( 'NONE', #20820, #34075, #6808 ) ;
#4628 = DIRECTION ( 'NONE',  ( 1.000000000000000000, 0.000000000000000000, 0.000000000000000000 ) ) ;
#4629 = CARTESIAN_POINT ( 'NONE',  ( 76.69346925293527306, 31.00000000000000000, 10.21457306974767398 ) ) ;
#4630 = VERTEX_POINT ( 'NONE', #5821 ) ;
#4631 = DIRECTION ( 'NONE',  ( 0.000000000000000000, 0.000000000000000000, -1.000000000000000000 ) ) ;
#4632 = MECHANICAL_DESIGN_GEOMETRIC_PRESENTATION_REPRESENTATION (  '', ( #442 ), #33228 ) ;
#4633 = LINE ( 'NONE', #17180, #37977 ) ;
#4634 = ORIENTED_EDGE ( 'NONE', *, *, #27292, .F. ) ;
#4635 = DIRECTION ( 'NONE',  ( -1.000000000000000000, 1.224646799147352714E-16, 0.000000000000000000 ) ) ;
#4636 = CIRCLE ( 'NONE', #22132, 58.99999999999999289 ) ;
#4637 = VERTEX_POINT ( 'NONE', #16103 ) ;
#4638 = CARTESIAN_POINT ( 'NONE',  ( 77.87745995356456774, 39.99999999999999289, 59.89653754212418590 ) ) ;
#4639 = EDGE_CURVE ( 'NONE', #1932, #33553, #31417, .T. ) ;
#4640 = CARTESIAN_POINT ( 'NONE',  ( -91.07534658258109062, 40.00000000000000711, 44.76935032130646874 ) ) ;
#4641 = EDGE_CURVE ( 'NONE', #6919, #6443, #6288, .T. ) ;
#4643 = DIRECTION ( 'NONE',  ( -1.000000000000000000, 0.000000000000000000, 0.000000000000000000 ) ) ;
#4642 = DIRECTION ( 'NONE',  ( 0.000000000000000000, 0.000000000000000000, 1.000000000000000000 ) ) ;
#4644 = CIRCLE ( 'NONE', #25586, 100.0000000000000000 ) ;
#4645 = DIRECTION ( 'NONE',  ( -1.000000000000000000, 1.084202172485505420E-16, 0.000000000000000000 ) ) ;
#4646 = DIRECTION ( 'NONE',  ( -1.000000000000000000, 0.000000000000000000, 0.000000000000000000 ) ) ;
#4647 = EDGE_LOOP ( 'NONE', ( #23298, #15444, #34694, #34797 ) ) ;
#4648 =( LENGTH_UNIT ( ) NAMED_UNIT ( * ) SI_UNIT ( .MILLI., .METRE. ) );
#4649 = DIRECTION ( 'NONE',  ( 1.000000000000000000, 0.000000000000000000, 0.000000000000000000 ) ) ;
#4650 = ORIENTED_EDGE ( 'NONE', *, *, #5217, .T. ) ;
#4651 = LINE ( 'NONE', #19711, #29647 ) ;
#4652 = CARTESIAN_POINT ( 'NONE',  ( -78.67873774631718220, 31.00000000000000711, 60.36924185307643143 ) ) ;
#4653 = FACE_OUTER_BOUND ( 'NONE', #17606, .T. ) ;
#4654 = CIRCLE ( 'NONE', #28364, 59.00000000000000000 ) ;
#4655 = ORIENTED_EDGE ( 'NONE', *, *, #2898, .F. ) ;
#4656 = VECTOR ( 'NONE', #29313, 1000.000000000000000 ) ;
#4657 = ADVANCED_FACE ( 'NONE', ( #39619 ), #23097, .F. ) ;
#4658 = CARTESIAN_POINT ( 'NONE',  ( -20.42974159057667194, 40.00000000000000000, -10.07157319949504526 ) ) ;
#4659 = VECTOR ( 'NONE', #14353, 1000.000000000000000 ) ;
#4660 = ORIENTED_EDGE ( 'NONE', *, *, #38394, .F. ) ;
#4661 = VECTOR ( 'NONE', #9289, 1000.000000000000000 ) ;
#4662 = VERTEX_POINT ( 'NONE', #12403 ) ;
#4663 = CARTESIAN_POINT ( 'NONE',  ( 17.99999999999999645, 12.43843445475471832, -111.5058645182328405 ) ) ;
#4664 = DIRECTION ( 'NONE',  ( 0.000000000000000000, 0.000000000000000000, 1.000000000000000000 ) ) ;
#4665 = CARTESIAN_POINT ( 'NONE',  ( 0.000000000000000000, -47.32430374665916162, -21.55018039121577544 ) ) ;
#4666 = CIRCLE ( 'NONE', #1169, 4.000000000000000000 ) ;
#4667 = DIRECTION ( 'NONE',  ( -1.000000000000000000, 0.000000000000000000, 0.000000000000000000 ) ) ;
#4668 = AXIS2_PLACEMENT_3D ( 'NONE', #40585, #22998, #36241 ) ;
#4669 = AXIS2_PLACEMENT_3D ( 'NONE', #674, #19565, #20006 ) ;
#4670 = EDGE_CURVE ( 'NONE', #37795, #12005, #36342, .T. ) ;
#4671 = ORIENTED_EDGE ( 'NONE', *, *, #23903, .T. ) ;
#4672 = FACE_OUTER_BOUND ( 'NONE', #35090, .T. ) ;
#4673 = ORIENTED_EDGE ( 'NONE', *, *, #5303, .F. ) ;
#4674 = LINE ( 'NONE', #14296, #37485 ) ;
#4675 = FACE_OUTER_BOUND ( 'NONE', #35556, .T. ) ;
#4676 = EDGE_CURVE ( 'NONE', #24669, #20680, #4931, .T. ) ;
#4677 = DIRECTION ( 'NONE',  ( 0.000000000000000000, -0.8660254037844390407, -0.4999999999999993339 ) ) ;
#4678 = CARTESIAN_POINT ( 'NONE',  ( -31.74999999999995737, 3.061616997868383634E-16, -2.500000000000000444 ) ) ;
#4679 = ORIENTED_EDGE ( 'NONE', *, *, #7553, .F. ) ;
#4680 = ORIENTED_EDGE ( 'NONE', *, *, #7946, .T. ) ;
#4681 = CARTESIAN_POINT ( 'NONE',  ( 17.99999999999999645, 34.03109950475727175, 115.5957406979051285 ) ) ;
#4682 = DIRECTION ( 'NONE',  ( -0.000000000000000000, -0.000000000000000000, 1.000000000000000000 ) ) ;
#4683 = ORIENTED_EDGE ( 'NONE', *, *, #30969, .T. ) ;
#4685 = ORIENTED_EDGE ( 'NONE', *, *, #30864, .F. ) ;
#4684 = DIRECTION ( 'NONE',  ( 0.000000000000000000, 0.000000000000000000, 1.000000000000000000 ) ) ;
#4686 = CARTESIAN_POINT ( 'NONE',  ( -37.12595630542501368, 31.00000000000000355, 18.22532657727797556 ) ) ;
#4687 = DIRECTION ( 'NONE',  ( -1.000000000000000000, 0.000000000000000000, 0.000000000000000000 ) ) ;
#4688 = AXIS2_PLACEMENT_3D ( 'NONE', #26736, #23915, #36969 ) ;
#4689 = AXIS2_PLACEMENT_3D ( 'NONE', #17767, #27137, #37575 ) ;
#4691 = SURFACE_STYLE_FILL_AREA ( #14548 ) ;
#4690 = CARTESIAN_POINT ( 'NONE',  ( 18.00000000000000355, 0.000000000000000000, 0.000000000000000000 ) ) ;
#4692 = ORIENTED_EDGE ( 'NONE', *, *, #32430, .F. ) ;
#4693 = CARTESIAN_POINT ( 'NONE',  ( 0.000000000000000000, 44.47301969247445186, 16.68249143361925135 ) ) ;
#4694 = CARTESIAN_POINT ( 'NONE',  ( -45.90931453312558119, 40.00000000000000000, 40.13788153756827626 ) ) ;
#4695 = AXIS2_PLACEMENT_3D ( 'NONE', #2080, #18514, #39155 ) ;
#4696 = AXIS2_PLACEMENT_3D ( 'NONE', #11904, #12114, #7953 ) ;
#4697 = EDGE_CURVE ( 'NONE', #1617, #35040, #10500, .T. ) ;
#4698 = ADVANCED_FACE ( 'NONE', ( #25727 ), #29403, .F. ) ;
#4699 = AXIS2_PLACEMENT_3D ( 'NONE', #10313, #23225, #7236 ) ;
#4700 = DIRECTION ( 'NONE',  ( -1.000000000000000000, 0.000000000000000000, 0.000000000000000000 ) ) ;
#4701 = EDGE_CURVE ( 'NONE', #12909, #33268, #21703, .T. ) ;
#4702 = EDGE_CURVE ( 'NONE', #23443, #35253, #14011, .T. ) ;
#4703 = EDGE_CURVE ( 'NONE', #17388, #3320, #9308, .T. ) ;
#4704 = DIRECTION ( 'NONE',  ( -1.000000000000000000, -0.000000000000000000, -0.000000000000000000 ) ) ;
#4705 = VERTEX_POINT ( 'NONE', #9098 ) ;
#4706 = CYLINDRICAL_SURFACE ( 'NONE', #34918, 59.00000000000000000 ) ;
#4707 = ORIENTED_EDGE ( 'NONE', *, *, #8268, .T. ) ;
#4708 =( LENGTH_UNIT ( ) NAMED_UNIT ( * ) SI_UNIT ( .MILLI., .METRE. ) );
#4709 = DIRECTION ( 'NONE',  ( 0.000000000000000000, -0.3641605752528294104, 0.9313361774523356562 ) ) ;
#4710 = LINE ( 'NONE', #14776, #40807 ) ;
#4711 = VECTOR ( 'NONE', #38762, 1000.000000000000000 ) ;
#4712 = CARTESIAN_POINT ( 'NONE',  ( -15.01009539198478748, 31.00000000000000355, 56.06562763604418365 ) ) ;
#4713 = FACE_OUTER_BOUND ( 'NONE', #10652, .T. ) ;
#4714 = VERTEX_POINT ( 'NONE', #13047 ) ;
#4715 = CARTESIAN_POINT ( 'NONE',  ( -10.00000000000000000, 0.000000000000000000, 0.000000000000000000 ) ) ;
#4716 = CARTESIAN_POINT ( 'NONE',  ( 30.80114556864472775, 40.00000000000000000, -15.19345985420777190 ) ) ;
#4717 = VERTEX_POINT ( 'NONE', #2312 ) ;
#4718 = DIRECTION ( 'NONE',  ( -1.000000000000000000, -0.000000000000000000, 0.000000000000000000 ) ) ;
#4719 = CARTESIAN_POINT ( 'NONE',  ( 8.999999999999998224, -48.55277268144396174, 105.3500273609078306 ) ) ;
#4720 = CIRCLE ( 'NONE', #33280, 59.00000000000001421 ) ;
#4721 = CARTESIAN_POINT ( 'NONE',  ( 42.86165537668586722, 31.00000000000000355, -73.99543480067944756 ) ) ;
#4722 = CARTESIAN_POINT ( 'NONE',  ( 87.09251733236553150, 39.99999999999999289, 5.815661930448016825 ) ) ;
#4723 = CYLINDRICAL_SURFACE ( 'NONE', #15374, 13.59999999999999964 ) ;
#4724 = VECTOR ( 'NONE', #10466, 1000.000000000000000 ) ;
#4725 = EDGE_CURVE ( 'NONE', #35938, #8548, #35495, .T. ) ;
#4726 = ORIENTED_EDGE ( 'NONE', *, *, #19657, .F. ) ;
#4727 = DIRECTION ( 'NONE',  ( -3.009274222672345096E-17, -1.000000000000000000, 2.455023325076454960E-18 ) ) ;
#4728 = AXIS2_PLACEMENT_3D ( 'NONE', #3279, #13579, #17078 ) ;
#4729 = EDGE_LOOP ( 'NONE', ( #15050, #32759, #17049, #31835 ) ) ;
#4730 = AXIS2_PLACEMENT_3D ( 'NONE', #15806, #15183, #22166 ) ;
#4731 =( NAMED_UNIT ( * ) PLANE_ANGLE_UNIT ( ) SI_UNIT ( $, .RADIAN. ) );
#4732 = DIRECTION ( 'NONE',  ( 1.000000000000000000, 0.000000000000000000, -6.546126324440832913E-16 ) ) ;
#4733 = EDGE_CURVE ( 'NONE', #37469, #10305, #2109, .T. ) ;
#4734 = VECTOR ( 'NONE', #26636, 1000.000000000000000 ) ;
#4736 = ORIENTED_EDGE ( 'NONE', *, *, #3057, .T. ) ;
#4735 = DIRECTION ( 'NONE',  ( 0.000000000000000000, 0.9048270524660205760, -0.4257792915650702170 ) ) ;
#4737 = CARTESIAN_POINT ( 'NONE',  ( 0.000000000000000000, -6.854627147197943415, -115.7972974066014018 ) ) ;
#4738 = ORIENTED_EDGE ( 'NONE', *, *, #35387, .F. ) ;
#4739 = CARTESIAN_POINT ( 'NONE',  ( -0.2142857142857142738, -10.49781318335647917, 0.000000000000000000 ) ) ;
#4740 = CARTESIAN_POINT ( 'NONE',  ( -6.054110834496889026, 40.00000000000000000, -92.39583333400220511 ) ) ;
#4741 = DIRECTION ( 'NONE',  ( 1.000000000000000000, 0.000000000000000000, 0.000000000000000000 ) ) ;
#4742 =( REPRESENTATION_RELATIONSHIP ('NONE','NONE', #330, #37437 ) REPRESENTATION_RELATIONSHIP_WITH_TRANSFORMATION ( #25308 )SHAPE_REPRESENTATION_RELATIONSHIP( ) );
#4743 = VECTOR ( 'NONE', #37203, 1000.000000000000000 ) ;
#4744 = ORIENTED_EDGE ( 'NONE', *, *, #40432, .F. ) ;
#4745 = DIRECTION ( 'NONE',  ( 0.000000000000000000, 1.000000000000000000, 0.000000000000000000 ) ) ;
#4746 = CYLINDRICAL_SURFACE ( 'NONE', #7165, 2.500000000000002665 ) ;
#4748 = DIRECTION ( 'NONE',  ( -1.000000000000000000, 0.000000000000000000, 0.000000000000000000 ) ) ;
#4747 = DIRECTION ( 'NONE',  ( -3.996523416598930318E-16, 2.658563593772947863E-15, 1.000000000000000000 ) ) ;
#4749 = ORIENTED_EDGE ( 'NONE', *, *, #10761, .F. ) ;
#4750 = CYLINDRICAL_SURFACE ( 'NONE', #35144, 20.00000000000000355 ) ;
#4751 = ORIENTED_EDGE ( 'NONE', *, *, #7351, .F. ) ;
#4752 = CARTESIAN_POINT ( 'NONE',  ( -2.000000000000006661, 3.464101615137750834, 0.000000000000000000 ) ) ;
#4753 = CARTESIAN_POINT ( 'NONE',  ( 7.507699080470448649, 40.00000000000000000, 28.16210111025598906 ) ) ;
#4754 = CYLINDRICAL_SURFACE ( 'NONE', #21625, 36.00000000000000000 ) ;
#4756 = EDGE_CURVE ( 'NONE', #6092, #17062, #9782, .T. ) ;
#4755 = CIRCLE ( 'NONE', #38872, 59.00000000000000711 ) ;
#4757 = VECTOR ( 'NONE', #9820, 1000.000000000000000 ) ;
#4758 = CARTESIAN_POINT ( 'NONE',  ( 0.000000000000000000, 0.000000000000000000, 0.000000000000000000 ) ) ;
#4759 = EDGE_CURVE ( 'NONE', #20305, #7155, #40647, .T. ) ;
#4760 = EDGE_CURVE ( 'NONE', #13499, #10354, #39825, .T. ) ;
#4761 = DIRECTION ( 'NONE',  ( -1.000000000000000000, 0.000000000000000000, 0.000000000000000000 ) ) ;
#4762 = EDGE_LOOP ( 'NONE', ( #26073, #32079, #20063, #25247 ) ) ;
#4764 = DIRECTION ( 'NONE',  ( 1.000000000000000000, 0.000000000000000000, 0.000000000000000000 ) ) ;
#4763 = DIRECTION ( 'NONE',  ( -1.000000000000000000, -0.000000000000000000, -0.000000000000000000 ) ) ;
#4765 = AXIS2_PLACEMENT_3D ( 'NONE', #39578, #13222, #16723 ) ;
#4766 = EDGE_CURVE ( 'NONE', #3059, #33656, #26551, .T. ) ;
#4767 = ORIENTED_EDGE ( 'NONE', *, *, #37855, .T. ) ;
#4768 = AXIS2_PLACEMENT_3D ( 'NONE', #14274, #21717, #17573 ) ;
#4769 = AXIS2_PLACEMENT_3D ( 'NONE', #29327, #9677, #9879 ) ;
#4770 = CARTESIAN_POINT ( 'NONE',  ( -103.7695705685756025, 106.4195705685752529, 6.999999999999998224 ) ) ;
#4771 = LINE ( 'NONE', #8033, #35182 ) ;
#4772 = CARTESIAN_POINT ( 'NONE',  ( -26.76192867387533170, 31.00000000000000355, -15.44647709060871321 ) ) ;
#4773 = ORIENTED_EDGE ( 'NONE', *, *, #13432, .F. ) ;
#4774 = DIRECTION ( 'NONE',  ( 0.000000000000000000, 0.000000000000000000, 1.000000000000000000 ) ) ;
#4775 = VECTOR ( 'NONE', #27728, 1000.000000000000000 ) ;
#4776 = FACE_BOUND ( 'NONE', #41078, .T. ) ;
#4777 = CONTEXT_DEPENDENT_SHAPE_REPRESENTATION ( #23432, #18013 ) ;
#4778 = CARTESIAN_POINT ( 'NONE',  ( 0.000000000000000000, 0.000000000000000000, 0.000000000000000000 ) ) ;
#4779 = CARTESIAN_POINT ( 'NONE',  ( 84.24376206367318787, 31.00000000000000000, -11.10575268747775901 ) ) ;
#4780 = ORIENTED_EDGE ( 'NONE', *, *, #24395, .F. ) ;
#4781 = CARTESIAN_POINT ( 'NONE',  ( 14.32751628686350287, 31.00000000000000355, -53.13354968560084757 ) ) ;
#4782 = CARTESIAN_POINT ( 'NONE',  ( 28.03234818517180216, 40.00000000000000000, 82.53419278363811884 ) ) ;
#4783 = ORIENTED_EDGE ( 'NONE', *, *, #37907, .F. ) ;
#4784 = DIRECTION ( 'NONE',  ( -1.000000000000000000, 0.000000000000000000, 0.000000000000000000 ) ) ;
#4785 = DIRECTION ( 'NONE',  ( 1.000000000000000000, -3.469446951953611107E-17, 0.000000000000000000 ) ) ;
#4786 = CARTESIAN_POINT ( 'NONE',  ( 17.99999999999999645, 86.84764344322962870, 76.89919913989776035 ) ) ;
#4787 = AXIS2_PLACEMENT_3D ( 'NONE', #41426, #24918, #17711 ) ;
#4788 = CIRCLE ( 'NONE', #8962, 20.00000000000000000 ) ;
#4790 = EDGE_LOOP ( 'NONE', ( #15274, #12760, #15288, #9893 ) ) ;
#4789 = CARTESIAN_POINT ( 'NONE',  ( 9.000000000000001776, 43.55304910509446614, -28.41006711799937889 ) ) ;
#4791 = CARTESIAN_POINT ( 'NONE',  ( 0.000000000000000000, -35.72777019205738469, 106.3569410558016273 ) ) ;
#4792 = CARTESIAN_POINT ( 'NONE',  ( 0.000000000000000000, -35.89808275599447285, 2.706964063997105541 ) ) ;
#4793 = VECTOR ( 'NONE', #17597, 1000.000000000000000 ) ;
#4794 = EDGE_LOOP ( 'NONE', ( #36301, #9854, #30019, #3969 ) ) ;
#4795 = CARTESIAN_POINT ( 'NONE',  ( 16.30650823456882748, 40.00000000000000000, -60.90571087954511142 ) ) ;
#4796 = CYLINDRICAL_SURFACE ( 'NONE', #18080, 20.00000000000000711 ) ;
#4797 = ORIENTED_EDGE ( 'NONE', *, *, #39627, .T. ) ;
#4798 = DIRECTION ( 'NONE',  ( 0.000000000000000000, 0.7980172272802362743, 0.6026346363792606242 ) ) ;
#4799 = CARTESIAN_POINT ( 'NONE',  ( -100.0000000000000568, 40.00000000000000000, 2.687954026026062593E-12 ) ) ;
#4800 = ORIENTED_EDGE ( 'NONE', *, *, #23694, .F. ) ;
#4801 = DIRECTION ( 'NONE',  ( 0.000000000000000000, 0.000000000000000000, 1.000000000000000000 ) ) ;
#4802 = ORIENTED_EDGE ( 'NONE', *, *, #16393, .F. ) ;
#4803 = CARTESIAN_POINT ( 'NONE',  ( 17.99999999999999645, 13.57797752207971520, -33.34124362422460308 ) ) ;
#4804 = ORIENTED_EDGE ( 'NONE', *, *, #28043, .T. ) ;
#4805 = CYLINDRICAL_SURFACE ( 'NONE', #4908, 59.00000000000000000 ) ;
#4806 = CARTESIAN_POINT ( 'NONE',  ( 0.000000000000000000, -120.2856157092987388, 7.201503623196430226 ) ) ;
#4807 = VERTEX_POINT ( 'NONE', #43112 ) ;
#4808 = PLANE ( 'NONE',  #31670 ) ;
#4809 = ADVANCED_FACE ( 'NONE', ( #20681 ), #27410, .F. ) ;
#4810 = DIRECTION ( 'NONE',  ( -1.000000000000000000, -0.000000000000000000, 0.000000000000000000 ) ) ;
#4811 = ORIENTED_EDGE ( 'NONE', *, *, #19772, .F. ) ;
#4812 = CYLINDRICAL_SURFACE ( 'NONE', #30819, 116.0000000000000000 ) ;
#4813 = EDGE_CURVE ( 'NONE', #40202, #31882, #18217, .T. ) ;
#4814 = DIRECTION ( 'NONE',  ( -1.000000000000000000, 0.000000000000000000, 0.000000000000000000 ) ) ;
#4815 = CIRCLE ( 'NONE', #10390, 51.99999999999999289 ) ;
#4816 = ORIENTED_EDGE ( 'NONE', *, *, #22573, .T. ) ;
#4817 = CONICAL_SURFACE ( 'NONE', #31987, 2.059999999999998721, 0.9599310885968738161 ) ;
#4818 = CARTESIAN_POINT ( 'NONE',  ( 0.000000000000000000, -11.65176648921111635, 115.4133282497342066 ) ) ;
#4819 = CARTESIAN_POINT ( 'NONE',  ( 17.99999999999999645, 63.24564713401931471, -102.5693868539688651 ) ) ;
#4820 = AXIS2_PLACEMENT_3D ( 'NONE', #18845, #6120, #29062 ) ;
#4821 = EDGE_CURVE ( 'NONE', #36379, #34535, #34164, .T. ) ;
#4822 = APPLICATION_PROTOCOL_DEFINITION ( 'draft international standard', 'automotive_design', 1998, #32827 ) ;
#4823 = LINE ( 'NONE', #24710, #28856 ) ;
#4824 = CARTESIAN_POINT ( 'NONE',  ( 51.69409438402072965, 31.00000000000000355, -17.56033928829605273 ) ) ;
#4825 = VERTEX_POINT ( 'NONE', #554 ) ;
#4827 = CARTESIAN_POINT ( 'NONE',  ( 0.000000000000000000, 110.0562500189205224, -49.07252625220001363 ) ) ;
#4826 = DIRECTION ( 'NONE',  ( 1.058513553088275437E-16, 1.000000000000000000, -8.813324511995299047E-17 ) ) ;
#4828 = EDGE_CURVE ( 'NONE', #32170, #30953, #20041, .T. ) ;
#4829 = DIRECTION ( 'NONE',  ( -1.000000000000000000, 0.000000000000000000, -0.000000000000000000 ) ) ;
#4830 = ORIENTED_EDGE ( 'NONE', *, *, #39351, .T. ) ;
#4831 = CARTESIAN_POINT ( 'NONE',  ( 0.000000000000000000, 0.000000000000000000, -6.000000000000000000 ) ) ;
#4832 = CARTESIAN_POINT ( 'NONE',  ( 54.43714469963884284, 40.00000000000000000, -7.178810421751046000 ) ) ;
#4833 = CARTESIAN_POINT ( 'NONE',  ( 3.791180027291366272, 40.00000000000000000, 59.39995347152935778 ) ) ;
#4834 = CARTESIAN_POINT ( 'NONE',  ( 18.00000000000000355, 7.162210897276454880, -51.50439529848820541 ) ) ;
#4835 = DIRECTION ( 'NONE',  ( 0.000000000000000000, 0.000000000000000000, 1.000000000000000000 ) ) ;
#4836 = DIRECTION ( 'NONE',  ( -1.000000000000000000, 0.000000000000000000, 0.000000000000000000 ) ) ;
#4837 = CARTESIAN_POINT ( 'NONE',  ( -5.732510072307491988, 31.00000000000000355, -21.37570426403446078 ) ) ;
#4838 = ORIENTED_EDGE ( 'NONE', *, *, #12506, .F. ) ;
#4839 = CARTESIAN_POINT ( 'NONE',  ( -2.127120017302697619, 40.00000000000000000, -32.39583333539214038 ) ) ;
#4840 = ORIENTED_EDGE ( 'NONE', *, *, #33144, .F. ) ;
#4841 = CYLINDRICAL_SURFACE ( 'NONE', #30622, 51.99999999999999289 ) ;
#4842 = CARTESIAN_POINT ( 'NONE',  ( -3.522875095019672109, 2.820352903225427532, -3.598441714920591394 ) ) ;
#4843 = VERTEX_POINT ( 'NONE', #17411 ) ;
#4844 = AXIS2_PLACEMENT_3D ( 'NONE', #2245, #6186, #32373 ) ;
#4845 = AXIS2_PLACEMENT_3D ( 'NONE', #22644, #12800, #32643 ) ;
#4846 = DIRECTION ( 'NONE',  ( 0.000000000000000000, 0.000000000000000000, -1.000000000000000000 ) ) ;
#4847 = CARTESIAN_POINT ( 'NONE',  ( -102.0670434220619427, -12.05525454449572109, 139.0496534599708980 ) ) ;
#4848 = EDGE_LOOP ( 'NONE', ( #34423, #26540, #39063, #13815 ) ) ;
#4849 = DIRECTION ( 'NONE',  ( 1.000000000000000000, 0.000000000000000000, 0.000000000000000000 ) ) ;
#4850 = VERTEX_POINT ( 'NONE', #10397 ) ;
#4851 = CIRCLE ( 'NONE', #38198, 4.000000000000000000 ) ;
#4852 = ORIENTED_EDGE ( 'NONE', *, *, #6733, .F. ) ;
#4853 = CARTESIAN_POINT ( 'NONE',  ( 17.99999999999999645, -32.49609705003693705, -15.49205204337308217 ) ) ;
#4854 = CARTESIAN_POINT ( 'NONE',  ( -65.32047834223114080, 31.00000000000000711, -32.32491738443057017 ) ) ;
#4855 = ORIENTED_EDGE ( 'NONE', *, *, #2254, .T. ) ;
#4856 = CARTESIAN_POINT ( 'NONE',  ( -4.000000000000000000, 1.677772373332757194, -3.535253723897187506 ) ) ;
#4857 = EDGE_CURVE ( 'NONE', #19972, #30408, #24464, .T. ) ;
#4858 = DIRECTION ( 'NONE',  ( 0.000000000000000000, -0.2113826236296314776, 0.9774033898178651203 ) ) ;
#4859 = VERTEX_POINT ( 'NONE', #10831 ) ;
#4860 = DIRECTION ( 'NONE',  ( 1.000000000000000000, 0.000000000000000000, 0.000000000000000000 ) ) ;
#4861 = VERTEX_POINT ( 'NONE', #30049 ) ;
#4862 = CARTESIAN_POINT ( 'NONE',  ( 64.90225467577229779, 39.99999999999999289, 74.17428024387139374 ) ) ;
#4863 = CARTESIAN_POINT ( 'NONE',  ( 1.622176940739286310, 31.00000000000000355, -24.60292901074088334 ) ) ;
#4865 = DIRECTION ( 'NONE',  ( -0.000000000000000000, 0.000000000000000000, 1.000000000000000000 ) ) ;
#4864 = DIRECTION ( 'NONE',  ( -1.000000000000000000, -0.000000000000000000, -0.000000000000000000 ) ) ;
#4866 = DIRECTION ( 'NONE',  ( -1.000000000000000000, -0.000000000000000000, 0.000000000000000000 ) ) ;
#4867 = CARTESIAN_POINT ( 'NONE',  ( 0.000000000000000000, 0.000000000000000000, -25.00000000000000000 ) ) ;
#4868 = EDGE_LOOP ( 'NONE', ( #42384, #32946, #18201, #5 ) ) ;
#4869 = EDGE_CURVE ( 'NONE', #37579, #2622, #14121, .T. ) ;
#4870 =( NAMED_UNIT ( * ) SI_UNIT ( $, .STERADIAN. ) SOLID_ANGLE_UNIT ( ) );
#4871 = CARTESIAN_POINT ( 'NONE',  ( 17.99999999999999645, 0.000000000000000000, 0.000000000000000000 ) ) ;
#4872 = VECTOR ( 'NONE', #25843, 1000.000000000000000 ) ;
#4873 = ORIENTED_EDGE ( 'NONE', *, *, #35271, .F. ) ;
#4874 = LINE ( 'NONE', #41071, #42127 ) ;
#4875 = AXIS2_PLACEMENT_3D ( 'NONE', #30496, #3617, #16987 ) ;
#4876 = EDGE_CURVE ( 'NONE', #14923, #31429, #40441, .T. ) ;
#4877 = CARTESIAN_POINT ( 'NONE',  ( 46.76839422403993751, 31.00000000000000000, -81.00140361174831583 ) ) ;
#4878 = CIRCLE ( 'NONE', #41104, 47.49900000000000233 ) ;
#4879 = LINE ( 'NONE', #18240, #16305 ) ;
#4880 = ORIENTED_EDGE ( 'NONE', *, *, #2094, .T. ) ;
#4881 = CARTESIAN_POINT ( 'NONE',  ( -29.88476798293163128, 40.00000000000000000, 10.10044382456043266 ) ) ;
#4882 = ORIENTED_EDGE ( 'NONE', *, *, #38246, .T. ) ;
#4883 = EDGE_LOOP ( 'NONE', ( #22935, #20869, #39550, #28800 ) ) ;
#4884 = DIRECTION ( 'NONE',  ( -1.000000000000000000, 0.000000000000000000, 0.000000000000000000 ) ) ;
#4885 = DIRECTION ( 'NONE',  ( -1.000000000000000000, 0.000000000000000000, 0.000000000000000000 ) ) ;
#4886 = CARTESIAN_POINT ( 'NONE',  ( 0.000000000000000000, 101.1403355683146117, 56.80345518653518866 ) ) ;
#4887 = CYLINDRICAL_SURFACE ( 'NONE', #3723, 59.00000000000000000 ) ;
#4888 = EDGE_CURVE ( 'NONE', #35775, #21277, #36961, .T. ) ;
#4889 = ORIENTED_EDGE ( 'NONE', *, *, #22311, .T. ) ;
#4890 = FACE_OUTER_BOUND ( 'NONE', #30091, .T. ) ;
#4891 = ORIENTED_EDGE ( 'NONE', *, *, #33750, .T. ) ;
#4892 = LINE ( 'NONE', #34994, #4793 ) ;
#4893 = EDGE_CURVE ( 'NONE', #2622, #5158, #728, .T. ) ;
#4894 = CARTESIAN_POINT ( 'NONE',  ( -2.100000000000000089, 2.571758278209441957E-16, -0.2800830152838844622 ) ) ;
#4895 = EDGE_CURVE ( 'NONE', #24356, #40010, #33478, .T. ) ;
#4896 = CARTESIAN_POINT ( 'NONE',  ( 0.000000000000000000, 5.492704054966705662, 115.8698847939556344 ) ) ;
#4897 = DIRECTION ( 'NONE',  ( 0.000000000000000000, 0.000000000000000000, 1.000000000000000000 ) ) ;
#4898 = ORIENTED_EDGE ( 'NONE', *, *, #22087, .T. ) ;
#4899 = ORIENTED_EDGE ( 'NONE', *, *, #39655, .T. ) ;
#4900 = DIRECTION ( 'NONE',  ( 0.000000000000000000, 0.000000000000000000, 1.000000000000000000 ) ) ;
#4901 = CARTESIAN_POINT ( 'NONE',  ( 17.99999999999999645, 0.000000000000000000, 0.000000000000000000 ) ) ;
#4902 = CIRCLE ( 'NONE', #41097, 59.00000000000000000 ) ;
#4903 = ORIENTED_EDGE ( 'NONE', *, *, #30581, .F. ) ;
#4905 = ORIENTED_EDGE ( 'NONE', *, *, #14002, .T. ) ;
#4904 = DIRECTION ( 'NONE',  ( 1.000000000000000000, 0.000000000000000000, 0.000000000000000000 ) ) ;
#4906 = VECTOR ( 'NONE', #4687, 1000.000000000000000 ) ;
#4907 = CARTESIAN_POINT ( 'NONE',  ( 22.78600399167716262, 31.00000000000000355, -39.30137845375363526 ) ) ;
#4908 = AXIS2_PLACEMENT_3D ( 'NONE', #8296, #18166, #34692 ) ;
#4909 = LINE ( 'NONE', #1844, #4906 ) ;
#4910 = VECTOR ( 'NONE', #21425, 1000.000000000000000 ) ;
#4911 = EDGE_CURVE ( 'NONE', #39320, #41075, #14706, .T. ) ;
#4913 = SURFACE_SIDE_STYLE ('',( #4691 ) ) ;
#4912 = DIRECTION ( 'NONE',  ( -0.000000000000000000, -0.000000000000000000, 1.000000000000000000 ) ) ;
#4914 = VERTEX_POINT ( 'NONE', #102 ) ;
#4915 = CARTESIAN_POINT ( 'NONE',  ( 9.000000000000001776, 30.03615769709733740, 42.44795908868999135 ) ) ;
#4916 = CARTESIAN_POINT ( 'NONE',  ( 29.31577600748121881, 40.00000000000000000, 50.95836110724019363 ) ) ;
#4917 = CARTESIAN_POINT ( 'NONE',  ( 18.00000000000000355, 29.60891106212838508, -37.14118181634735549 ) ) ;
#4918 = FACE_OUTER_BOUND ( 'NONE', #19978, .T. ) ;
#4919 = EDGE_LOOP ( 'NONE', ( #15446, #35529, #22324, #19970 ) ) ;
#4920 = DIRECTION ( 'NONE',  ( 1.000000000000000000, 0.000000000000000000, 0.000000000000000000 ) ) ;
#4921 = ORIENTED_EDGE ( 'NONE', *, *, #8792, .T. ) ;
#4922 = EDGE_CURVE ( 'NONE', #16072, #3331, #16800, .T. ) ;
#4923 = DIRECTION ( 'NONE',  ( 1.000000000000000000, 0.000000000000000000, 0.000000000000000000 ) ) ;
#4924 = CARTESIAN_POINT ( 'NONE',  ( 0.000000000000000000, 0.7408941433508176022, 0.000000000000000000 ) ) ;
#4925 = CIRCLE ( 'NONE', #41825, 36.00000000000000000 ) ;
#4926 = EDGE_CURVE ( 'NONE', #23473, #25436, #25855, .T. ) ;
#4927 = CARTESIAN_POINT ( 'NONE',  ( 50.84997085137049311, 31.00000000000000000, -39.01959913718239648 ) ) ;
#4928 = DIRECTION ( 'NONE',  ( -1.000000000000000000, 0.000000000000000000, -0.000000000000000000 ) ) ;
#4929 = ORIENTED_EDGE ( 'NONE', *, *, #15849, .T. ) ;
#4930 = EDGE_CURVE ( 'NONE', #39721, #40482, #41126, .T. ) ;
#4931 = CIRCLE ( 'NONE', #11903, 2.500000000000000444 ) ;
#4932 = FACE_OUTER_BOUND ( 'NONE', #30822, .T. ) ;
#4933 = CIRCLE ( 'NONE', #29332, 20.00000000000000711 ) ;
#4934 = AXIS2_PLACEMENT_3D ( 'NONE', #16468, #43043, #7252 ) ;
#4935 = EDGE_LOOP ( 'NONE', ( #40444, #11667, #32012, #9538 ) ) ;
#4936 = DIRECTION ( 'NONE',  ( -1.000000000000000000, 0.000000000000000000, -0.000000000000000000 ) ) ;
#4937 = CIRCLE ( 'NONE', #13928, 20.00000000000000355 ) ;
#4938 = CARTESIAN_POINT ( 'NONE',  ( 17.99999999999999645, -63.55543939553702160, -97.03971415477388973 ) ) ;
#4939 = CARTESIAN_POINT ( 'NONE',  ( 22.98560153734151257, 31.00000000000000355, 86.26083236265422727 ) ) ;
#4940 = CARTESIAN_POINT ( 'NONE',  ( 44.33290732825513203, 40.00000000000000000, 77.00207852759155003 ) ) ;
#4941 = CIRCLE ( 'NONE', #26528, 130.0000000000000000 ) ;
#4942 = CARTESIAN_POINT ( 'NONE',  ( 1.798435537469519230E-14, -1.196353617197826191E-13, -44.99999999999999289 ) ) ;
#4943 = ORIENTED_EDGE ( 'NONE', *, *, #25789, .T. ) ;
#4944 = DIRECTION ( 'NONE',  ( 0.000000000000000000, 0.5076658003388409002, -0.8615540813938056264 ) ) ;
#4945 = ORIENTED_EDGE ( 'NONE', *, *, #15192, .T. ) ;
#4946 = CYLINDRICAL_SURFACE ( 'NONE', #17928, 20.00000000000000355 ) ;
#4947 = CYLINDRICAL_SURFACE ( 'NONE', #6648, 58.99999999999998579 ) ;
#4948 = ADVANCED_FACE ( 'NONE', ( #36995 ), #7108, .F. ) ;
#4949 = PRODUCT_RELATED_PRODUCT_CATEGORY ( 'part', '', ( #9892 ) ) ;
#4951 = ORIENTED_EDGE ( 'NONE', *, *, #36443, .F. ) ;
#4950 = CARTESIAN_POINT ( 'NONE',  ( 18.00000000000000355, 37.91532898920922889, 28.61088654061651937 ) ) ;
#4952 = LINE ( 'NONE', #34187, #5202 ) ;
#4953 = VERTEX_POINT ( 'NONE', #34812 ) ;
#4954 = CARTESIAN_POINT ( 'NONE',  ( 1.567478505476135000E-15, 4.618802153517012954, -3.504269196027527844 ) ) ;
#4955 = CARTESIAN_POINT ( 'NONE',  ( 6.054110834496887250, 40.00000000000000000, -92.60416666599778068 ) ) ;
#4956 = CARTESIAN_POINT ( 'NONE',  ( 17.99999999999999645, 6.007673836298523362, -35.49518073029991427 ) ) ;
#4957 = ORIENTED_EDGE ( 'NONE', *, *, #31037, .F. ) ;
#4958 = FACE_OUTER_BOUND ( 'NONE', #37130, .T. ) ;
#4959 = DIRECTION ( 'NONE',  ( 0.000000000000000000, -1.224646799147343346E-16, 1.000000000000000000 ) ) ;
#4960 = CIRCLE ( 'NONE', #11235, 24.99999999999998934 ) ;
#4961 = EDGE_CURVE ( 'NONE', #29560, #384, #6320, .T. ) ;
#4963 = CYLINDRICAL_SURFACE ( 'NONE', #366, 59.00000000000000000 ) ;
#4962 = LINE ( 'NONE', #8449, #30022 ) ;
#4964 = ORIENTED_EDGE ( 'NONE', *, *, #31671, .T. ) ;
#4965 = DIRECTION ( 'NONE',  ( -1.000000000000000000, 0.000000000000000000, 0.000000000000000000 ) ) ;
#4967 = ORIENTED_EDGE ( 'NONE', *, *, #5545, .T. ) ;
#4966 = AXIS2_PLACEMENT_3D ( 'NONE', #14316, #24376, #7750 ) ;
#4968 = CARTESIAN_POINT ( 'NONE',  ( 0.000000000000000000, 29.03409033315599075, -12.21509719675360373 ) ) ;
#4969 = CARTESIAN_POINT ( 'NONE',  ( 11.33656872182470643, 40.00000000000000000, -33.21392199183605953 ) ) ;
#4970 = DIRECTION ( 'NONE',  ( 1.000000000000000000, -1.373900992973642066E-15, -3.979293995072266947E-16 ) ) ;
#4971 = CIRCLE ( 'NONE', #21054, 59.00000000000000000 ) ;
#4972 = CARTESIAN_POINT ( 'NONE',  ( 17.99999999999999645, 31.80866420683995699, -2.997093558040963224 ) ) ;
#4973 = CIRCLE ( 'NONE', #7043, 2.649999999999973266 ) ;
#4974 = DIRECTION ( 'NONE',  ( 0.000000000000000000, 0.000000000000000000, 1.000000000000000000 ) ) ;
#4975 = VERTEX_POINT ( 'NONE', #8204 ) ;
#4976 = CARTESIAN_POINT ( 'NONE',  ( 1.243802165048773611, -3.900692638707475624, -3.223146290109810241 ) ) ;
#4977 = EDGE_LOOP ( 'NONE', ( #24117, #35600, #37362, #16666, #4390 ) ) ;
#4978 = ADVANCED_FACE ( 'NONE', ( #41333 ), #38295, .F. ) ;
#4979 = AXIS2_PLACEMENT_3D ( 'NONE', #19226, #29450, #19020 ) ;
#4980 = CARTESIAN_POINT ( 'NONE',  ( 0.000000000000000000, 0.000000000000000000, 0.000000000000000000 ) ) ;
#4981 = DIRECTION ( 'NONE',  ( 0.000000000000000000, 0.000000000000000000, 1.000000000000000000 ) ) ;
#4982 = EDGE_CURVE ( 'NONE', #8937, #13915, #11963, .T. ) ;
#4983 = CARTESIAN_POINT ( 'NONE',  ( -18.51709390187839688, 31.00000000000000355, -37.54239277154294996 ) ) ;
#4984 = VERTEX_POINT ( 'NONE', #1857 ) ;
#4985 = CARTESIAN_POINT ( 'NONE',  ( 0.2500000000000002220, 0.000000000000000000, 0.000000000000000000 ) ) ;
#4986 = CARTESIAN_POINT ( 'NONE',  ( 17.99999999999999645, 120.2856157092987957, -7.201503623195590009 ) ) ;
#4987 = AXIS2_PLACEMENT_3D ( 'NONE', #29919, #25991, #19250 ) ;
#4988 = CARTESIAN_POINT ( 'NONE',  ( 19.99305134020393382, 31.00000000000000355, 74.61661993947731730 ) ) ;
#4989 = EDGE_CURVE ( 'NONE', #41689, #18808, #4960, .T. ) ;
#4990 = ORIENTED_EDGE ( 'NONE', *, *, #26453, .T. ) ;
#4991 = CARTESIAN_POINT ( 'NONE',  ( 56.82522199878360425, 31.00000000000000355, 7.581518937762241173 ) ) ;
#4992 = CARTESIAN_POINT ( 'NONE',  ( -89.62817255407412631, 40.00000000000000711, -11.80141054548196422 ) ) ;
#4993 = ORIENTED_EDGE ( 'NONE', *, *, #7710, .T. ) ;
#4994 =( REPRESENTATION_RELATIONSHIP ('NONE','NONE', #330, #15194 ) REPRESENTATION_RELATIONSHIP_WITH_TRANSFORMATION ( #5878 )SHAPE_REPRESENTATION_RELATIONSHIP( ) );
#4995 = DIRECTION ( 'NONE',  ( 0.000000000000000000, 0.000000000000000000, 1.000000000000000000 ) ) ;
#4996 = ADVANCED_FACE ( 'NONE', ( #27637 ), #21337, .F. ) ;
#4997 = CARTESIAN_POINT ( 'NONE',  ( -12.69999999999999929, 0.000000000000000000, 0.000000000000000000 ) ) ;
#4998 = ADVANCED_FACE ( 'NONE', ( #17838 ), #30756, .T. ) ;
#4999 = EDGE_CURVE ( 'NONE', #3403, #37380, #41114, .T. ) ;
#5000 = EDGE_CURVE ( 'NONE', #41773, #9315, #20318, .T. ) ;
#5001 = CIRCLE ( 'NONE', #30089, 116.0000000000000000 ) ;
#5003 = ORIENTED_EDGE ( 'NONE', *, *, #39073, .T. ) ;
#5002 = LINE ( 'NONE', #28146, #3469 ) ;
#5004 = CARTESIAN_POINT ( 'NONE',  ( 0.000000000000000000, -18.53613841426756892, -48.58406706613922665 ) ) ;
#5005 = DIRECTION ( 'NONE',  ( -1.000000000000000000, 0.000000000000000000, 0.000000000000000000 ) ) ;
#5006 = VERTEX_POINT ( 'NONE', #41780 ) ;
#5007 = CARTESIAN_POINT ( 'NONE',  ( 57.13603463884887645, 40.00000000000000000, 32.98675068510902264 ) ) ;
#5008 = CARTESIAN_POINT ( 'NONE',  ( 18.00000000000000355, 0.000000000000000000, 0.000000000000000000 ) ) ;
#5009 = AXIS2_PLACEMENT_3D ( 'NONE', #7378, #20738, #34002 ) ;
#5010 = VERTEX_POINT ( 'NONE', #4255 ) ;
#5011 = LINE ( 'NONE', #14857, #41953 ) ;
#5012 = CARTESIAN_POINT ( 'NONE',  ( 3.983177536951266529, -13.66651769228263191, 0.000000000000000000 ) ) ;
#5013 = FACE_OUTER_BOUND ( 'NONE', #32700, .T. ) ;
#5014 = ORIENTED_EDGE ( 'NONE', *, *, #27318, .F. ) ;
#5015 = DIRECTION ( 'NONE',  ( -1.000000000000000000, 2.668805347656627603E-17, 0.000000000000000000 ) ) ;
#5016 = VERTEX_POINT ( 'NONE', #15220 ) ;
#5017 = DIRECTION ( 'NONE',  ( -1.000000000000000000, 0.000000000000000000, 0.000000000000000000 ) ) ;
#5018 = CARTESIAN_POINT ( 'NONE',  ( 17.99999999999999645, 0.000000000000000000, 0.000000000000000000 ) ) ;
#5019 = DIRECTION ( 'NONE',  ( 0.000000000000000000, 0.000000000000000000, 1.000000000000000000 ) ) ;
#5020 = DIRECTION ( 'NONE',  ( 1.000000000000000000, 0.000000000000000000, 0.000000000000000000 ) ) ;
#5021 = ORIENTED_EDGE ( 'NONE', *, *, #24000, .T. ) ;
#5022 = DIRECTION ( 'NONE',  ( -1.000000000000000000, 0.000000000000000000, 0.000000000000000000 ) ) ;
#5023 = VECTOR ( 'NONE', #21662, 1000.000000000000000 ) ;
#5024 = AXIS2_PLACEMENT_3D ( 'NONE', #1084, #17511, #38393 ) ;
#5025 = AXIS2_PLACEMENT_3D ( 'NONE', #21038, #34078, #17539 ) ;
#5026 = CYLINDRICAL_SURFACE ( 'NONE', #2899, 16.00000000000023448 ) ;
#5027 = ADVANCED_FACE ( 'NONE', ( #31545 ), #4706, .F. ) ;
#5028 = ORIENTED_EDGE ( 'NONE', *, *, #42625, .T. ) ;
#5029 = CARTESIAN_POINT ( 'NONE',  ( 18.00000000000000355, -44.47301969247456555, 16.68249143361894582 ) ) ;
#5030 = CIRCLE ( 'NONE', #34299, 58.99999999999999289 ) ;
#5031 = CARTESIAN_POINT ( 'NONE',  ( 18.00000000000000355, 0.000000000000000000, 0.000000000000000000 ) ) ;
#5032 = APPLICATION_PROTOCOL_DEFINITION ( 'draft international standard', 'automotive_design', 1998, #22886 ) ;
#5033 = CARTESIAN_POINT ( 'NONE',  ( 0.000000000000000000, 30.71634675606066267, -8.790889055186230649 ) ) ;
#5034 = CARTESIAN_POINT ( 'NONE',  ( 44.89583333484414140, 31.00000000000000355, -2.945243104263157274 ) ) ;
#5035 = CIRCLE ( 'NONE', #22487, 12.55910585664918422 ) ;
#5036 = ORIENTED_EDGE ( 'NONE', *, *, #1654, .F. ) ;
#5038 = DIRECTION ( 'NONE',  ( -3.996523416598930318E-16, 2.658563593772947863E-15, 1.000000000000000000 ) ) ;
#5037 = DIRECTION ( 'NONE',  ( -1.000000000000000000, 0.000000000000000000, 0.000000000000000000 ) ) ;
#5039 = ORIENTED_EDGE ( 'NONE', *, *, #35442, .T. ) ;
#5040 = CARTESIAN_POINT ( 'NONE',  ( 3.763366191185776088, 40.00000000000000000, 57.39583333449059666 ) ) ;
#5041 = CARTESIAN_POINT ( 'NONE',  ( 7.664524495375378166, 40.00000000000000000, 58.91906827748253050 ) ) ;
#5042 = FACE_OUTER_BOUND ( 'NONE', #20843, .T. ) ;
#5043 = DIRECTION ( 'NONE',  ( 1.000000000000000000, 1.836909530733573776E-16, 0.000000000000000000 ) ) ;
#5044 = EDGE_CURVE ( 'NONE', #28643, #12333, #31336, .T. ) ;
#5045 = EDGE_CURVE ( 'NONE', #28564, #14100, #12635, .T. ) ;
#5046 = DIRECTION ( 'NONE',  ( 0.000000000000000000, -0.7525707698561440173, 0.6585113790650322096 ) ) ;
#5047 = CARTESIAN_POINT ( 'NONE',  ( 23.22631124480444598, 31.00000000000000355, -7.893869537065737241 ) ) ;
#5048 = EDGE_CURVE ( 'NONE', #35040, #20538, #14769, .T. ) ;
#5049 = CIRCLE ( 'NONE', #158, 120.5010000000000190 ) ;
#5050 = ORIENTED_EDGE ( 'NONE', *, *, #16705, .F. ) ;
#5051 = CARTESIAN_POINT ( 'NONE',  ( -30.10416666442597844, 40.00000000000000000, -1.963495399902747574 ) ) ;
#5052 = ORIENTED_EDGE ( 'NONE', *, *, #25762, .F. ) ;
#5053 = CARTESIAN_POINT ( 'NONE',  ( 17.99999999999999645, 83.49789599728782719, 86.88263557826796557 ) ) ;
#5054 = CYLINDRICAL_SURFACE ( 'NONE', #32573, 20.00000000000000711 ) ;
#5055 = VERTEX_POINT ( 'NONE', #20907 ) ;
#5056 = DIRECTION ( 'NONE',  ( 0.000000000000000000, 0.000000000000000000, 1.000000000000000000 ) ) ;
#5057 = CARTESIAN_POINT ( 'NONE',  ( 0.000000000000000000, 0.000000000000000000, 0.000000000000000000 ) ) ;
#5058 = ORIENTED_EDGE ( 'NONE', *, *, #3376, .F. ) ;
#5059 = CARTESIAN_POINT ( 'NONE',  ( 1.393927851585479161, -4.043713361053543842, -3.526374918436840922 ) ) ;
#5060 = ORIENTED_EDGE ( 'NONE', *, *, #7410, .T. ) ;
#5061 = CIRCLE ( 'NONE', #36378, 52.00000000000000000 ) ;
#5062 = ORIENTED_EDGE ( 'NONE', *, *, #18769, .F. ) ;
#5063 = CARTESIAN_POINT ( 'NONE',  ( 5.639656061357294803, -10.48075544252183100, -1.199999999999999956 ) ) ;
#5064 = EDGE_CURVE ( 'NONE', #12884, #10324, #15433, .T. ) ;
#5065 = CARTESIAN_POINT ( 'NONE',  ( 83.84057477258951963, 31.00000000000000000, -22.33845567675551180 ) ) ;
#5066 = VERTEX_POINT ( 'NONE', #14988 ) ;
#5067 = DIRECTION ( 'NONE',  ( 0.000000000000000000, 0.000000000000000000, 1.000000000000000000 ) ) ;
#5068 = DIRECTION ( 'NONE',  ( 0.000000000000000000, -6.982962677686265922E-15, 1.000000000000000000 ) ) ;
#5069 = ORIENTED_EDGE ( 'NONE', *, *, #14033, .T. ) ;
#5070 = CARTESIAN_POINT ( 'NONE',  ( 4.197393957002303999, -0.4069871074557456780, -3.503767560748925813 ) ) ;
#5071 = ORIENTED_EDGE ( 'NONE', *, *, #35615, .F. ) ;
#5072 = CARTESIAN_POINT ( 'NONE',  ( 22.90854556226730310, -35.35525454449573601, -74.83297477053802993 ) ) ;
#5073 = CARTESIAN_POINT ( 'NONE',  ( -10.52919346384764054, 31.00000000000000355, -21.36894910329525032 ) ) ;
#5075 = CYLINDRICAL_SURFACE ( 'NONE', #32548, 116.0000000000000000 ) ;
#5074 = FACE_OUTER_BOUND ( 'NONE', #3855, .T. ) ;
#5076 = DIRECTION ( 'NONE',  ( -1.000000000000000000, 0.000000000000000000, 0.000000000000000000 ) ) ;
#5077 = CARTESIAN_POINT ( 'NONE',  ( 0.000000000000000000, 114.8812324315175033, 16.07179003769187986 ) ) ;
#5078 = VERTEX_POINT ( 'NONE', #28296 ) ;
#5079 = AXIS2_PLACEMENT_3D ( 'NONE', #12135, #2901, #2265 ) ;
#5080 = CARTESIAN_POINT ( 'NONE',  ( 17.99999999999999645, 0.000000000000000000, 0.000000000000000000 ) ) ;
#5081 = ORIENTED_EDGE ( 'NONE', *, *, #23327, .F. ) ;
#5082 = DIRECTION ( 'NONE',  ( -1.000000000000000000, 0.000000000000000000, 0.000000000000000000 ) ) ;
#5083 = CARTESIAN_POINT ( 'NONE',  ( 95.10416666600561086, 31.00000000000000000, 6.217735451873073416 ) ) ;
#5084 = CARTESIAN_POINT ( 'NONE',  ( 0.000000000000000000, -115.9387338813861987, 3.769613505535687636 ) ) ;
#5085 = ORIENTED_EDGE ( 'NONE', *, *, #10352, .F. ) ;
#5086 = AXIS2_PLACEMENT_3D ( 'NONE', #16088, #12391, #9083 ) ;
#5087 = COLOUR_RGB ( '', 0.72549020, 0.75294118, 0.79215686) ;
#5088 = CARTESIAN_POINT ( 'NONE',  ( 26.53203760875094019, 40.00000000000000000, 7.134992448515056651 ) ) ;
#5089 = VECTOR ( 'NONE', #19656, 1000.000000000000000 ) ;
#5090 = ORIENTED_EDGE ( 'NONE', *, *, #14851, .F. ) ;
#5091 = EDGE_LOOP ( 'NONE', ( #17118, #33569, #21105, #3596 ) ) ;
#5092 = CARTESIAN_POINT ( 'NONE',  ( -10.00000000000000000, 0.000000000000000000, 0.000000000000000000 ) ) ;
#5093 = CARTESIAN_POINT ( 'NONE',  ( 0.000000000000000000, 66.49630760163600485, 90.36876423296011751 ) ) ;
#5094 = DIRECTION ( 'NONE',  ( -1.000000000000000000, 0.000000000000000000, 0.000000000000000000 ) ) ;
#5095 = EDGE_CURVE ( 'NONE', #42446, #30653, #33512, .T. ) ;
#5096 = DIRECTION ( 'NONE',  ( -1.000000000000000000, 0.000000000000000000, 0.000000000000000000 ) ) ;
#5097 = ORIENTED_EDGE ( 'NONE', *, *, #38098, .T. ) ;
#5098 = CYLINDRICAL_SURFACE ( 'NONE', #13103, 130.0000000000000284 ) ;
#5099 = ORIENTED_EDGE ( 'NONE', *, *, #11532, .T. ) ;
#5100 = DIRECTION ( 'NONE',  ( -1.000000000000000000, -0.000000000000000000, 0.000000000000000000 ) ) ;
#5101 = FACE_BOUND ( 'NONE', #19325, .T. ) ;
#5102 = EDGE_CURVE ( 'NONE', #25078, #32554, #35585, .T. ) ;
#5103 = DIRECTION ( 'NONE',  ( 0.000000000000000000, 1.000000000000000000, -1.060184893785364939E-15 ) ) ;
#5104 = CIRCLE ( 'NONE', #39926, 13.59999999999999964 ) ;
#5105 = DIRECTION ( 'NONE',  ( 1.000000000000000000, 0.000000000000000000, 0.000000000000000000 ) ) ;
#5106 = EDGE_LOOP ( 'NONE', ( #3724, #38063, #24079, #42426 ) ) ;
#5107 = VERTEX_POINT ( 'NONE', #30893 ) ;
#5108 = CARTESIAN_POINT ( 'NONE',  ( 9.000000000000001776, -51.19683565102450018, 9.104066087303291255 ) ) ;
#5109 = DIRECTION ( 'NONE',  ( -1.000000000000000000, -0.000000000000000000, 0.000000000000000000 ) ) ;
#5110 = EDGE_CURVE ( 'NONE', #15819, #18858, #41155, .T. ) ;
#5111 = CIRCLE ( 'NONE', #16981, 120.5010000000000190 ) ;
#5112 = ORIENTED_EDGE ( 'NONE', *, *, #26850, .T. ) ;
#5114 = ORIENTED_EDGE ( 'NONE', *, *, #16195, .T. ) ;
#5113 = FACE_BOUND ( 'NONE', #4583, .T. ) ;
#5115 = ADVANCED_FACE ( 'NONE', ( #2261 ), #42190, .F. ) ;
#5116 = CARTESIAN_POINT ( 'NONE',  ( 12.49611804805956261, 31.00000000000000355, 37.00809541493615029 ) ) ;
#5117 = VERTEX_POINT ( 'NONE', #25453 ) ;
#5118 = DIRECTION ( 'NONE',  ( -1.000000000000000000, 0.000000000000000000, 0.000000000000000000 ) ) ;
#5120 = DIRECTION ( 'NONE',  ( 0.000000000000000000, 0.000000000000000000, 1.000000000000000000 ) ) ;
#5119 = LINE ( 'NONE', #18713, #39076 ) ;
#5121 = ORIENTED_EDGE ( 'NONE', *, *, #30559, .F. ) ;
#5122 = DIRECTION ( 'NONE',  ( -1.000000000000000000, 0.000000000000000000, 0.000000000000000000 ) ) ;
#5124 = CARTESIAN_POINT ( 'NONE',  ( -59.63693792272297856, 40.00000000000000711, 15.87187584492933823 ) ) ;
#5123 =( GEOMETRIC_REPRESENTATION_CONTEXT ( 3 ) GLOBAL_UNCERTAINTY_ASSIGNED_CONTEXT ( ( #26975 ) ) GLOBAL_UNIT_ASSIGNED_CONTEXT ( ( #12825, #2319, #25307 ) ) REPRESENTATION_CONTEXT ( 'NONE', 'WORKASPACE' ) );
#5125 = DIRECTION ( 'NONE',  ( 1.000000000000000000, 0.000000000000000000, -3.273063162220416457E-16 ) ) ;
#5126 = CARTESIAN_POINT ( 'NONE',  ( 18.00000000000001421, 9.184850993605147944E-16, -7.500000000000000000 ) ) ;
#5127 = VERTEX_POINT ( 'NONE', #21973 ) ;
#5128 = DIRECTION ( 'NONE',  ( 1.000000000000000000, -0.000000000000000000, 0.000000000000000000 ) ) ;
#5129 = CIRCLE ( 'NONE', #23286, 2.649999999999957723 ) ;
#5130 = ORIENTED_EDGE ( 'NONE', *, *, #16089, .T. ) ;
#5131 =( LENGTH_UNIT ( ) NAMED_UNIT ( * ) SI_UNIT ( .MILLI., .METRE. ) );
#5132 = EDGE_CURVE ( 'NONE', #5549, #14617, #32180, .T. ) ;
#5133 = DIRECTION ( 'NONE',  ( 0.000000000000000000, 0.000000000000000000, 1.000000000000000000 ) ) ;
#5134 = DIRECTION ( 'NONE',  ( 1.000000000000000000, 0.000000000000000000, 0.000000000000000000 ) ) ;
#5135 = VECTOR ( 'NONE', #2426, 1000.000000000000000 ) ;
#5136 = CARTESIAN_POINT ( 'NONE',  ( -23.19911330973958030, 31.00000000000000355, -68.30030121463531145 ) ) ;
#5137 = DIRECTION ( 'NONE',  ( -1.000000000000000000, -0.000000000000000000, -0.000000000000000000 ) ) ;
#5138 = ORIENTED_EDGE ( 'NONE', *, *, #2767, .T. ) ;
#5139 = CIRCLE ( 'NONE', #18457, 52.00000000000000000 ) ;
#5140 = DIRECTION ( 'NONE',  ( 0.000000000000000000, 0.000000000000000000, 1.000000000000000000 ) ) ;
#5141 = VERTEX_POINT ( 'NONE', #38712 ) ;
#5142 = LINE ( 'NONE', #41793, #4018 ) ;
#5143 = DIRECTION ( 'NONE',  ( -3.009274222672345096E-17, -1.000000000000000000, 2.455023325076455345E-18 ) ) ;
#5144 = CARTESIAN_POINT ( 'NONE',  ( -10.92011822083620309, 31.00000000000000355, -83.75917815547792600 ) ) ;
#5145 = CARTESIAN_POINT ( 'NONE',  ( 5.735608225908777946, 40.00000000000000000, 89.40012361736363289 ) ) ;
#5146 = DIRECTION ( 'NONE',  ( -1.000000000000000000, -0.000000000000000000, -0.000000000000000000 ) ) ;
#5147 = EDGE_CURVE ( 'NONE', #34755, #34370, #1454, .T. ) ;
#5148 = EDGE_LOOP ( 'NONE', ( #31660, #30323, #41809, #40796 ) ) ;
#5149 = DIRECTION ( 'NONE',  ( 0.000000000000000000, 0.000000000000000000, 1.000000000000000000 ) ) ;
#5150 = VERTEX_POINT ( 'NONE', #12349 ) ;
#5151 = AXIS2_PLACEMENT_3D ( 'NONE', #34819, #7555, #31552 ) ;
#5152 = DIRECTION ( 'NONE',  ( 1.000000000000000000, 0.000000000000000000, 0.000000000000000000 ) ) ;
#5153 = CYLINDRICAL_SURFACE ( 'NONE', #4560, 36.00000000000000000 ) ;
#5155 = ORIENTED_EDGE ( 'NONE', *, *, #8850, .F. ) ;
#5154 = DIRECTION ( 'NONE',  ( -1.000000000000000000, 1.577021341797098793E-16, 0.000000000000000000 ) ) ;
#5156 = CLOSED_SHELL ( 'NONE', ( #11390, #17769, #21411, #31700, #36108, #22905, #2007, #37370, #40041, #30386, #39837, #29411, #12008, #42611, #38116, #7814, #20253, #29250, #5489, #19636, #41260, #15535, #23935, #41545, #22012, #37144, #13377, #20211, #22616, #31401, #29732, #21008, #21220, #4191, #2051, #6737, #42483, #13350, #33730, #36344, #11227, #42732, #32296, #41762, #14615, #14448, #38735, #17674, #8738, #19714, #28870, #19536, #3679, #31342, #21773, #31146, #5969, #24793, #13025, #8925, #43066, #19175, #33510, #7074, #126, #12207, #8002, #30302, #22157, #21191, #13109, #3784, #34152, #32513, #2176, #37703, #6145, #24192, #35136, #28420, #20462, #13511, #31773, #9200, #9381, #41475, #10259, #19463, #42244, #40388, #34545, #17373, #28529, #16196, #32885, #22733, #38217, #32371, #20389, #29793, #15482, #1311, #1902, #43133, #23457, #27821, #13000, #13216, #30911, #39086, #1911, #24553, #15555, #24320, #131, #10903, #18397, #15608, #19480, #16225, #1429, #24976, #11923, #11975, #36442, #12709, #10713, #34595, #38250, #22215, #36527, #37608, #36612, #29899, #15656, #20085, #35002, #6419, #25106, #22282, #10729, #37500, #41173, #32010, #41330 ) ) ;
#5157 = CARTESIAN_POINT ( 'NONE',  ( 9.999999999999998224, 0.000000000000000000, 0.000000000000000000 ) ) ;
#5158 = VERTEX_POINT ( 'NONE', #15421 ) ;
#5159 = DIRECTION ( 'NONE',  ( -1.000000000000000000, 0.000000000000000000, -0.000000000000000000 ) ) ;
#5160 = VECTOR ( 'NONE', #32489, 1000.000000000000000 ) ;
#5161 = EDGE_CURVE ( 'NONE', #13064, #38711, #19626, .T. ) ;
#5162 = CARTESIAN_POINT ( 'NONE',  ( 18.00000000000000355, -42.60732521687558005, -19.80331771201703006 ) ) ;
#5163 = CIRCLE ( 'NONE', #37202, 20.00000000000000711 ) ;
#5164 = ORIENTED_EDGE ( 'NONE', *, *, #31561, .F. ) ;
#5165 = LINE ( 'NONE', #38531, #21399 ) ;
#5166 = DIRECTION ( 'NONE',  ( -1.000000000000000000, 0.000000000000000000, 0.000000000000000000 ) ) ;
#5167 = AXIS2_PLACEMENT_3D ( 'NONE', #12668, #42725, #6310 ) ;
#5169 = FACE_OUTER_BOUND ( 'NONE', #41361, .T. ) ;
#5168 = DIRECTION ( 'NONE',  ( 0.000000000000000000, 0.9407002666710319039, 0.3392388661180338882 ) ) ;
#5170 = AXIS2_PLACEMENT_3D ( 'NONE', #23123, #33978, #17222 ) ;
#5171 = VERTEX_POINT ( 'NONE', #42618 ) ;
#5172 = DIRECTION ( 'NONE',  ( 0.000000000000000000, 0.000000000000000000, 1.000000000000000000 ) ) ;
#5173 = ORIENTED_EDGE ( 'NONE', *, *, #7615, .T. ) ;
#5174 = CARTESIAN_POINT ( 'NONE',  ( 17.99999999999999645, 19.12429268481714928, 114.4126803693779948 ) ) ;
#5175 = CARTESIAN_POINT ( 'NONE',  ( 35.58384423644164229, 40.00000000000000000, 12.14845634898874494 ) ) ;
#5176 = DIRECTION ( 'NONE',  ( 0.000000000000000000, 0.2113826236296247330, -0.9774033898178666746 ) ) ;
#5177 = CYLINDRICAL_SURFACE ( 'NONE', #15225, 2.500000000000000444 ) ;
#5178 = CARTESIAN_POINT ( 'NONE',  ( 9.000000000000001776, -101.8011932243944386, -55.61040422519432980 ) ) ;
#5179 = ORIENTED_EDGE ( 'NONE', *, *, #33784, .F. ) ;
#5180 = DIRECTION ( 'NONE',  ( -3.009274222672345096E-17, -1.000000000000000000, 2.455023325076454960E-18 ) ) ;
#5181 = DIRECTION ( 'NONE',  ( -1.000000000000000000, -0.000000000000000000, -0.000000000000000000 ) ) ;
#5182 = AXIS2_PLACEMENT_3D ( 'NONE', #20362, #33623, #40156 ) ;
#5183 = ORIENTED_EDGE ( 'NONE', *, *, #34113, .T. ) ;
#5184 = AXIS2_PLACEMENT_3D ( 'NONE', #38405, #1970, #24946 ) ;
#5185 = ADVANCED_FACE ( 'NONE', ( #19547 ), #39339, .F. ) ;
#5186 = DIRECTION ( 'NONE',  ( -1.000000000000000000, -0.000000000000000000, 0.000000000000000000 ) ) ;
#5187 = DIRECTION ( 'NONE',  ( 0.000000000000000000, 0.8747630845319623871, -0.4845508703326482647 ) ) ;
#5189 = ADVANCED_FACE ( 'NONE', ( #2060 ), #29352, .T. ) ;
#5188 = CARTESIAN_POINT ( 'NONE',  ( 30.80114556864472775, 31.00000000000000355, -15.19345985420777190 ) ) ;
#5190 = ORIENTED_EDGE ( 'NONE', *, *, #29366, .F. ) ;
#5191 = CARTESIAN_POINT ( 'NONE',  ( 17.99999999999999645, 111.7974656912331426, -9.465682155094398809 ) ) ;
#5192 = AXIS2_PLACEMENT_3D ( 'NONE', #38593, #25344, #32074 ) ;
#5193 = DIRECTION ( 'NONE',  ( 1.000000000000000000, -3.469446951953614189E-17, 0.000000000000000000 ) ) ;
#5194 = CARTESIAN_POINT ( 'NONE',  ( -70.15350862410126354, 31.00000000000000711, -40.50401079722123399 ) ) ;
#5195 = AXIS2_PLACEMENT_3D ( 'NONE', #34023, #16675, #19945 ) ;
#5196 = CIRCLE ( 'NONE', #38634, 52.00000000000000000 ) ;
#5197 = ORIENTED_EDGE ( 'NONE', *, *, #26203, .F. ) ;
#5198 = CARTESIAN_POINT ( 'NONE',  ( -23.74678488967455436, 31.00000000000000355, -48.36925102894097961 ) ) ;
#5199 = CIRCLE ( 'NONE', #28889, 13.59999999999999964 ) ;
#5200 = CARTESIAN_POINT ( 'NONE',  ( -70.72766149062127283, 40.00000000000000711, 54.26934393422349956 ) ) ;
#5201 = EDGE_CURVE ( 'NONE', #2622, #21205, #42556, .T. ) ;
#5202 = VECTOR ( 'NONE', #11513, 1000.000000000000000 ) ;
#5203 = ORIENTED_EDGE ( 'NONE', *, *, #1131, .T. ) ;
#5204 = CARTESIAN_POINT ( 'NONE',  ( -4.140404888673278272, -2.228338276487456415, -3.686887068327035166 ) ) ;
#5205 = CARTESIAN_POINT ( 'NONE',  ( -6.004904395537136175, 0.000000000000000000, 0.000000000000000000 ) ) ;
#5206 = FACE_OUTER_BOUND ( 'NONE', #26391, .T. ) ;
#5208 = ORIENTED_EDGE ( 'NONE', *, *, #35205, .F. ) ;
#5207 = CYLINDRICAL_SURFACE ( 'NONE', #23740, 59.00000000000000000 ) ;
#5209 = DIRECTION ( 'NONE',  ( -1.000000000000000000, 0.000000000000000000, -0.000000000000000000 ) ) ;
#5210 = CARTESIAN_POINT ( 'NONE',  ( 17.99999999999999645, -14.84191762912334767, 27.78316904333121684 ) ) ;
#5211 = CIRCLE ( 'NONE', #8699, 20.00000000000000355 ) ;
#5212 = EDGE_CURVE ( 'NONE', #33622, #16464, #8837, .T. ) ;
#5213 = VERTEX_POINT ( 'NONE', #39137 ) ;
#5214 = CARTESIAN_POINT ( 'NONE',  ( -19.97695672607123640, 40.00000000000000000, -58.81104016858105155 ) ) ;
#5215 = DIRECTION ( 'NONE',  ( 0.000000000000000000, 0.000000000000000000, 1.000000000000000000 ) ) ;
#5216 = VERTEX_POINT ( 'NONE', #26293 ) ;
#5217 = EDGE_CURVE ( 'NONE', #43150, #23930, #9050, .T. ) ;
#5218 = CARTESIAN_POINT ( 'NONE',  ( 0.000000000000000000, 66.49630760163724119, -90.36876423295917959 ) ) ;
#5219 = CARTESIAN_POINT ( 'NONE',  ( -3.239593890920906993, -13.56862304811759223, 0.000000000000000000 ) ) ;
#5220 = VECTOR ( 'NONE', #9196, 1000.000000000000000 ) ;
#5221 = CYLINDRICAL_SURFACE ( 'NONE', #29135, 120.5010000000000190 ) ;
#5222 = ORIENTED_EDGE ( 'NONE', *, *, #28811, .T. ) ;
#5223 = CIRCLE ( 'NONE', #13625, 120.5010000000000190 ) ;
#5224 = CIRCLE ( 'NONE', #8679, 2.649999999999985700 ) ;
#5225 = EDGE_LOOP ( 'NONE', ( #14781, #27174, #36143, #24895 ) ) ;
#5226 = LINE ( 'NONE', #11581, #17060 ) ;
#5227 = VERTEX_POINT ( 'NONE', #22403 ) ;
#5228 = AXIS2_PLACEMENT_3D ( 'NONE', #11343, #14846, #18146 ) ;
#5229 = DIRECTION ( 'NONE',  ( 1.000000000000000000, 0.000000000000000000, 0.000000000000000000 ) ) ;
#5230 = FACE_OUTER_BOUND ( 'NONE', #2906, .T. ) ;
#5231 = AXIS2_PLACEMENT_3D ( 'NONE', #34425, #4530, #26444 ) ;
#5232 = VECTOR ( 'NONE', #17854, 1000.000000000000000 ) ;
#5233 = DIRECTION ( 'NONE',  ( -1.000000000000000000, 0.000000000000000000, -0.000000000000000000 ) ) ;
#5234 = CARTESIAN_POINT ( 'NONE',  ( 18.00000000000000355, 0.000000000000000000, 0.000000000000000000 ) ) ;
#5235 = ORIENTED_EDGE ( 'NONE', *, *, #35877, .F. ) ;
#5236 = DIRECTION ( 'NONE',  ( 0.000000000000000000, 0.000000000000000000, 1.000000000000000000 ) ) ;
#5237 = CARTESIAN_POINT ( 'NONE',  ( 0.000000000000000000, -98.69720329640996681, 60.94966826379877745 ) ) ;
#5238 = EDGE_CURVE ( 'NONE', #39353, #20934, #11935, .T. ) ;
#5239 = ADVANCED_FACE ( 'NONE', ( #35449 ), #9259, .F. ) ;
#5240 = ORIENTED_EDGE ( 'NONE', *, *, #22433, .T. ) ;
#5241 = DIRECTION ( 'NONE',  ( -1.000000000000000000, -0.000000000000000000, -0.000000000000000000 ) ) ;
#5242 = ADVANCED_FACE ( 'NONE', ( #42413 ), #2895, .F. ) ;
#5243 = EDGE_CURVE ( 'NONE', #1492, #12095, #32610, .T. ) ;
#5244 = DIRECTION ( 'NONE',  ( 0.000000000000000000, -1.332282330596594362E-14, -1.000000000000000000 ) ) ;
#5245 = DIRECTION ( 'NONE',  ( 6.413747168845437910E-31, 1.000000000000000000, 6.123233995736766036E-17 ) ) ;
#5246 = DIRECTION ( 'NONE',  ( 0.000000000000000000, 0.000000000000000000, 1.000000000000000000 ) ) ;
#5247 = CARTESIAN_POINT ( 'NONE',  ( 13.71368254939966036, 31.00000000000000355, -51.22554439249349656 ) ) ;
#5248 = ORIENTED_EDGE ( 'NONE', *, *, #12173, .F. ) ;
#5250 = DIRECTION ( 'NONE',  ( -1.000000000000000000, 0.000000000000000000, 0.000000000000000000 ) ) ;
#5249 = DIRECTION ( 'NONE',  ( -1.000000000000000000, -0.000000000000000000, -0.000000000000000000 ) ) ;
#5251 = APPLICATION_CONTEXT ( 'automotive_design' ) ;
#5253 = EDGE_LOOP ( 'NONE', ( #7674, #38000, #38428, #36957 ) ) ;
#5252 = CIRCLE ( 'NONE', #28972, 10.50000000000000178 ) ;
#5254 = AXIS2_PLACEMENT_3D ( 'NONE', #21445, #37534, #4141 ) ;
#5255 = VECTOR ( 'NONE', #29258, 1000.000000000000000 ) ;
#5256 = CARTESIAN_POINT ( 'NONE',  ( -4.090615425948576522, 40.00000000000000000, -62.39583333438447710 ) ) ;
#5257 = AXIS2_PLACEMENT_3D ( 'NONE', #37535, #34258, #17725 ) ;
#5258 = CIRCLE ( 'NONE', #29657, 13.60000000000000142 ) ;
#5259 = AXIS2_PLACEMENT_3D ( 'NONE', #8434, #21998, #4732 ) ;
#5260 = CARTESIAN_POINT ( 'NONE',  ( 18.00000000000000355, -39.55064067543082018, 25.36340625197346199 ) ) ;
#5261 = DIRECTION ( 'NONE',  ( -1.000000000000000000, -0.000000000000000000, -0.000000000000000000 ) ) ;
#5262 = CIRCLE ( 'NONE', #23381, 13.40000000000000036 ) ;
#5263 = CARTESIAN_POINT ( 'NONE',  ( 18.00000000000000355, 51.85248208264516734, 3.914090171286377817 ) ) ;
#5264 = CARTESIAN_POINT ( 'NONE',  ( -20.10416666680962550, 31.00000000000000355, -1.308996940106889273 ) ) ;
#5265 = EDGE_CURVE ( 'NONE', #7867, #37436, #23095, .T. ) ;
#5266 = ORIENTED_EDGE ( 'NONE', *, *, #2308, .T. ) ;
#5267 = CARTESIAN_POINT ( 'NONE',  ( 31.10108666877329853, 40.00000000000000000, 17.95223046116557697 ) ) ;
#5268 = VERTEX_POINT ( 'NONE', #31980 ) ;
#5269 = CARTESIAN_POINT ( 'NONE',  ( 17.99999999999999645, 14.84191762912315049, 27.78316904333131276 ) ) ;
#5270 = CARTESIAN_POINT ( 'NONE',  ( 9.000000000000001776, 46.77034588191335018, -22.72740077717179830 ) ) ;
#5271 = ORIENTED_EDGE ( 'NONE', *, *, #4009, .T. ) ;
#5272 = EDGE_CURVE ( 'NONE', #29573, #9315, #9128, .T. ) ;
#5273 = DIRECTION ( 'NONE',  ( -3.996523416598930318E-16, 2.658563593772947863E-15, 1.000000000000000000 ) ) ;
#5274 = DIRECTION ( 'NONE',  ( -1.000000000000000000, -0.000000000000000000, -0.000000000000000000 ) ) ;
#5275 = VERTEX_POINT ( 'NONE', #20627 ) ;
#5276 = CARTESIAN_POINT ( 'NONE',  ( 0.6937372685066666156, -4.453844082567737672, -3.610536846335894445 ) ) ;
#5277 = ORIENTED_EDGE ( 'NONE', *, *, #27912, .T. ) ;
#5278 = VERTEX_POINT ( 'NONE', #19984 ) ;
#5279 = FACE_OUTER_BOUND ( 'NONE', #34037, .T. ) ;
#5280 = CARTESIAN_POINT ( 'NONE',  ( -54.99468034530342919, 31.00000000000000355, -62.86974495748531666 ) ) ;
#5281 = ORIENTED_EDGE ( 'NONE', *, *, #31581, .T. ) ;
#5282 = CARTESIAN_POINT ( 'NONE',  ( 17.99999999999999645, 112.5120133921113563, -43.14554256760899875 ) ) ;
#5283 = CIRCLE ( 'NONE', #9447, 36.00000000000000000 ) ;
#5285 = DIRECTION ( 'NONE',  ( 1.000000000000000000, 0.000000000000000000, 0.000000000000000000 ) ) ;
#5284 = CIRCLE ( 'NONE', #41525, 58.99999999999998579 ) ;
#5286 = ORIENTED_EDGE ( 'NONE', *, *, #6083, .F. ) ;
#5287 = AXIS2_PLACEMENT_3D ( 'NONE', #21788, #27657, #41794 ) ;
#5288 = CARTESIAN_POINT ( 'NONE',  ( -4.207491450040567571, 2.029819825146470524, -3.671670828759566074 ) ) ;
#5289 = LINE ( 'NONE', #31921, #29712 ) ;
#5290 =( GEOMETRIC_REPRESENTATION_CONTEXT ( 3 ) GLOBAL_UNCERTAINTY_ASSIGNED_CONTEXT ( ( #2937 ) ) GLOBAL_UNIT_ASSIGNED_CONTEXT ( ( #7508, #4218, #37169 ) ) REPRESENTATION_CONTEXT ( 'NONE', 'WORKASPACE' ) );
#5291 = CARTESIAN_POINT ( 'NONE',  ( 19.49047152472852673, 31.00000000000000355, -17.07028940128360261 ) ) ;
#5292 = AXIS2_PLACEMENT_3D ( 'NONE', #7112, #13690, #3811 ) ;
#5293 = EDGE_CURVE ( 'NONE', #192, #24364, #26931, .T. ) ;
#5295 = DIRECTION ( 'NONE',  ( 0.000000000000000000, 0.000000000000000000, 1.000000000000000000 ) ) ;
#5294 = CARTESIAN_POINT ( 'NONE',  ( -10.00000000000000000, 0.000000000000000000, 0.000000000000000000 ) ) ;
#5296 = EDGE_CURVE ( 'NONE', #24285, #16293, #39750, .T. ) ;
#5297 = EDGE_CURVE ( 'NONE', #3781, #10000, #2137, .T. ) ;
#5298 = CIRCLE ( 'NONE', #10888, 47.49900000000000233 ) ;
#5299 = DIRECTION ( 'NONE',  ( -1.000000000000000000, 0.000000000000000000, 0.000000000000000000 ) ) ;
#5300 = DIRECTION ( 'NONE',  ( 0.000000000000000000, -0.7525707698561440173, 0.6585113790650324317 ) ) ;
#5301 = VERTEX_POINT ( 'NONE', #20408 ) ;
#5302 = SURFACE_SIDE_STYLE ('',( #28464 ) ) ;
#5303 = EDGE_CURVE ( 'NONE', #41672, #25049, #9696, .T. ) ;
#5304 = CIRCLE ( 'NONE', #6656, 125.9999999999993605 ) ;
#5305 = FACE_OUTER_BOUND ( 'NONE', #37404, .T. ) ;
#5306 = ORIENTED_EDGE ( 'NONE', *, *, #35678, .T. ) ;
#5307 = DIRECTION ( 'NONE',  ( -1.000000000000000000, 0.000000000000000000, -0.000000000000000000 ) ) ;
#5308 = CARTESIAN_POINT ( 'NONE',  ( 17.99999999999999645, -98.39501399267926729, -53.91376164787777014 ) ) ;
#5309 = CARTESIAN_POINT ( 'NONE',  ( 8.999999999999998224, 110.8621702203448649, 34.14058016547577523 ) ) ;
#5310 = ORIENTED_EDGE ( 'NONE', *, *, #24792, .F. ) ;
#5311 = CARTESIAN_POINT ( 'NONE',  ( 33.88265278290065652, 40.00000000000000000, 16.77599488388066007 ) ) ;
#5312 = ORIENTED_EDGE ( 'NONE', *, *, #1747, .T. ) ;
#5313 = EDGE_CURVE ( 'NONE', #31622, #37525, #32120, .T. ) ;
#5314 = ORIENTED_EDGE ( 'NONE', *, *, #25942, .F. ) ;
#5315 = DIRECTION ( 'NONE',  ( 0.000000000000000000, 0.000000000000000000, 1.000000000000000000 ) ) ;
#5316 = LINE ( 'NONE', #5530, #22121 ) ;
#5317 = LINE ( 'NONE', #21528, #42896 ) ;
#5318 = DIRECTION ( 'NONE',  ( -1.000000000000000000, -0.000000000000000000, 0.000000000000000000 ) ) ;
#5319 = CIRCLE ( 'NONE', #21412, 58.99999999999999289 ) ;
#5320 = AXIS2_PLACEMENT_3D ( 'NONE', #12604, #36781, #6673 ) ;
#5321 = CIRCLE ( 'NONE', #36660, 120.5010000000000332 ) ;
#5322 = DIRECTION ( 'NONE',  ( 1.000000000000000000, 0.000000000000000000, 0.000000000000000000 ) ) ;
#5323 = VERTEX_POINT ( 'NONE', #13863 ) ;
#5324 = DIRECTION ( 'NONE',  ( 0.000000000000000000, 0.000000000000000000, -1.000000000000000000 ) ) ;
#5325 = ORIENTED_EDGE ( 'NONE', *, *, #21329, .F. ) ;
#5326 = CARTESIAN_POINT ( 'NONE',  ( 9.999999999999998224, 0.000000000000000000, 0.000000000000000000 ) ) ;
#5327 = DIRECTION ( 'NONE',  ( 1.000000000000000000, 0.000000000000000000, 0.000000000000000000 ) ) ;
#5328 = AXIS2_PLACEMENT_3D ( 'NONE', #6164, #25837, #29741 ) ;
#5329 = AXIS2_PLACEMENT_3D ( 'NONE', #8779, #6355, #22138 ) ;
#5330 = EDGE_CURVE ( 'NONE', #32585, #37461, #29999, .T. ) ;
#5331 = CIRCLE ( 'NONE', #17200, 52.00000000000000000 ) ;
#5332 = DIRECTION ( 'NONE',  ( 0.000000000000000000, 0.3140767120219495334, -0.9493976084683810601 ) ) ;
#5333 = CARTESIAN_POINT ( 'NONE',  ( 18.00000000000000355, -46.90537658765333617, 2.727856614654147638 ) ) ;
#5334 = EDGE_LOOP ( 'NONE', ( #7355, #22700 ) ) ;
#5335 = VERTEX_POINT ( 'NONE', #3340 ) ;
#5336 = CARTESIAN_POINT ( 'NONE',  ( 17.99999999999999645, -17.33727698085246871, 110.8498592715972961 ) ) ;
#5337 = CIRCLE ( 'NONE', #8820, 120.5010000000000332 ) ;
#5338 = ORIENTED_EDGE ( 'NONE', *, *, #10542, .T. ) ;
#5340 = ORIENTED_EDGE ( 'NONE', *, *, #13057, .F. ) ;
#5339 = CARTESIAN_POINT ( 'NONE',  ( 0.000000000000000000, -110.8621702203446659, -34.14058016547651420 ) ) ;
#5341 = CARTESIAN_POINT ( 'NONE',  ( 50.61746024623598572, 31.00000000000000355, -24.85206051842254737 ) ) ;
#5342 = VERTEX_POINT ( 'NONE', #19758 ) ;
#5343 = CYLINDRICAL_SURFACE ( 'NONE', #5646, 10.99999999999999645 ) ;
#5344 = AXIS2_PLACEMENT_3D ( 'NONE', #16927, #30210, #23689 ) ;
#5345 = DIRECTION ( 'NONE',  ( -0.000000000000000000, -0.000000000000000000, 1.000000000000000000 ) ) ;
#5346 = ORIENTED_EDGE ( 'NONE', *, *, #25625, .T. ) ;
#5347 = CARTESIAN_POINT ( 'NONE',  ( -44.72205690102931896, 40.00000000000000000, -58.47036224960022111 ) ) ;
#5348 = EDGE_CURVE ( 'NONE', #28845, #12939, #15459, .T. ) ;
#5349 = AXIS2_PLACEMENT_3D ( 'NONE', #28953, #2085, #2504 ) ;
#5350 = DIRECTION ( 'NONE',  ( -1.000000000000000000, 0.000000000000000000, 0.000000000000000000 ) ) ;
#5351 = EDGE_CURVE ( 'NONE', #22453, #36212, #26584, .T. ) ;
#5352 = DIRECTION ( 'NONE',  ( 0.000000000000000000, 0.000000000000000000, 1.000000000000000000 ) ) ;
#5354 = ORIENTED_EDGE ( 'NONE', *, *, #36093, .T. ) ;
#5353 = CIRCLE ( 'NONE', #16417, 59.00000000000000000 ) ;
#5355 = DIRECTION ( 'NONE',  ( 0.000000000000000000, 1.000000000000000000, -1.060184893785364939E-15 ) ) ;
#5356 = AXIS2_PLACEMENT_3D ( 'NONE', #32571, #22160, #9435 ) ;
#5357 = ORIENTED_EDGE ( 'NONE', *, *, #37444, .T. ) ;
#5358 = DIRECTION ( 'NONE',  ( -1.000000000000000000, -0.000000000000000000, -0.000000000000000000 ) ) ;
#5359 = DIRECTION ( 'NONE',  ( 0.000000000000000000, 0.000000000000000000, 1.000000000000000000 ) ) ;
#5360 = CARTESIAN_POINT ( 'NONE',  ( 29.59587406094124873, 31.00000000000000355, 60.01321678176139329 ) ) ;
#5361 = DIRECTION ( 'NONE',  ( -1.000000000000000000, -0.000000000000000000, 0.000000000000000000 ) ) ;
#5363 = VERTEX_POINT ( 'NONE', #3547 ) ;
#5362 = CIRCLE ( 'NONE', #31127, 59.00000000000000000 ) ;
#5364 = EDGE_CURVE ( 'NONE', #14556, #31789, #13822, .T. ) ;
#5366 = CIRCLE ( 'NONE', #6751, 59.00000000000000711 ) ;
#5365 = LINE ( 'NONE', #37861, #5232 ) ;
#5367 = AXIS2_PLACEMENT_3D ( 'NONE', #3106, #2256, #35851 ) ;
#5368 = EDGE_CURVE ( 'NONE', #10216, #28707, #33897, .T. ) ;
#5369 = ORIENTED_EDGE ( 'NONE', *, *, #19092, .F. ) ;
#5370 = DIRECTION ( 'NONE',  ( 0.000000000000000000, 0.000000000000000000, 1.000000000000000000 ) ) ;
#5371 = DIRECTION ( 'NONE',  ( -1.058513553088275437E-16, -1.000000000000000000, 8.813324511995299047E-17 ) ) ;
#5372 = CARTESIAN_POINT ( 'NONE',  ( 37.87019299815447937, 31.00000000000000355, -76.55254356380190472 ) ) ;
#5373 = CARTESIAN_POINT ( 'NONE',  ( 11.20008397363331198, 40.00000000000000000, -84.14439686172906363 ) ) ;
#5374 = EDGE_CURVE ( 'NONE', #39340, #37783, #537, .T. ) ;
#5375 = CARTESIAN_POINT ( 'NONE',  ( 17.99999999999999645, 0.000000000000000000, 0.000000000000000000 ) ) ;
#5376 = EDGE_LOOP ( 'NONE', ( #10798, #40178, #5130, #15126, #16261 ) ) ;
#5377 = DIRECTION ( 'NONE',  ( -1.000000000000000000, 0.000000000000000000, -0.000000000000000000 ) ) ;
#5378 = ORIENTED_EDGE ( 'NONE', *, *, #38040, .F. ) ;
#5379 =( LENGTH_UNIT ( ) NAMED_UNIT ( * ) SI_UNIT ( .MILLI., .METRE. ) );
#5380 = DIRECTION ( 'NONE',  ( 0.000000000000000000, -0.3641605752528294104, 0.9313361774523356562 ) ) ;
#5381 = AXIS2_PLACEMENT_3D ( 'NONE', #27387, #26527, #36750 ) ;
#5383 = VERTEX_POINT ( 'NONE', #10346 ) ;
#5382 = FACE_OUTER_BOUND ( 'NONE', #4494, .T. ) ;
#5384 = LINE ( 'NONE', #2088, #40751 ) ;
#5385 = ORIENTED_EDGE ( 'NONE', *, *, #20734, .F. ) ;
#5386 = CARTESIAN_POINT ( 'NONE',  ( 9.000000000000001776, -109.3506818544112917, 38.70953859160975696 ) ) ;
#5387 = VECTOR ( 'NONE', #7452, 1000.000000000000000 ) ;
#5388 = DIRECTION ( 'NONE',  ( -1.058513553088275437E-16, -1.000000000000000000, 8.813324511995299047E-17 ) ) ;
#5389 = AXIS2_PLACEMENT_3D ( 'NONE', #37134, #41265, #27557 ) ;
#5390 = DIRECTION ( 'NONE',  ( -1.000000000000000000, 0.000000000000000000, -0.000000000000000000 ) ) ;
#5391 = ORIENTED_EDGE ( 'NONE', *, *, #27933, .F. ) ;
#5392 = CARTESIAN_POINT ( 'NONE',  ( 25.73918080462996372, 31.00000000000000355, -6.871072672212910959 ) ) ;
#5393 = CARTESIAN_POINT ( 'NONE',  ( 0.000000000000000000, -43.55304910509386218, -28.41006711800032392 ) ) ;
#5394 = AXIS2_PLACEMENT_3D ( 'NONE', #15186, #24574, #5327 ) ;
#5395 = AXIS2_PLACEMENT_3D ( 'NONE', #10962, #21235, #21464 ) ;
#5397 = DIRECTION ( 'NONE',  ( 3.009274222672345096E-17, 1.000000000000000000, -2.455023325076454960E-18 ) ) ;
#5396 = LINE ( 'NONE', #35484, #24470 ) ;
#5398 = ORIENTED_EDGE ( 'NONE', *, *, #1304, .F. ) ;
#5399 = DIRECTION ( 'NONE',  ( -1.000000000000000000, 0.000000000000000000, -0.000000000000000000 ) ) ;
#5400 = CARTESIAN_POINT ( 'NONE',  ( 0.000000000000000000, -115.5737863835462917, 9.934782381633276316 ) ) ;
#5401 = CARTESIAN_POINT ( 'NONE',  ( 40.10317558969867946, 40.00000000000000000, -23.06553963618951286 ) ) ;
#5402 = CARTESIAN_POINT ( 'NONE',  ( -10.00000000000000000, 0.000000000000000000, 0.000000000000000000 ) ) ;
#5403 = CIRCLE ( 'NONE', #6754, 13.60000000000000142 ) ;
#5404 = CARTESIAN_POINT ( 'NONE',  ( 20.55500000000001748, 0.000000000000000000, 2.500000000000000888 ) ) ;
#5405 = CARTESIAN_POINT ( 'NONE',  ( 9.000000000000000000, -29.09613215194497826, 21.19941258140312002 ) ) ;
#5406 = ORIENTED_EDGE ( 'NONE', *, *, #15582, .T. ) ;
#5407 = CARTESIAN_POINT ( 'NONE',  ( 2.725741868436127202, -3.045094352033990148, -3.220599429844051453 ) ) ;
#5408 = EDGE_CURVE ( 'NONE', #5107, #19359, #27774, .T. ) ;
#5409 = EDGE_LOOP ( 'NONE', ( #26215, #4736, #32992, #16953 ) ) ;
#5410 = CYLINDRICAL_SURFACE ( 'NONE', #22528, 59.00000000000000000 ) ;
#5411 = CARTESIAN_POINT ( 'NONE',  ( 0.000000000000000000, -79.18387647320821543, 84.76976882518735579 ) ) ;
#5412 = CARTESIAN_POINT ( 'NONE',  ( 33.70925502316616473, 31.00000000000000355, 11.43906998022225707 ) ) ;
#5413 = ORIENTED_EDGE ( 'NONE', *, *, #38339, .F. ) ;
#5414 = DIRECTION ( 'NONE',  ( 1.000000000000000000, 0.000000000000000000, 0.000000000000000000 ) ) ;
#5415 = ORIENTED_EDGE ( 'NONE', *, *, #39381, .F. ) ;
#5416 = VECTOR ( 'NONE', #26624, 1000.000000000000000 ) ;
#5417 = ADVANCED_FACE ( 'NONE', ( #17137 ), #36726, .F. ) ;
#5418 = VECTOR ( 'NONE', #421, 1000.000000000000000 ) ;
#5419 = FACE_OUTER_BOUND ( 'NONE', #15549, .T. ) ;
#5420 = CARTESIAN_POINT ( 'NONE',  ( -71.24862878704732339, 31.00000000000000711, 35.13526414049667324 ) ) ;
#5421 = AXIS2_PLACEMENT_3D ( 'NONE', #23404, #33411, #3494 ) ;
#5422 = VECTOR ( 'NONE', #24357, 1000.000000000000000 ) ;
#5423 = EDGE_CURVE ( 'NONE', #39508, #38342, #9617, .T. ) ;
#5424 = ORIENTED_EDGE ( 'NONE', *, *, #26015, .F. ) ;
#5426 = CARTESIAN_POINT ( 'NONE',  ( -51.89982240187124063, 31.00000000000000355, 3.308651922604603168 ) ) ;
#5425 = CIRCLE ( 'NONE', #20105, 31.49899999999999878 ) ;
#5427 = CARTESIAN_POINT ( 'NONE',  ( 84.89583333414414312, 39.99999999999999289, -5.563236982362012029 ) ) ;
#5428 = VERTEX_POINT ( 'NONE', #30203 ) ;
#5429 = DIRECTION ( 'NONE',  ( 1.000000000000000000, 1.836909530733573776E-16, 0.000000000000000000 ) ) ;
#5430 = AXIS2_PLACEMENT_3D ( 'NONE', #22888, #2736, #42666 ) ;
#5431 = CYLINDRICAL_SURFACE ( 'NONE', #3327, 59.00000000000000000 ) ;
#5432 = DIRECTION ( 'NONE',  ( 0.000000000000000000, 0.000000000000000000, 1.000000000000000000 ) ) ;
#5434 = ORIENTED_EDGE ( 'NONE', *, *, #301, .F. ) ;
#5433 = CARTESIAN_POINT ( 'NONE',  ( 17.99999999999999645, -40.37724737309996215, -104.6802291180871265 ) ) ;
#5435 = CARTESIAN_POINT ( 'NONE',  ( 18.00000000000000355, 6.109652351742432153, -46.58570277113501845 ) ) ;
#5436 = FACE_OUTER_BOUND ( 'NONE', #5253, .T. ) ;
#5437 = ORIENTED_EDGE ( 'NONE', *, *, #37646, .F. ) ;
#5438 = CARTESIAN_POINT ( 'NONE',  ( 62.17703816010947548, 39.99999999999999289, 21.10553973064489597 ) ) ;
#5439 = DIRECTION ( 'NONE',  ( -1.000000000000000000, 0.000000000000000000, 0.000000000000000000 ) ) ;
#5440 = ADVANCED_FACE ( 'NONE', ( #13635 ), #23249, .F. ) ;
#5441 = ORIENTED_EDGE ( 'NONE', *, *, #32084, .T. ) ;
#5442 = EDGE_CURVE ( 'NONE', #38197, #22945, #40966, .T. ) ;
#5443 = CIRCLE ( 'NONE', #36098, 14.99999999999999822 ) ;
#5444 = DIRECTION ( 'NONE',  ( -1.000000000000000000, -0.000000000000000000, -0.000000000000000000 ) ) ;
#5445 = FACE_OUTER_BOUND ( 'NONE', #7909, .T. ) ;
#5446 = ORIENTED_EDGE ( 'NONE', *, *, #36778, .F. ) ;
#5447 = AXIS2_PLACEMENT_3D ( 'NONE', #29002, #35092, #35310 ) ;
#5448 = VECTOR ( 'NONE', #8422, 1000.000000000000000 ) ;
#5449 = VERTEX_POINT ( 'NONE', #31286 ) ;
#5450 = CIRCLE ( 'NONE', #3332, 116.0000000000000000 ) ;
#5451 = CARTESIAN_POINT ( 'NONE',  ( 17.99999999999999645, 107.2703412112694963, 32.88383143828500721 ) ) ;
#5452 = VERTEX_POINT ( 'NONE', #1802 ) ;
#5453 = AXIS2_PLACEMENT_3D ( 'NONE', #39950, #22798, #39534 ) ;
#5454 = CARTESIAN_POINT ( 'NONE',  ( 0.000000000000000000, -23.85344185397118011, -113.5209818126993611 ) ) ;
#5455 = CARTESIAN_POINT ( 'NONE',  ( 8.999999999999998224, 87.74575819880170968, 75.87280091124503656 ) ) ;
#5456 = AXIS2_PLACEMENT_3D ( 'NONE', #15548, #28844, #42108 ) ;
#5457 = FACE_OUTER_BOUND ( 'NONE', #19641, .T. ) ;
#5458 = CARTESIAN_POINT ( 'NONE',  ( 2.500000000000000000, -2.357898499370432166, 3.035766082959412415E-15 ) ) ;
#5459 = ORIENTED_EDGE ( 'NONE', *, *, #16655, .F. ) ;
#5460 = DIRECTION ( 'NONE',  ( -1.000000000000000000, -0.000000000000000000, 0.000000000000000000 ) ) ;
#5461 = EDGE_CURVE ( 'NONE', #1856, #24349, #6119, .T. ) ;
#5462 = ORIENTED_EDGE ( 'NONE', *, *, #681, .F. ) ;
#5463 = DIRECTION ( 'NONE',  ( 1.000000000000000000, 0.000000000000000000, 0.000000000000000000 ) ) ;
#5464 = VERTEX_POINT ( 'NONE', #5077 ) ;
#5465 = DIRECTION ( 'NONE',  ( 0.000000000000000000, 0.000000000000000000, 1.000000000000000000 ) ) ;
#5466 = DIRECTION ( 'NONE',  ( -1.000000000000000000, 0.000000000000000000, 0.000000000000000000 ) ) ;
#5467 = DIRECTION ( 'NONE',  ( -6.123233995736766036E-17, 1.000000000000000000, 4.275831445896958607E-31 ) ) ;
#5468 = ADVANCED_FACE ( 'NONE', ( #920, #8146 ), #40627, .F. ) ;
#5469 = FACE_OUTER_BOUND ( 'NONE', #18237, .T. ) ;
#5470 = CARTESIAN_POINT ( 'NONE',  ( -36.80126402429788612, 31.00000000000000355, 32.28896105221774349 ) ) ;
#5471 = VERTEX_POINT ( 'NONE', #41505 ) ;
#5472 = CARTESIAN_POINT ( 'NONE',  ( 17.99999999999999645, -80.02407177073008882, 78.64108602299921813 ) ) ;
#5473 = EDGE_CURVE ( 'NONE', #9695, #16188, #11431, .T. ) ;
#5474 = AXIS2_PLACEMENT_3D ( 'NONE', #39378, #19792, #33058 ) ;
#5475 = ORIENTED_EDGE ( 'NONE', *, *, #6842, .T. ) ;
#5476 = AXIS2_PLACEMENT_3D ( 'NONE', #21855, #25543, #42061 ) ;
#5477 = EDGE_CURVE ( 'NONE', #27783, #7249, #18055, .T. ) ;
#5478 = CARTESIAN_POINT ( 'NONE',  ( -57.67632858778466698, 40.00000000000000711, 15.45560639130400205 ) ) ;
#5479 = VECTOR ( 'NONE', #42976, 1000.000000000000000 ) ;
#5480 = CARTESIAN_POINT ( 'NONE',  ( 1.598609366639573350E-14, -1.063425437509180407E-13, -40.00000000000000000 ) ) ;
#5481 = CARTESIAN_POINT ( 'NONE',  ( 17.99999999999999645, 97.19627249181192497, -71.22763238166385236 ) ) ;
#5482 = DIRECTION ( 'NONE',  ( 2.932542530036133930E-17, 1.000000000000000000, -5.216001792149171863E-18 ) ) ;
#5483 = DIRECTION ( 'NONE',  ( 0.000000000000000000, 0.1590634960190723812, -0.9872683547213445543 ) ) ;
#5484 = VERTEX_POINT ( 'NONE', #37591 ) ;
#5485 = CARTESIAN_POINT ( 'NONE',  ( -39.53383601736616271, 40.00000000000000000, 5.215339288884301538 ) ) ;
#5486 = ORIENTED_EDGE ( 'NONE', *, *, #4639, .F. ) ;
#5487 = DIRECTION ( 'NONE',  ( 0.000000000000000000, 0.000000000000000000, 1.000000000000000000 ) ) ;
#5488 = CARTESIAN_POINT ( 'NONE',  ( -6.999999999999999112, 4.546351088565595293E-15, 0.000000000000000000 ) ) ;
#5489 = ADVANCED_FACE ( 'NONE', ( #24109 ), #24995, .T. ) ;
#5490 = VERTEX_POINT ( 'NONE', #21283 ) ;
#5491 = EDGE_CURVE ( 'NONE', #24229, #26181, #24340, .T. ) ;
#5492 = CARTESIAN_POINT ( 'NONE',  ( 17.99999999999999645, 112.5120133921107737, 43.14554256761054063 ) ) ;
#5493 = ADVANCED_FACE ( 'NONE', ( #1151 ), #28023, .F. ) ;
#5494 = EDGE_CURVE ( 'NONE', #40931, #12750, #21545, .T. ) ;
#5495 = EDGE_LOOP ( 'NONE', ( #13359, #6931, #18177, #33037 ) ) ;
#5496 = CARTESIAN_POINT ( 'NONE',  ( 17.99999999999999645, -29.09613215194498181, 21.19941258140312357 ) ) ;
#5497 = EDGE_LOOP ( 'NONE', ( #16247, #39511, #36391, #34067 ) ) ;
#5498 = ORIENTED_EDGE ( 'NONE', *, *, #13346, .F. ) ;
#5499 = CARTESIAN_POINT ( 'NONE',  ( -10.00000000000000000, 0.000000000000000000, 0.000000000000000000 ) ) ;
#5500 = CARTESIAN_POINT ( 'NONE',  ( 5.650912336215120568, 31.00000000000000355, -84.59266001507907617 ) ) ;
#5501 = VERTEX_POINT ( 'NONE', #20859 ) ;
#5502 = CARTESIAN_POINT ( 'NONE',  ( 17.99999999999999645, 0.6819280456844267757, -115.9979955608738607 ) ) ;
#5503 = AXIS2_PLACEMENT_3D ( 'NONE', #16741, #6878, #10590 ) ;
#5504 = EDGE_CURVE ( 'NONE', #17317, #15115, #40854, .T. ) ;
#5505 = VECTOR ( 'NONE', #25907, 1000.000000000000000 ) ;
#5506 = CARTESIAN_POINT ( 'NONE',  ( 17.99999999999999645, -108.8880088604279166, 39.99251838045924501 ) ) ;
#5507 = AXIS2_PLACEMENT_3D ( 'NONE', #30612, #30391, #26685 ) ;
#5508 = VERTEX_POINT ( 'NONE', #11220 ) ;
#5509 = DIRECTION ( 'NONE',  ( -0.06345332152672161774, 0.000000000000000000, 0.9979848074931934043 ) ) ;
#5510 = DIRECTION ( 'NONE',  ( 0.000000000000000000, -0.2486898871648622333, 0.9685831611286292997 ) ) ;
#5511 = CARTESIAN_POINT ( 'NONE',  ( 20.65150112226810819, 31.00000000000000355, -15.81946110361252522 ) ) ;
#5513 = DIRECTION ( 'NONE',  ( 1.000000000000000000, 0.000000000000000000, 0.000000000000000000 ) ) ;
#5512 = CARTESIAN_POINT ( 'NONE',  ( 17.99999999999999645, 0.000000000000000000, 0.000000000000000000 ) ) ;
#5514 = DIRECTION ( 'NONE',  ( 0.000000000000000000, 0.000000000000000000, 1.000000000000000000 ) ) ;
#5515 = LINE ( 'NONE', #25199, #25032 ) ;
#5516 = ORIENTED_EDGE ( 'NONE', *, *, #41897, .F. ) ;
#5517 = EDGE_CURVE ( 'NONE', #416, #23951, #2642, .T. ) ;
#5518 = DIRECTION ( 'NONE',  ( 0.000000000000000000, 0.000000000000000000, 1.000000000000000000 ) ) ;
#5519 = VERTEX_POINT ( 'NONE', #18438 ) ;
#5520 = CYLINDRICAL_SURFACE ( 'NONE', #7318, 47.49900000000000233 ) ;
#5521 = CARTESIAN_POINT ( 'NONE',  ( -31.57754862722326905, 31.00000000000000355, 93.01713655900283584 ) ) ;
#5522 = ADVANCED_FACE ( 'NONE', ( #34319 ), #30847, .T. ) ;
#5523 = CARTESIAN_POINT ( 'NONE',  ( 17.99999999999999645, -78.75547124681429523, 91.20343606296975736 ) ) ;
#5524 = VERTEX_POINT ( 'NONE', #7491 ) ;
#5525 = CARTESIAN_POINT ( 'NONE',  ( 23.12883206328222130, 40.00000000000000000, 11.39561251172168355 ) ) ;
#5526 = CARTESIAN_POINT ( 'NONE',  ( -5.264430561742839743, 40.00000000000000000, 39.44269128746232411 ) ) ;
#5527 = EDGE_LOOP ( 'NONE', ( #27665, #5666, #16051, #9460 ) ) ;
#5528 = ORIENTED_EDGE ( 'NONE', *, *, #5609, .F. ) ;
#5529 = LINE ( 'NONE', #8164, #19998 ) ;
#5530 = CARTESIAN_POINT ( 'NONE',  ( 17.99999999999999645, 57.69704296431184787, 105.7900857083231472 ) ) ;
#5531 = CIRCLE ( 'NONE', #13931, 59.00000000000000000 ) ;
#5532 = DIRECTION ( 'NONE',  ( -1.000000000000000000, 0.000000000000000000, 0.000000000000000000 ) ) ;
#5533 = CIRCLE ( 'NONE', #2726, 116.0000000000000000 ) ;
#5534 = DIRECTION ( 'NONE',  ( 0.000000000000000000, 0.000000000000000000, 1.000000000000000000 ) ) ;
#5535 = VECTOR ( 'NONE', #11351, 1000.000000000000000 ) ;
#5536 = DIRECTION ( 'NONE',  ( 0.06345332152672161774, -5.286866677681789116E-16, -0.9979848074931934043 ) ) ;
#5537 = VERTEX_POINT ( 'NONE', #11007 ) ;
#5538 = LINE ( 'NONE', #38263, #18718 ) ;
#5539 = ORIENTED_EDGE ( 'NONE', *, *, #17119, .F. ) ;
#5540 = CYLINDRICAL_SURFACE ( 'NONE', #10363, 116.0000000000000000 ) ;
#5541 = LINE ( 'NONE', #29117, #9597 ) ;
#5542 = EDGE_CURVE ( 'NONE', #1492, #22195, #41662, .T. ) ;
#5543 = ADVANCED_FACE ( 'NONE', ( #4415 ), #37802, .F. ) ;
#5544 = DIRECTION ( 'NONE',  ( -1.000000000000000000, -0.000000000000000000, -0.000000000000000000 ) ) ;
#5545 = EDGE_CURVE ( 'NONE', #28510, #24559, #28465, .T. ) ;
#5546 = ADVANCED_FACE ( 'NONE', ( #32333 ), #41729, .T. ) ;
#5547 = DIRECTION ( 'NONE',  ( -1.000000000000000000, 0.000000000000000000, -0.000000000000000000 ) ) ;
#5548 = ORIENTED_EDGE ( 'NONE', *, *, #4554, .T. ) ;
#5549 = VERTEX_POINT ( 'NONE', #9207 ) ;
#5550 = CYLINDRICAL_SURFACE ( 'NONE', #17993, 59.00000000000000000 ) ;
#5551 = EDGE_CURVE ( 'NONE', #13205, #16464, #22221, .T. ) ;
#5552 = ORIENTED_EDGE ( 'NONE', *, *, #14770, .F. ) ;
#5554 = EDGE_LOOP ( 'NONE', ( #21862, #20945, #24916, #2774 ) ) ;
#5553 = CARTESIAN_POINT ( 'NONE',  ( 17.99999999999999645, -120.3696465864706369, 5.624871700595674540 ) ) ;
#5555 = CARTESIAN_POINT ( 'NONE',  ( -49.80813925210023996, 31.00000000000000355, -17.00652635548579994 ) ) ;
#5556 = ORIENTED_EDGE ( 'NONE', *, *, #30381, .F. ) ;
#5557 = CARTESIAN_POINT ( 'NONE',  ( 17.99999999999999645, -73.78980555658671392, 95.26571049921967926 ) ) ;
#5558 = DIRECTION ( 'NONE',  ( -1.000000000000000000, 0.000000000000000000, 0.000000000000000000 ) ) ;
#5559 = EDGE_LOOP ( 'NONE', ( #39796, #41266, #9743, #7292 ) ) ;
#5560 = CARTESIAN_POINT ( 'NONE',  ( 8.965261019434027645, 40.00000000000000000, 68.85524230650666766 ) ) ;
#5561 = AXIS2_PLACEMENT_3D ( 'NONE', #41749, #12529, #9230 ) ;
#5562 = AXIS2_PLACEMENT_3D ( 'NONE', #5499, #32116, #26217 ) ;
#5564 = CYLINDRICAL_SURFACE ( 'NONE', #32515, 15.99999999999999289 ) ;
#5563 = DIRECTION ( 'NONE',  ( -1.000000000000000000, 0.000000000000000000, 0.000000000000000000 ) ) ;
#5565 = CARTESIAN_POINT ( 'NONE',  ( 17.99999999999999645, 0.000000000000000000, 0.000000000000000000 ) ) ;
#5566 = VERTEX_POINT ( 'NONE', #18669 ) ;
#5567 = CARTESIAN_POINT ( 'NONE',  ( 8.999999999999998224, 97.97378550988308632, -62.10585602713663178 ) ) ;
#5568 = ORIENTED_EDGE ( 'NONE', *, *, #29222, .T. ) ;
#5569 = CARTESIAN_POINT ( 'NONE',  ( -15.99999999999997691, 17.11489954122026447, -4.499999999999995559 ) ) ;
#5570 = DIRECTION ( 'NONE',  ( -1.000000000000000000, -0.000000000000000000, 0.000000000000000000 ) ) ;
#5571 = CARTESIAN_POINT ( 'NONE',  ( -66.92166868300088822, 31.00000000000000711, -22.71661802240650019 ) ) ;
#5573 = CARTESIAN_POINT ( 'NONE',  ( 18.00000000000000355, 42.41764978026606769, 20.20639853260304619 ) ) ;
#5572 = CARTESIAN_POINT ( 'NONE',  ( 0.000000000000000000, 35.78484819117633720, 110.3423972910434117 ) ) ;
#5574 = ORIENTED_EDGE ( 'NONE', *, *, #5265, .F. ) ;
#5575 = EDGE_CURVE ( 'NONE', #23951, #25725, #38879, .T. ) ;
#5576 = DIRECTION ( 'NONE',  ( -1.000000000000000000, -0.000000000000000000, -0.000000000000000000 ) ) ;
#5577 = EDGE_LOOP ( 'NONE', ( #34210, #39106, #40941, #34667 ) ) ;
#5578 = DIRECTION ( 'NONE',  ( 0.000000000000000000, 0.000000000000000000, 1.000000000000000000 ) ) ;
#5579 = DIRECTION ( 'NONE',  ( 0.000000000000000000, -0.8183027759081623609, -0.5747874102144165942 ) ) ;
#5580 = CARTESIAN_POINT ( 'NONE',  ( 86.58052584568748955, 31.00000000000000000, -42.55516686010645344 ) ) ;
#5581 = CARTESIAN_POINT ( 'NONE',  ( 49.34100556531813453, 40.00000000000000000, 85.68208892729249726 ) ) ;
#5582 = DIRECTION ( 'NONE',  ( 0.000000000000000000, 0.000000000000000000, 1.000000000000000000 ) ) ;
#5583 = EDGE_LOOP ( 'NONE', ( #9345, #24294, #13935, #24520 ) ) ;
#5584 = CARTESIAN_POINT ( 'NONE',  ( 2.682243648011666703, 3.070208061305304881, -0.04852650426601266831 ) ) ;
#5585 = ORIENTED_EDGE ( 'NONE', *, *, #41064, .T. ) ;
#5586 = AXIS2_PLACEMENT_3D ( 'NONE', #18532, #1894, #31582 ) ;
#5587 = CIRCLE ( 'NONE', #31393, 59.00000000000000000 ) ;
#5589 = EDGE_LOOP ( 'NONE', ( #21616, #10933, #41941, #25454 ) ) ;
#5588 = LINE ( 'NONE', #8868, #37385 ) ;
#5590 = ADVANCED_FACE ( 'NONE', ( #22555 ), #5923, .T. ) ;
#5591 = EDGE_CURVE ( 'NONE', #8366, #38244, #5450, .T. ) ;
#5592 = DIRECTION ( 'NONE',  ( -1.000000000000000000, -0.000000000000000000, -0.000000000000000000 ) ) ;
#5593 = VERTEX_POINT ( 'NONE', #42567 ) ;
#5594 = PLANE ( 'NONE',  #34929 ) ;
#5595 = CARTESIAN_POINT ( 'NONE',  ( -103.7695705685749772, 106.4195705685765745, 10.00000000000033396 ) ) ;
#5596 = EDGE_CURVE ( 'NONE', #32579, #28564, #33319, .T. ) ;
#5597 = DIRECTION ( 'NONE',  ( 1.000000000000000000, 1.836909530733573776E-16, 0.000000000000000000 ) ) ;
#5598 = ORIENTED_EDGE ( 'NONE', *, *, #43160, .F. ) ;
#5599 = CARTESIAN_POINT ( 'NONE',  ( -6.259644161404862988E-16, -4.618802153517027165, -3.504271511726793076 ) ) ;
#5600 = DIRECTION ( 'NONE',  ( 0.000000000000000000, -0.6382441836448262684, 0.7698339834299010587 ) ) ;
#5601 = EDGE_CURVE ( 'NONE', #23828, #27222, #5515, .T. ) ;
#5603 = ORIENTED_EDGE ( 'NONE', *, *, #12813, .F. ) ;
#5602 = CARTESIAN_POINT ( 'NONE',  ( 0.000000000000000000, 0.000000000000000000, 0.000000000000000000 ) ) ;
#5604 = ORIENTED_EDGE ( 'NONE', *, *, #21562, .F. ) ;
#5605 = CARTESIAN_POINT ( 'NONE',  ( 18.00000000000000355, 22.82995208772746665, -41.06517797613638976 ) ) ;
#5606 = CARTESIAN_POINT ( 'NONE',  ( -2.687328764639638656, 3.067272167851286202, -0.05923475698270370959 ) ) ;
#5607 = CARTESIAN_POINT ( 'NONE',  ( 30.22238470470974292, 40.00000000000000000, -34.33595424619393555 ) ) ;
#5608 = CYLINDRICAL_SURFACE ( 'NONE', #18137, 31.49899999999999878 ) ;
#5609 = EDGE_CURVE ( 'NONE', #28896, #40202, #32633, .T. ) ;
#5610 = DIRECTION ( 'NONE',  ( 0.000000000000000000, 0.000000000000000000, 1.000000000000000000 ) ) ;
#5611 = VECTOR ( 'NONE', #12186, 1000.000000000000000 ) ;
#5612 = ORIENTED_EDGE ( 'NONE', *, *, #34877, .T. ) ;
#5613 = DIRECTION ( 'NONE',  ( -1.000000000000000000, 0.000000000000000000, -0.000000000000000000 ) ) ;
#5614 = ORIENTED_EDGE ( 'NONE', *, *, #42203, .T. ) ;
#5615 = CIRCLE ( 'NONE', #12610, 58.99999999999999289 ) ;
#5616 = CARTESIAN_POINT ( 'NONE',  ( 0.000000000000000000, 0.000000000000000000, 0.000000000000000000 ) ) ;
#5617 = DIRECTION ( 'NONE',  ( 0.000000000000000000, 0.9510565162951523099, 0.3090169943749515591 ) ) ;
#5618 = AXIS2_PLACEMENT_3D ( 'NONE', #9036, #5757, #22393 ) ;
#5620 = CARTESIAN_POINT ( 'NONE',  ( -19.20510714644778361, 31.00000000000000355, 33.27066566623395261 ) ) ;
#5619 = VECTOR ( 'NONE', #18121, 1000.000000000000000 ) ;
#5621 = ORIENTED_EDGE ( 'NONE', *, *, #39526, .F. ) ;
#5622 = CARTESIAN_POINT ( 'NONE',  ( -0.6666666666666651864, 4.233901974057260098, -3.300726591567081147 ) ) ;
#5623 = ORIENTED_EDGE ( 'NONE', *, *, #10507, .F. ) ;
#5624 = EDGE_CURVE ( 'NONE', #8001, #13563, #38204, .T. ) ;
#5625 = CYLINDRICAL_SURFACE ( 'NONE', #18488, 116.0000000000000000 ) ;
#5626 = CARTESIAN_POINT ( 'NONE',  ( -39.09256291070916944, 31.00000000000000355, 79.30589209199378331 ) ) ;
#5627 = DIRECTION ( 'NONE',  ( -1.000000000000000000, 1.058513553088275437E-16, 0.000000000000000000 ) ) ;
#5628 = ORIENTED_EDGE ( 'NONE', *, *, #27229, .F. ) ;
#5629 = CARTESIAN_POINT ( 'NONE',  ( 44.54779904930365575, 31.00000000000000355, -34.05916983163054113 ) ) ;
#5630 = CARTESIAN_POINT ( 'NONE',  ( 0.000000000000000000, -46.12538073176427389, 111.3235835452210125 ) ) ;
#5631 = ORIENTED_EDGE ( 'NONE', *, *, #8893, .F. ) ;
#5632 = FACE_OUTER_BOUND ( 'NONE', #15385, .T. ) ;
#5633 = AXIS2_PLACEMENT_3D ( 'NONE', #14177, #10899, #17259 ) ;
#5634 = FACE_OUTER_BOUND ( 'NONE', #19999, .T. ) ;
#5635 = CARTESIAN_POINT ( 'NONE',  ( 17.99999999999999645, 16.77566611177940104, -119.3275660838940553 ) ) ;
#5637 = ORIENTED_EDGE ( 'NONE', *, *, #5408, .T. ) ;
#5636 = LINE ( 'NONE', #16126, #11592 ) ;
#5638 = ADVANCED_FACE ( 'NONE', ( #22770 ), #38658, .F. ) ;
#5639 = CARTESIAN_POINT ( 'NONE',  ( 17.99999999999999645, 86.84764344323065188, -76.89919913989662348 ) ) ;
#5640 = VECTOR ( 'NONE', #3983, 1000.000000000000000 ) ;
#5641 = LINE ( 'NONE', #22691, #41136 ) ;
#5642 = ORIENTED_EDGE ( 'NONE', *, *, #31701, .T. ) ;
#5643 = CARTESIAN_POINT ( 'NONE',  ( -47.15756294055117337, 40.00000000000000000, -53.75246728999482571 ) ) ;
#5644 = DIRECTION ( 'NONE',  ( -1.000000000000000000, 0.000000000000000000, 0.000000000000000000 ) ) ;
#5645 = CIRCLE ( 'NONE', #35591, 59.00000000000000000 ) ;
#5646 = AXIS2_PLACEMENT_3D ( 'NONE', #9686, #36068, #2249 ) ;
#5647 = VERTEX_POINT ( 'NONE', #8783 ) ;
#5648 = DIRECTION ( 'NONE',  ( -1.000000000000000000, -0.000000000000000000, 0.000000000000000000 ) ) ;
#5649 = EDGE_CURVE ( 'NONE', #17781, #22195, #3293, .T. ) ;
#5650 = AXIS2_PLACEMENT_3D ( 'NONE', #27391, #20437, #13666 ) ;
#5651 = ORIENTED_EDGE ( 'NONE', *, *, #25524, .T. ) ;
#5652 = ADVANCED_FACE ( 'NONE', ( #2639 ), #19281, .F. ) ;
#5653 = ORIENTED_EDGE ( 'NONE', *, *, #4465, .T. ) ;
#5654 = DIRECTION ( 'NONE',  ( 0.000000000000000000, -0.3612416661871405976, -0.9324722294043605864 ) ) ;
#5655 = EDGE_LOOP ( 'NONE', ( #37834, #24385, #24160, #33284 ) ) ;
#5656 = DIRECTION ( 'NONE',  ( -1.000000000000000000, -0.000000000000000000, 0.000000000000000000 ) ) ;
#5657 = DIRECTION ( 'NONE',  ( -1.000000000000000000, -0.000000000000000000, -0.000000000000000000 ) ) ;
#5658 = EDGE_CURVE ( 'NONE', #33813, #21218, #13102, .T. ) ;
#5659 = DIRECTION ( 'NONE',  ( 0.000000000000000000, 0.000000000000000000, -1.000000000000000000 ) ) ;
#5660 = CARTESIAN_POINT ( 'NONE',  ( 0.000000000000000000, 0.000000000000000000, 0.000000000000000000 ) ) ;
#5661 = EDGE_LOOP ( 'NONE', ( #31563, #40413, #28059, #961 ) ) ;
#5662 = CARTESIAN_POINT ( 'NONE',  ( 0.000000000000000000, -31.81777574834308098, 2.898764365605205562 ) ) ;
#5663 = ORIENTED_EDGE ( 'NONE', *, *, #25017, .F. ) ;
#5664 = AXIS2_PLACEMENT_3D ( 'NONE', #33162, #19466, #29473 ) ;
#5665 = CARTESIAN_POINT ( 'NONE',  ( 0.3000000000000028200, -14.69693845669907084, -1.199999999999999956 ) ) ;
#5666 = ORIENTED_EDGE ( 'NONE', *, *, #17547, .F. ) ;
#5667 = DIRECTION ( 'NONE',  ( 1.000000000000000000, 0.000000000000000000, 0.000000000000000000 ) ) ;
#5668 = DIRECTION ( 'NONE',  ( -1.000000000000000000, 0.000000000000000000, 0.000000000000000000 ) ) ;
#5669 = EDGE_CURVE ( 'NONE', #16679, #30476, #15213, .T. ) ;
#5670 = DIRECTION ( 'NONE',  ( -1.000000000000000000, -0.000000000000000000, -0.000000000000000000 ) ) ;
#5671 = CARTESIAN_POINT ( 'NONE',  ( 34.44467569804516671, 31.00000000000000355, 44.88666365967159777 ) ) ;
#5673 = EDGE_CURVE ( 'NONE', #5841, #36212, #21921, .T. ) ;
#5672 = CIRCLE ( 'NONE', #11269, 20.00000000000000711 ) ;
#5674 = ORIENTED_EDGE ( 'NONE', *, *, #18541, .F. ) ;
#5675 = FACE_OUTER_BOUND ( 'NONE', #6334, .T. ) ;
#5676 = AXIS2_PLACEMENT_3D ( 'NONE', #36010, #8986, #38646 ) ;
#5677 = EDGE_CURVE ( 'NONE', #38358, #31625, #25666, .T. ) ;
#5678 = ORIENTED_EDGE ( 'NONE', *, *, #24651, .T. ) ;
#5679 = AXIS2_PLACEMENT_3D ( 'NONE', #16396, #39257, #28498 ) ;
#5680 = CARTESIAN_POINT ( 'NONE',  ( -27.38011802910879311, 40.00000000000000000, -55.51905197969063011 ) ) ;
#5681 = AXIS2_PLACEMENT_3D ( 'NONE', #9692, #35645, #19980 ) ;
#5682 = DIRECTION ( 'NONE',  ( -1.000000000000000000, -0.000000000000000000, -0.000000000000000000 ) ) ;
#5683 = DIRECTION ( 'NONE',  ( 0.000000000000000000, 0.000000000000000000, -1.000000000000000000 ) ) ;
#5684 = CARTESIAN_POINT ( 'NONE',  ( 22.90854556226710415, -14.05525454449572997, -74.83297477053821467 ) ) ;
#5685 = CARTESIAN_POINT ( 'NONE',  ( 0.000000000000000000, 0.000000000000000000, -5.000000000000000000 ) ) ;
#5686 = EDGE_CURVE ( 'NONE', #16407, #1606, #2213, .T. ) ;
#5687 = PRODUCT ( 'internal spur gear_iso_ISO - Internal spur gear 2M 118T 20PA 18FW ---S118S260OD 1.0AF', 'internal spur gear_iso_ISO - Internal spur gear 2M 118T 20PA 18FW ---S118S260OD 1.0AF', '', ( #10013 ) ) ;
#5688 = EDGE_LOOP ( 'NONE', ( #6430, #7483, #28678, #24186 ) ) ;
#5689 = CARTESIAN_POINT ( 'NONE',  ( -46.94946386092573221, 40.00000000000000000, 15.94926099647653928 ) ) ;
#5690 = VERTEX_POINT ( 'NONE', #25822 ) ;
#5691 = DIRECTION ( 'NONE',  ( 0.000000000000000000, 0.3140767120219429276, 0.9493976084683832806 ) ) ;
#5692 = DIRECTION ( 'NONE',  ( -1.000000000000000000, 0.000000000000000000, 0.000000000000000000 ) ) ;
#5693 = ORIENTED_EDGE ( 'NONE', *, *, #25641, .F. ) ;
#5694 = DIRECTION ( 'NONE',  ( 0.000000000000000000, 0.000000000000000000, 1.000000000000000000 ) ) ;
#5695 = ORIENTED_EDGE ( 'NONE', *, *, #8889, .T. ) ;
#5696 = LINE ( 'NONE', #38425, #33257 ) ;
#5697 = VERTEX_POINT ( 'NONE', #33617 ) ;
#5698 = ADVANCED_FACE ( 'NONE', ( #20356 ), #30363, .F. ) ;
#5699 = VERTEX_POINT ( 'NONE', #9847 ) ;
#5700 = CARTESIAN_POINT ( 'NONE',  ( 17.99999999999999645, -84.09610293794020208, -74.27057253243097534 ) ) ;
#5701 = AXIS2_PLACEMENT_3D ( 'NONE', #26543, #36544, #29835 ) ;
#5702 = CARTESIAN_POINT ( 'NONE',  ( 86.62806645044915399, 31.00000000000000000, 11.52843970785434990 ) ) ;
#5703 = VERTEX_POINT ( 'NONE', #36234 ) ;
#5704 = CARTESIAN_POINT ( 'NONE',  ( -3.999999999998910649, -1.658469974638591804, -3.531532913075256186 ) ) ;
#5705 = VECTOR ( 'NONE', #7846, 1000.000000000000000 ) ;
#5706 = EDGE_CURVE ( 'NONE', #37148, #27491, #8195, .T. ) ;
#5707 = DIRECTION ( 'NONE',  ( 0.000000000000000000, 0.000000000000000000, 1.000000000000000000 ) ) ;
#5708 = EDGE_LOOP ( 'NONE', ( #40977, #28777, #13448, #25033 ) ) ;
#5709 = DIRECTION ( 'NONE',  ( -1.000000000000000000, 0.000000000000000000, -0.000000000000000000 ) ) ;
#5710 = CARTESIAN_POINT ( 'NONE',  ( 17.99999999999999645, -67.32409792376445523, -89.75376489259431878 ) ) ;
#5711 = CIRCLE ( 'NONE', #21817, 36.00000000000000000 ) ;
#5712 = CARTESIAN_POINT ( 'NONE',  ( 0.000000000000000000, -22.66088087769196235, 21.87856208362548571 ) ) ;
#5714 = DIRECTION ( 'NONE',  ( -3.996523416598930318E-16, 2.658563593772947863E-15, 1.000000000000000000 ) ) ;
#5713 = DIRECTION ( 'NONE',  ( 0.000000000000000000, 0.000000000000000000, 1.000000000000000000 ) ) ;
#5715 = DIRECTION ( 'NONE',  ( 0.000000000000000000, 0.000000000000000000, 1.000000000000000000 ) ) ;
#5716 = CARTESIAN_POINT ( 'NONE',  ( 18.00000000000000355, 39.78933988720115877, 24.98727647985016276 ) ) ;
#5717 = VERTEX_POINT ( 'NONE', #445 ) ;
#5718 = SURFACE_SIDE_STYLE ('',( #38885 ) ) ;
#5719 = ADVANCED_FACE ( 'NONE', ( #7000 ), #36445, .F. ) ;
#5720 = ORIENTED_EDGE ( 'NONE', *, *, #1110, .F. ) ;
#5721 = FACE_OUTER_BOUND ( 'NONE', #3280, .T. ) ;
#5722 = EDGE_CURVE ( 'NONE', #11152, #9805, #41632, .T. ) ;
#5723 = DIRECTION ( 'NONE',  ( -1.000000000000000000, -0.000000000000000000, 0.000000000000000000 ) ) ;
#5724 = ORIENTED_EDGE ( 'NONE', *, *, #35189, .T. ) ;
#5725 = CARTESIAN_POINT ( 'NONE',  ( 1.799870782497353439, 40.00000000000000000, 27.39583333577991908 ) ) ;
#5726 = CARTESIAN_POINT ( 'NONE',  ( 27.04960320298795651, 40.00000000000000000, -23.64836272119224247 ) ) ;
#5727 = CIRCLE ( 'NONE', #30138, 120.5010000000000474 ) ;
#5728 = ORIENTED_EDGE ( 'NONE', *, *, #11920, .F. ) ;
#5729 = VECTOR ( 'NONE', #32575, 1000.000000000000000 ) ;
#5730 = VERTEX_POINT ( 'NONE', #9644 ) ;
#5731 = LINE ( 'NONE', #32352, #4656 ) ;
#5732 = CARTESIAN_POINT ( 'NONE',  ( 0.000000000000000000, -46.21320724403656044, 10.97699764141937173 ) ) ;
#5733 = EDGE_CURVE ( 'NONE', #27433, #9297, #27741, .T. ) ;
#5734 = CIRCLE ( 'NONE', #30145, 36.00000000000000000 ) ;
#5735 = DIRECTION ( 'NONE',  ( 0.000000000000000000, 0.000000000000000000, 1.000000000000000000 ) ) ;
#5736 = EDGE_CURVE ( 'NONE', #13228, #40785, #13367, .T. ) ;
#5737 = DIRECTION ( 'NONE',  ( 1.000000000000000000, 0.000000000000000000, 0.000000000000000000 ) ) ;
#5738 = ORIENTED_EDGE ( 'NONE', *, *, #6612, .T. ) ;
#5739 = FACE_OUTER_BOUND ( 'NONE', #17879, .T. ) ;
#5740 = ORIENTED_EDGE ( 'NONE', *, *, #21265, .T. ) ;
#5741 = DIRECTION ( 'NONE',  ( -1.000000000000000000, 0.000000000000000000, 0.000000000000000000 ) ) ;
#5742 = AXIS2_PLACEMENT_3D ( 'NONE', #29942, #7952, #41446 ) ;
#5743 = CYLINDRICAL_SURFACE ( 'NONE', #28436, 2.649999999999971934 ) ;
#5744 = DIRECTION ( 'NONE',  ( -1.000000000000000000, 0.000000000000000000, 0.000000000000000000 ) ) ;
#5745 = DIRECTION ( 'NONE',  ( 0.000000000000000000, 0.000000000000000000, 1.000000000000000000 ) ) ;
#5746 = EDGE_LOOP ( 'NONE', ( #39123, #42293, #12435, #13480 ) ) ;
#5747 = CARTESIAN_POINT ( 'NONE',  ( 83.17098260925966713, 39.99999999999999289, 48.02127090943169208 ) ) ;
#5748 = ORIENTED_EDGE ( 'NONE', *, *, #37318, .T. ) ;
#5749 = FACE_OUTER_BOUND ( 'NONE', #18210, .T. ) ;
#5750 = EDGE_CURVE ( 'NONE', #10114, #6578, #10501, .T. ) ;
#5751 = VERTEX_POINT ( 'NONE', #13806 ) ;
#5753 = ORIENTED_EDGE ( 'NONE', *, *, #40195, .T. ) ;
#5752 = DIRECTION ( 'NONE',  ( 1.000000000000000000, 0.000000000000000000, -0.000000000000000000 ) ) ;
#5754 = CARTESIAN_POINT ( 'NONE',  ( -32.53655534684842365, 31.00000000000000355, -42.55839752837237455 ) ) ;
#5755 = ADVANCED_FACE ( 'NONE', ( #20568 ), #32970, .F. ) ;
#5756 = ORIENTED_EDGE ( 'NONE', *, *, #24118, .F. ) ;
#5757 = DIRECTION ( 'NONE',  ( -1.000000000000000000, 0.000000000000000000, 0.000000000000000000 ) ) ;
#5758 = CARTESIAN_POINT ( 'NONE',  ( 17.99999999999999645, -34.45183346761128718, -10.44371441202691742 ) ) ;
#5759 = ORIENTED_EDGE ( 'NONE', *, *, #34742, .F. ) ;
#5760 = CIRCLE ( 'NONE', #38489, 10.49999999999998934 ) ;
#5761 = CARTESIAN_POINT ( 'NONE',  ( 74.90833963778730720, 39.99999999999999289, 20.17845691863183077 ) ) ;
#5762 = EDGE_CURVE ( 'NONE', #39595, #15674, #11706, .T. ) ;
#5764 = DIRECTION ( 'NONE',  ( 1.000000000000000000, 0.000000000000000000, 0.000000000000000000 ) ) ;
#5763 = FACE_OUTER_BOUND ( 'NONE', #36648, .T. ) ;
#5765 = AXIS2_PLACEMENT_3D ( 'NONE', #9733, #26334, #5600 ) ;
#5766 = DIRECTION ( 'NONE',  ( 0.000000000000000000, 0.000000000000000000, 1.000000000000000000 ) ) ;
#5767 = ORIENTED_EDGE ( 'NONE', *, *, #5575, .F. ) ;
#5768 = DIRECTION ( 'NONE',  ( 1.000000000000000000, -3.035766082959414264E-17, 0.000000000000000000 ) ) ;
#5769 = VERTEX_POINT ( 'NONE', #16659 ) ;
#5770 = DIRECTION ( 'NONE',  ( 0.000000000000000000, 0.7865515558026436871, -0.6175246149461904865 ) ) ;
#5771 = LINE ( 'NONE', #32395, #14998 ) ;
#5772 = ADVANCED_FACE ( 'NONE', ( #27102 ), #37105, .T. ) ;
#5773 = CARTESIAN_POINT ( 'NONE',  ( 62.17703816010947548, 31.00000000000000000, 21.10553973062999589 ) ) ;
#5774 = EDGE_CURVE ( 'NONE', #7155, #14112, #18026, .T. ) ;
#5776 = CARTESIAN_POINT ( 'NONE',  ( 8.999999999999998224, 32.49609705003704363, 15.49205204337285835 ) ) ;
#5775 = FACE_OUTER_BOUND ( 'NONE', #39175, .T. ) ;
#5777 = ORIENTED_EDGE ( 'NONE', *, *, #9722, .F. ) ;
#5778 = ADVANCED_FACE ( 'NONE', ( #3048 ), #29502, .F. ) ;
#5779 = EDGE_CURVE ( 'NONE', #19793, #12073, #34688, .T. ) ;
#5780 = CARTESIAN_POINT ( 'NONE',  ( 17.99999999999999645, 0.000000000000000000, 0.000000000000000000 ) ) ;
#5781 = ORIENTED_EDGE ( 'NONE', *, *, #35251, .T. ) ;
#5782 = CYLINDRICAL_SURFACE ( 'NONE', #3329, 12.49999999999993427 ) ;
#5783 = DIRECTION ( 'NONE',  ( 0.000000000000000000, 1.000000000000000000, -1.060184893785364939E-15 ) ) ;
#5784 = CARTESIAN_POINT ( 'NONE',  ( -91.21105805184879500, 31.00000000000000711, 11.89862498597365104 ) ) ;
#5785 = CARTESIAN_POINT ( 'NONE',  ( -6.060882879309179572, 40.00000000000000000, -94.40013096063921694 ) ) ;
#5786 = CARTESIAN_POINT ( 'NONE',  ( 0.000000000000000000, 0.000000000000000000, 0.000000000000000000 ) ) ;
#5787 = ADVANCED_FACE ( 'NONE', ( #30156 ), #10061, .F. ) ;
#5788 = CIRCLE ( 'NONE', #38514, 47.49900000000000233 ) ;
#5789 = ORIENTED_EDGE ( 'NONE', *, *, #12855, .F. ) ;
#5790 = CARTESIAN_POINT ( 'NONE',  ( 2.000000000000008882, 3.464101615137749945, 0.000000000000000000 ) ) ;
#5791 = ORIENTED_EDGE ( 'NONE', *, *, #25713, .T. ) ;
#5792 = DIRECTION ( 'NONE',  ( 0.000000000000000000, 0.3612416661871538093, -0.9324722294043554793 ) ) ;
#5793 = CYLINDRICAL_SURFACE ( 'NONE', #20743, 59.00000000000000000 ) ;
#5794 = DIRECTION ( 'NONE',  ( -1.000000000000000000, 0.000000000000000000, 0.000000000000000000 ) ) ;
#5795 = ORIENTED_EDGE ( 'NONE', *, *, #41227, .T. ) ;
#5796 = CYLINDRICAL_SURFACE ( 'NONE', #9845, 120.5010000000000190 ) ;
#5797 = MECHANICAL_DESIGN_GEOMETRIC_PRESENTATION_REPRESENTATION (  '', ( #10670 ), #35049 ) ;
#5798 = DIRECTION ( 'NONE',  ( -2.249565377136137858E-32, 1.224646799147353207E-16, 1.000000000000000000 ) ) ;
#5799 = EDGE_CURVE ( 'NONE', #26752, #38997, #16872, .T. ) ;
#5800 = B_SPLINE_CURVE_WITH_KNOTS ( 'NONE', 3,
 ( #35503, #5622, #29203, #42470, #12616 ),
 .UNSPECIFIED., .F., .F.,
 ( 4, 1, 4 ),
 ( 0.000000000000000000, 0.002309401076758506657, 0.004618802153517013315 ),
 .UNSPECIFIED. ) ;
#5801 = CARTESIAN_POINT ( 'NONE',  ( 6.999999999999999112, 7.118024431592597790E-15, 0.000000000000000000 ) ) ;
#5802 = CIRCLE ( 'NONE', #35111, 58.99999999999999289 ) ;
#5803 = ORIENTED_EDGE ( 'NONE', *, *, #37006, .T. ) ;
#5804 = CARTESIAN_POINT ( 'NONE',  ( -7.718844055051848230, 31.00000000000000355, -22.75659427661714673 ) ) ;
#5805 = ADVANCED_FACE ( 'NONE', ( #20799 ), #34061, .F. ) ;
#5806 = DIRECTION ( 'NONE',  ( 1.000000000000000000, 0.000000000000000000, 0.000000000000000000 ) ) ;
#5807 = ADVANCED_FACE ( 'NONE', ( #28179 ), #11597, .T. ) ;
#5809 = ORIENTED_EDGE ( 'NONE', *, *, #13030, .T. ) ;
#5808 = CARTESIAN_POINT ( 'NONE',  ( 0.000000000000000000, 3.840921266750508156, -47.34345070675165346 ) ) ;
#5810 = ORIENTED_EDGE ( 'NONE', *, *, #32657, .T. ) ;
#5811 = DIRECTION ( 'NONE',  ( -1.000000000000000000, 0.000000000000000000, -0.000000000000000000 ) ) ;
#5812 = CARTESIAN_POINT ( 'NONE',  ( 17.99999999999999645, -114.1157422997284669, 20.82300072952894610 ) ) ;
#5813 = CARTESIAN_POINT ( 'NONE',  ( -32.60815990948594134, 40.00000000000000000, 24.92795611697640368 ) ) ;
#5814 = DIRECTION ( 'NONE',  ( 0.000000000000000000, 0.000000000000000000, 1.000000000000000000 ) ) ;
#5815 = APPLICATION_CONTEXT ( 'automotive_design' ) ;
#5816 = AXIS2_PLACEMENT_3D ( 'NONE', #1379, #7714, #25004 ) ;
#5817 = FACE_OUTER_BOUND ( 'NONE', #9061, .T. ) ;
#5818 = CIRCLE ( 'NONE', #29501, 19.99999999999989342 ) ;
#5819 = DIRECTION ( 'NONE',  ( 0.000000000000000000, 0.000000000000000000, 1.000000000000000000 ) ) ;
#5820 = EDGE_LOOP ( 'NONE', ( #29759, #30479, #41113, #19566 ) ) ;
#5821 = CARTESIAN_POINT ( 'NONE',  ( 18.00000000000000355, 19.74581912682909035, -48.10512059033371912 ) ) ;
#5822 = VERTEX_POINT ( 'NONE', #14012 ) ;
#5823 = CIRCLE ( 'NONE', #7916, 59.00000000000000000 ) ;
#5824 = DIRECTION ( 'NONE',  ( 0.000000000000000000, 0.05322217484217219019, 0.9985826956767622775 ) ) ;
#5825 = CARTESIAN_POINT ( 'NONE',  ( 2.500000000000000000, 2.357898499370431722, -2.818925648462311528E-15 ) ) ;
#5826 = CARTESIAN_POINT ( 'NONE',  ( 35.10416666475790493, 31.00000000000000355, 2.290744634698880233 ) ) ;
#5827 = ORIENTED_EDGE ( 'NONE', *, *, #37104, .F. ) ;
#5828 = EDGE_CURVE ( 'NONE', #16799, #12487, #35370, .T. ) ;
#5829 = EDGE_CURVE ( 'NONE', #5268, #29453, #30590, .T. ) ;
#5830 = PRESENTATION_LAYER_ASSIGNMENT (  '', '', ( #220 ) ) ;
#5831 = EDGE_CURVE ( 'NONE', #33525, #34589, #16604, .T. ) ;
#5832 = DIRECTION ( 'NONE',  ( 0.000000000000000000, 0.000000000000000000, 1.000000000000000000 ) ) ;
#5833 = CARTESIAN_POINT ( 'NONE',  ( -23.88228986782336349, 31.00000000000000355, -89.13686966975919290 ) ) ;
#5834 = CIRCLE ( 'NONE', #41358, 31.49899999999999878 ) ;
#5835 = FACE_OUTER_BOUND ( 'NONE', #3685, .T. ) ;
#5836 = EDGE_LOOP ( 'NONE', ( #23350, #23842, #40671, #35473 ) ) ;
#5837 = CARTESIAN_POINT ( 'NONE',  ( -54.47698434024490410, 31.00000000000000355, -31.57393205620728693 ) ) ;
#5838 = CARTESIAN_POINT ( 'NONE',  ( -47.50570208456527865, 40.00000000000000000, -41.80188021843024870 ) ) ;
#5839 = CARTESIAN_POINT ( 'NONE',  ( 90.64482129758324902, 39.99999999999999289, 30.77200948131585889 ) ) ;
#5840 = CIRCLE ( 'NONE', #1634, 13.59999999999999787 ) ;
#5841 = VERTEX_POINT ( 'NONE', #34267 ) ;
#5842 = CARTESIAN_POINT ( 'NONE',  ( 18.00000000000000355, -7.162210897275384625, -51.50439529848835463 ) ) ;
#5843 = EDGE_CURVE ( 'NONE', #2052, #30264, #34476, .T. ) ;
#5844 = CARTESIAN_POINT ( 'NONE',  ( -106.4195705685749402, 106.4195705685765745, 10.00000000000033573 ) ) ;
#5845 = DIRECTION ( 'NONE',  ( -1.000000000000000000, -0.000000000000000000, -0.000000000000000000 ) ) ;
#5846 = AXIS2_PLACEMENT_3D ( 'NONE', #24235, #10672, #33575 ) ;
#5848 = EDGE_LOOP ( 'NONE', ( #31544, #20693, #103, #43110 ) ) ;
#5847 = DIRECTION ( 'NONE',  ( 0.000000000000000000, 0.000000000000000000, 1.000000000000000000 ) ) ;
#5849 = CARTESIAN_POINT ( 'NONE',  ( 0.000000000000000000, 0.000000000000000000, 0.000000000000000000 ) ) ;
#5850 = CARTESIAN_POINT ( 'NONE',  ( 0.000000000000000000, -86.84764344322910290, -76.89919913989835720 ) ) ;
#5851 = ORIENTED_EDGE ( 'NONE', *, *, #33988, .T. ) ;
#5852 = CARTESIAN_POINT ( 'NONE',  ( -68.69954721042445556, 40.00000000000000711, 39.68009708086182741 ) ) ;
#5853 = CARTESIAN_POINT ( 'NONE',  ( 0.000000000000000000, -86.84764344323014029, 76.89919913989720612 ) ) ;
#5854 = ORIENTED_EDGE ( 'NONE', *, *, #928, .T. ) ;
#5855 = DIRECTION ( 'NONE',  ( 0.000000000000000000, 0.7865515558026436871, -0.6175246149461902645 ) ) ;
#5856 = VERTEX_POINT ( 'NONE', #4819 ) ;
#5857 = ADVANCED_FACE ( 'NONE', ( #7438 ), #1530, .F. ) ;
#5858 = EDGE_CURVE ( 'NONE', #34567, #19682, #4451, .T. ) ;
#5859 = EDGE_LOOP ( 'NONE', ( #25757, #36871, #28869, #12411 ) ) ;
#5860 = CYLINDRICAL_SURFACE ( 'NONE', #35806, 31.49899999999999878 ) ;
#5861 = EDGE_LOOP ( 'NONE', ( #9888, #29025, #5866, #17663, #33632, #2883, #15285, #14965, #11068, #21017, #14636, #31968, #34644, #26739, #24899, #20985, #10597, #17857, #12493, #24025, #3609, #7439, #2340, #7771, #19177, #4080, #38224, #11326, #38416, #11989, #7759, #23096, #6700, #31297, #18169, #9717, #35060, #35677, #13259, #17066, #19691, #15400, #1205, #34130, #13559, #40054, #32215, #29386, #1229, #24819, #16915, #3994, #31718, #30401, #10083, #15416, #4065, #914, #253, #38547, #14045, #18268, #1427, #28216, #20852, #16271, #7023, #24622, #28517, #20040, #34349, #6873, #36105, #9858, #3185, #15139, #16037, #43034, #25562, #16451, #7965, #22937, #34559, #9541, #19857, #40289, #15627, #37043, #10149, #5312, #11200, #21590, #43065, #28689, #43057, #5568, #23807, #4945, #34197, #40586, #37127, #3422, #34903, #33186, #25376, #42543, #9019, #27737, #27831, #18622, #28439, #24769, #21284, #30834, #5240, #8304, #10126, #24330, #32650, #19305, #42640, #6829, #37418, #19967, #1447, #3028, #30340, #1032, #11173, #40868, #41042, #13420, #9007, #26243, #24030, #2002, #25760, #42934, #2985, #12265, #11198, #10547, #35662, #34148, #18861, #28666, #10455, #4767, #13193, #35326, #23652, #33879, #21370, #30776, #6534, #33022, #23703, #39876, #29740, #32803, #6329, #570, #34137, #36331, #3380, #18085, #29850, #43172, #10868, #32569, #16001, #28365, #25185, #30517, #8035, #32953, #15029, #7654, #17452, #19427, #26326, #22462, #8263, #4993, #24665, #9818, #17540, #28147, #10905, #21431, #32535, #5021, #27390, #37829, #5266, #41011, #27510, #11779, #24803, #5112, #697, #26447, #4050 ) ) ;
#5862 = CARTESIAN_POINT ( 'NONE',  ( 17.99999999999999645, 0.000000000000000000, 0.000000000000000000 ) ) ;
#5863 = DIRECTION ( 'NONE',  ( -1.000000000000000000, -0.000000000000000000, 0.000000000000000000 ) ) ;
#5864 = DIRECTION ( 'NONE',  ( -1.000000000000000000, 0.000000000000000000, -0.000000000000000000 ) ) ;
#5865 = CARTESIAN_POINT ( 'NONE',  ( 17.99999999999999645, -109.4038418350900059, -50.51029986767660773 ) ) ;
#5866 = ORIENTED_EDGE ( 'NONE', *, *, #11477, .T. ) ;
#5867 = CARTESIAN_POINT ( 'NONE',  ( -58.65872368235312706, -2.055254544495720648, -38.66963954070958209 ) ) ;
#5868 = PRODUCT_DEFINITION_CONTEXT ( 'detailed design', #3308, 'design' ) ;
#5869 = CIRCLE ( 'NONE', #35146, 2.649999999999985700 ) ;
#5870 = ORIENTED_EDGE ( 'NONE', *, *, #41967, .T. ) ;
#5871 = CIRCLE ( 'NONE', #39264, 20.00000000000000000 ) ;
#5872 = CARTESIAN_POINT ( 'NONE',  ( -101.9145453900124068, 40.00000000000000000, -1.407535261550463268 ) ) ;
#5873 = ORIENTED_EDGE ( 'NONE', *, *, #37787, .T. ) ;
#5874 = FACE_OUTER_BOUND ( 'NONE', #9990, .T. ) ;
#5875 = AXIS2_PLACEMENT_3D ( 'NONE', #36353, #16551, #12416 ) ;
#5876 = EDGE_CURVE ( 'NONE', #30917, #29560, #14882, .T. ) ;
#5877 = FACE_OUTER_BOUND ( 'NONE', #42942, .T. ) ;
#5878 = ITEM_DEFINED_TRANSFORMATION ( 'NONE', 'NONE', #15640,  #13552 ) ;
#5880 = AXIS2_PLACEMENT_3D ( 'NONE', #3421, #16999, #26377 ) ;
#5879 = CARTESIAN_POINT ( 'NONE',  ( -24.74979319748359785, 5.944745455504278020, 2.972870684497277427 ) ) ;
#5881 = CARTESIAN_POINT ( 'NONE',  ( 57.76613438074698337, 31.00000000000000000, -28.48799604501563110 ) ) ;
#5882 = CARTESIAN_POINT ( 'NONE',  ( 0.000000000000000000, -11.65176648920959757, -115.4133282497343487 ) ) ;
#5883 = ORIENTED_EDGE ( 'NONE', *, *, #34794, .T. ) ;
#5884 = CARTESIAN_POINT ( 'NONE',  ( -10.41556553088919834, 31.00000000000000355, 38.62046602036556209 ) ) ;
#5885 = CARTESIAN_POINT ( 'NONE',  ( -65.92798595308768483, 40.00000000000000711, 22.39357416381200849 ) ) ;
#5886 = EDGE_CURVE ( 'NONE', #37125, #35721, #27971, .T. ) ;
#5887 = CIRCLE ( 'NONE', #30294, 2.700000000000000622 ) ;
#5888 = CARTESIAN_POINT ( 'NONE',  ( 17.99999999999999645, -58.30069736313732420, 100.2847380560565256 ) ) ;
#5889 = EDGE_CURVE ( 'NONE', #3181, #5107, #40578, .T. ) ;
#5890 = FACE_OUTER_BOUND ( 'NONE', #37355, .T. ) ;
#5891 = EDGE_CURVE ( 'NONE', #26858, #8245, #24965, .T. ) ;
#5892 = CARTESIAN_POINT ( 'NONE',  ( 9.000000000000001776, -40.47821179127736713, 32.64221760512746329 ) ) ;
#5893 = CIRCLE ( 'NONE', #40701, 2.649999999999985700 ) ;
#5894 = LINE ( 'NONE', #36205, #54 ) ;
#5895 = ORIENTED_EDGE ( 'NONE', *, *, #35579, .F. ) ;
#5896 = CARTESIAN_POINT ( 'NONE',  ( 28.83751338862256119, 40.00000000000000000, -32.88701605462710376 ) ) ;
#5897 = CARTESIAN_POINT ( 'NONE',  ( 17.99999999999999645, 21.56073507908645936, 23.57770962728572428 ) ) ;
#5898 = DIRECTION ( 'NONE',  ( 0.000000000000000000, -0.1837495178165569620, -0.9829730996839042279 ) ) ;
#5899 = VERTEX_POINT ( 'NONE', #17962 ) ;
#5900 = DIRECTION ( 'NONE',  ( -1.000000000000000000, -0.000000000000000000, 0.000000000000000000 ) ) ;
#5901 = CARTESIAN_POINT ( 'NONE',  ( 17.99999999999999645, -111.7974656912330715, 9.465682155095141326 ) ) ;
#5902 = AXIS2_PLACEMENT_3D ( 'NONE', #18291, #7770, #1866 ) ;
#5903 = ORIENTED_EDGE ( 'NONE', *, *, #8793, .F. ) ;
#5904 = CARTESIAN_POINT ( 'NONE',  ( 17.99999999999999645, -9.484061862024134371, 30.03730300138978038 ) ) ;
#5905 = ORIENTED_EDGE ( 'NONE', *, *, #17284, .F. ) ;
#5906 = EDGE_CURVE ( 'NONE', #40508, #8627, #2104, .T. ) ;
#5907 = CIRCLE ( 'NONE', #9396, 47.49900000000000233 ) ;
#5908 = EDGE_CURVE ( 'NONE', #37158, #27138, #1424, .T. ) ;
#5909 = ORIENTED_EDGE ( 'NONE', *, *, #30581, .T. ) ;
#5910 = CARTESIAN_POINT ( 'NONE',  ( 17.99999999999999645, -79.18387647320821543, 84.76976882518735579 ) ) ;
#5911 = CARTESIAN_POINT ( 'NONE',  ( -82.09281090897877675, 31.00000000000000711, -5.486092462564049477 ) ) ;
#5912 = ORIENTED_EDGE ( 'NONE', *, *, #32267, .T. ) ;
#5913 = DIRECTION ( 'NONE',  ( 0.000000000000000000, 0.000000000000000000, 1.000000000000000000 ) ) ;
#5914 = DIRECTION ( 'NONE',  ( 0.000000000000000000, 0.2486898871648553500, -0.9685831611286310761 ) ) ;
#5915 = CARTESIAN_POINT ( 'NONE',  ( 0.000000000000000000, -99.97660604679919061, -67.26937820704989690 ) ) ;
#5916 = ORIENTED_EDGE ( 'NONE', *, *, #32138, .T. ) ;
#5917 = CARTESIAN_POINT ( 'NONE',  ( 0.000000000000000000, 0.000000000000000000, 0.000000000000000000 ) ) ;
#5918 = CARTESIAN_POINT ( 'NONE',  ( -101.1468392228030098, 40.00000000000000711, 13.20405500234329921 ) ) ;
#5919 = CARTESIAN_POINT ( 'NONE',  ( 17.99999999999999645, 72.00556975657703163, 86.04342158279412445 ) ) ;
#5921 = CARTESIAN_POINT ( 'NONE',  ( 1.039096088315723056E-14, -6.912265343809663812E-14, -26.00000000000000355 ) ) ;
#5920 = FACE_OUTER_BOUND ( 'NONE', #30599, .T. ) ;
#5922 = AXIS2_PLACEMENT_3D ( 'NONE', #1195, #41554, #11702 ) ;
#5923 = CYLINDRICAL_SURFACE ( 'NONE', #16631, 20.00000000000000355 ) ;
#5924 = CIRCLE ( 'NONE', #42136, 120.5010000000000332 ) ;
#5925 = EDGE_CURVE ( 'NONE', #31919, #28896, #8412, .T. ) ;
#5926 = ORIENTED_EDGE ( 'NONE', *, *, #40859, .T. ) ;
#5927 = CARTESIAN_POINT ( 'NONE',  ( -8.325335757348113930, 31.00000000000000355, -31.05587074991522201 ) ) ;
#5928 = ORIENTED_EDGE ( 'NONE', *, *, #32480, .T. ) ;
#5929 = DIRECTION ( 'NONE',  ( 1.000000000000000000, 0.000000000000000000, 0.000000000000000000 ) ) ;
#5930 = DIRECTION ( 'NONE',  ( -1.000000000000000000, 0.000000000000000000, -0.000000000000000000 ) ) ;
#5931 = ORIENTED_EDGE ( 'NONE', *, *, #16505, .T. ) ;
#5932 = AXIS2_PLACEMENT_3D ( 'NONE', #41991, #16061, #23052 ) ;
#5933 = CARTESIAN_POINT ( 'NONE',  ( -39.53383601736616271, 40.00000000000000000, 5.215339288884301538 ) ) ;
#5934 = CARTESIAN_POINT ( 'NONE',  ( 36.20216622922067984, 40.00000000000000000, 9.761693653842600682 ) ) ;
#5935 = ADVANCED_FACE ( 'NONE', ( #37749 ), #7866, .F. ) ;
#5936 = AXIS2_PLACEMENT_3D ( 'NONE', #14531, #18049, #20885 ) ;
#5937 = EDGE_LOOP ( 'NONE', ( #27562, #24563, #10407, #27378 ) ) ;
#5938 = ORIENTED_EDGE ( 'NONE', *, *, #14457, .T. ) ;
#5939 = CYLINDRICAL_SURFACE ( 'NONE', #21417, 120.5010000000000190 ) ;
#5940 = EDGE_CURVE ( 'NONE', #6854, #40629, #6995, .T. ) ;
#5941 = FACE_OUTER_BOUND ( 'NONE', #33826, .T. ) ;
#5942 = DIRECTION ( 'NONE',  ( -3.996523416598930318E-16, 2.658563593772947863E-15, 1.000000000000000000 ) ) ;
#5943 = FACE_OUTER_BOUND ( 'NONE', #35611, .T. ) ;
#5944 = CARTESIAN_POINT ( 'NONE',  ( 0.000000000000000000, 50.95304419620838843, -10.38206564895608786 ) ) ;
#5945 = CARTESIAN_POINT ( 'NONE',  ( 17.99999999999999645, 0.000000000000000000, 0.000000000000000000 ) ) ;
#5946 = ORIENTED_EDGE ( 'NONE', *, *, #30217, .T. ) ;
#5947 = DIRECTION ( 'NONE',  ( 1.000000000000000000, -0.000000000000000000, -0.000000000000000000 ) ) ;
#5948 = ORIENTED_EDGE ( 'NONE', *, *, #26794, .F. ) ;
#5949 = CARTESIAN_POINT ( 'NONE',  ( 56.25020680251638083, -12.05525454449572642, 2.972870684497274762 ) ) ;
#5950 = CARTESIAN_POINT ( 'NONE',  ( 17.99999999999999645, -6.007673836298256020, 35.49518073029995691 ) ) ;
#5951 = AXIS2_PLACEMENT_3D ( 'NONE', #40207, #708, #7261 ) ;
#5952 = DIRECTION ( 'NONE',  ( -1.000000000000000000, 0.000000000000000000, -0.000000000000000000 ) ) ;
#5953 = DIRECTION ( 'NONE',  ( 1.000000000000000000, 0.000000000000000000, 0.000000000000000000 ) ) ;
#5954 = EDGE_LOOP ( 'NONE', ( #40867, #3731, #36935, #14311 ) ) ;
#5955 = DIRECTION ( 'NONE',  ( -1.000000000000000000, -0.000000000000000000, -0.000000000000000000 ) ) ;
#5956 = AXIS2_PLACEMENT_3D ( 'NONE', #15461, #1252, #11524 ) ;
#5957 = ORIENTED_EDGE ( 'NONE', *, *, #40387, .F. ) ;
#5958 = CIRCLE ( 'NONE', #35910, 7.500000000000000000 ) ;
#5959 = CYLINDRICAL_SURFACE ( 'NONE', #35776, 20.00000000000000711 ) ;
#5960 = AXIS2_PLACEMENT_3D ( 'NONE', #881, #21237, #34072 ) ;
#5961 = EDGE_CURVE ( 'NONE', #15922, #21082, #1320, .T. ) ;
#5962 = VERTEX_POINT ( 'NONE', #3925 ) ;
#5963 = AXIS2_PLACEMENT_3D ( 'NONE', #10192, #6915, #20275 ) ;
#5965 = ORIENTED_EDGE ( 'NONE', *, *, #12721, .F. ) ;
#5964 = DIRECTION ( 'NONE',  ( -1.000000000000000000, 0.000000000000000000, -0.000000000000000000 ) ) ;
#5966 = CARTESIAN_POINT ( 'NONE',  ( -48.87578956997907653, 31.00000000000000355, 16.50293044076727611 ) ) ;
#5967 = CIRCLE ( 'NONE', #33130, 120.5010000000000190 ) ;
#5969 = ADVANCED_FACE ( 'NONE', ( #15102 ), #25977, .T. ) ;
#5968 = ORIENTED_EDGE ( 'NONE', *, *, #21175, .T. ) ;
#5970 = CARTESIAN_POINT ( 'NONE',  ( 17.99999999999999645, 107.2885202478273783, -54.86040852957203384 ) ) ;
#5971 = AXIS2_PLACEMENT_3D ( 'NONE', #27064, #34441, #1282 ) ;
#5972 = AXIS2_PLACEMENT_3D ( 'NONE', #5919, #13363, #22765 ) ;
#5973 = ORIENTED_EDGE ( 'NONE', *, *, #2844, .T. ) ;
#5974 = FACE_OUTER_BOUND ( 'NONE', #37328, .T. ) ;
#5975 = CIRCLE ( 'NONE', #35925, 10.50000000000000178 ) ;
#5976 = ORIENTED_EDGE ( 'NONE', *, *, #2308, .F. ) ;
#5977 = CARTESIAN_POINT ( 'NONE',  ( -58.00742674161275403, 40.00000000000000711, -44.63796826977546317 ) ) ;
#5979 = CARTESIAN_POINT ( 'NONE',  ( 0.000000000000000000, 8.053585752061904302, 46.81126742072025593 ) ) ;
#5978 = DIRECTION ( 'NONE',  ( -1.000000000000000000, 0.000000000000000000, 0.000000000000000000 ) ) ;
#5980 = CARTESIAN_POINT ( 'NONE',  ( 17.99999999999999645, -42.87700105098682002, 107.7847984684003393 ) ) ;
#5981 = ORIENTED_EDGE ( 'NONE', *, *, #17609, .F. ) ;
#5982 = DIRECTION ( 'NONE',  ( -1.000000000000000000, 0.000000000000000000, -0.000000000000000000 ) ) ;
#5983 = EDGE_CURVE ( 'NONE', #19271, #710, #39712, .T. ) ;
#5984 = ORIENTED_EDGE ( 'NONE', *, *, #23591, .T. ) ;
#5985 =( NAMED_UNIT ( * ) PLANE_ANGLE_UNIT ( ) SI_UNIT ( $, .RADIAN. ) );
#5986 = DIRECTION ( 'NONE',  ( 0.000000000000000000, 0.5963673585385027565, -0.8027116379309627847 ) ) ;
#5987 = DIRECTION ( 'NONE',  ( 0.000000000000000000, 0.000000000000000000, -1.000000000000000000 ) ) ;
#5988 = CARTESIAN_POINT ( 'NONE',  ( 44.85399723358655422, 31.00000000000000355, -58.47732767552992073 ) ) ;
#5990 = DIRECTION ( 'NONE',  ( 0.000000000000000000, 0.5963673585385025344, -0.8027116379309628957 ) ) ;
#5989 = DIRECTION ( 'NONE',  ( -1.000000000000000000, -0.000000000000000000, -0.000000000000000000 ) ) ;
#5991 = CIRCLE ( 'NONE', #42914, 120.5010000000000332 ) ;
#5992 = EDGE_LOOP ( 'NONE', ( #35502, #22317, #135, #35553 ) ) ;
#5993 = CIRCLE ( 'NONE', #36656, 0.2000000000000000944 ) ;
#5994 = CIRCLE ( 'NONE', #23440, 0.08401999999999715252 ) ;
#5995 = CIRCLE ( 'NONE', #38045, 20.00000000000000711 ) ;
#5996 = DIRECTION ( 'NONE',  ( 0.000000000000000000, -0.3140767120219362107, -0.9493976084683853900 ) ) ;
#5997 = EDGE_CURVE ( 'NONE', #39703, #5769, #42089, .T. ) ;
#5998 = AXIS2_PLACEMENT_3D ( 'NONE', #14518, #17803, #34335 ) ;
#5999 = ORIENTED_EDGE ( 'NONE', *, *, #24247, .F. ) ;
#6000 = LINE ( 'NONE', #19354, #10165 ) ;
#6001 = EDGE_CURVE ( 'NONE', #10513, #31219, #38336, .T. ) ;
#6002 = DIRECTION ( 'NONE',  ( -1.000000000000000000, 0.000000000000000000, 0.000000000000000000 ) ) ;
#6003 = CARTESIAN_POINT ( 'NONE',  ( -32.34013556242301490, 31.00000000000000355, 94.87070470182929682 ) ) ;
#6005 = CARTESIAN_POINT ( 'NONE',  ( 6.386360208629404234, 40.00000000000000000, 99.40013590833049761 ) ) ;
#6004 = AXIS2_PLACEMENT_3D ( 'NONE', #35091, #41640, #25530 ) ;
#6006 = CIRCLE ( 'NONE', #35951, 59.00000000000000000 ) ;
#6007 = DIRECTION ( 'NONE',  ( 0.000000000000000000, 0.000000000000000000, 1.000000000000000000 ) ) ;
#6008 = EDGE_CURVE ( 'NONE', #31470, #13399, #16796, .T. ) ;
#6009 = VERTEX_POINT ( 'NONE', #28613 ) ;
#6010 = CARTESIAN_POINT ( 'NONE',  ( 17.99999999999999645, 115.5737863835462349, 9.934782381634081005 ) ) ;
#6011 = ORIENTED_EDGE ( 'NONE', *, *, #39788, .F. ) ;
#6012 = CARTESIAN_POINT ( 'NONE',  ( 9.000000000000001776, 104.6166166098452379, -50.11350645393572023 ) ) ;
#6013 = DIRECTION ( 'NONE',  ( 0.000000000000000000, 0.000000000000000000, 1.000000000000000000 ) ) ;
#6014 = DIRECTION ( 'NONE',  ( 1.000000000000000000, 0.000000000000000000, 0.000000000000000000 ) ) ;
#6015 = ORIENTED_EDGE ( 'NONE', *, *, #42762, .T. ) ;
#6016 = LINE ( 'NONE', #13023, #11246 ) ;
#6017 = FACE_OUTER_BOUND ( 'NONE', #29939, .T. ) ;
#6018 = DIRECTION ( 'NONE',  ( -1.000000000000000000, 0.000000000000000000, 0.000000000000000000 ) ) ;
#6020 = EDGE_LOOP ( 'NONE', ( #42361, #27556, #1621, #16749 ) ) ;
#6019 = CARTESIAN_POINT ( 'NONE',  ( 18.00000000000000355, -11.90021268425522827, -45.45261810511227907 ) ) ;
#6021 = ADVANCED_FACE ( 'NONE', ( #35550 ), #25353, .F. ) ;
#6022 = CARTESIAN_POINT ( 'NONE',  ( 11.19416946702030735, 31.00000000000000355, -22.66942529387728555 ) ) ;
#6023 = EDGE_CURVE ( 'NONE', #16211, #19378, #30010, .T. ) ;
#6024 = DIRECTION ( 'NONE',  ( -1.000000000000000000, 0.000000000000000000, 0.000000000000000000 ) ) ;
#6025 = EDGE_CURVE ( 'NONE', #27337, #1059, #4925, .T. ) ;
#6026 = EDGE_CURVE ( 'NONE', #27822, #13721, #31408, .T. ) ;
#6027 = EDGE_CURVE ( 'NONE', #13915, #8937, #11896, .T. ) ;
#6028 = CIRCLE ( 'NONE', #1855, 59.00000000000000000 ) ;
#6029 = AXIS2_PLACEMENT_3D ( 'NONE', #18938, #32831, #29369 ) ;
#6031 = EDGE_LOOP ( 'NONE', ( #27869, #35477, #16575, #38468 ) ) ;
#6030 = DIRECTION ( 'NONE',  ( 0.000000000000000000, -6.982962677686266711E-15, 1.000000000000000000 ) ) ;
#6032 = ORIENTED_EDGE ( 'NONE', *, *, #35082, .T. ) ;
#6033 = DIRECTION ( 'NONE',  ( 1.000000000000000000, -1.373900992973641277E-15, -5.551115123125812284E-16 ) ) ;
#6034 = CARTESIAN_POINT ( 'NONE',  ( 17.99999999999999645, -84.77518783075045405, -73.49448960231443095 ) ) ;
#6035 = CARTESIAN_POINT ( 'NONE',  ( 38.14553738578516828, 40.00000000000000000, 29.36968266378342207 ) ) ;
#6036 = TOROIDAL_SURFACE ( 'NONE', #30435, 2.700000000000000622, 0.2000000000000000111 ) ;
#6037 = FACE_OUTER_BOUND ( 'NONE', #40237, .T. ) ;
#6038 = AXIS2_PLACEMENT_3D ( 'NONE', #13018, #39798, #20010 ) ;
#6039 = FACE_OUTER_BOUND ( 'NONE', #3478, .T. ) ;
#6040 = DIRECTION ( 'NONE',  ( -1.770125995894701942E-16, 1.000000000000000000, 0.000000000000000000 ) ) ;
#6041 = ORIENTED_EDGE ( 'NONE', *, *, #41870, .F. ) ;
#6042 = CARTESIAN_POINT ( 'NONE',  ( -1.654252653721913102, -3.663718938583024443, -0.01223254789874440342 ) ) ;
#6044 = VERTEX_POINT ( 'NONE', #25147 ) ;
#6043 = VECTOR ( 'NONE', #1627, 1000.000000000000000 ) ;
#6045 = CYLINDRICAL_SURFACE ( 'NONE', #15543, 59.00000000000000000 ) ;
#6046 = DIRECTION ( 'NONE',  ( -1.000000000000000000, 0.000000000000000000, 0.000000000000000000 ) ) ;
#6047 = AXIS2_PLACEMENT_3D ( 'NONE', #42615, #42186, #12346 ) ;
#6048 = CARTESIAN_POINT ( 'NONE',  ( 39.78947517253659072, 31.00000000000000355, -19.62497191778171413 ) ) ;
#6049 = PRESENTATION_STYLE_ASSIGNMENT (( #38984 ) ) ;
#6050 = ORIENTED_EDGE ( 'NONE', *, *, #13450, .T. ) ;
#6051 = PRODUCT_DEFINITION_SHAPE ( 'NONE', 'NONE',  #43207 ) ;
#6052 = CARTESIAN_POINT ( 'NONE',  ( 0.000000000000000000, 83.58328028049768932, -80.43528614701241963 ) ) ;
#6053 = EDGE_CURVE ( 'NONE', #9725, #24319, #18827, .T. ) ;
#6054 = CARTESIAN_POINT ( 'NONE',  ( -78.83182461418512332, 31.00000000000000711, -45.51551753872077910 ) ) ;
#6055 = DIRECTION ( 'NONE',  ( 0.000000000000000000, -0.8951632913550570114, -0.4457383557765489668 ) ) ;
#6057 = EDGE_LOOP ( 'NONE', ( #5391, #29218, #14335, #40689 ) ) ;
#6056 = AXIS2_PLACEMENT_3D ( 'NONE', #3836, #13285, #581 ) ;
#6058 = CARTESIAN_POINT ( 'NONE',  ( 49.67886955982877595, 31.00000000000000355, -43.43868092391004865 ) ) ;
#6059 = CARTESIAN_POINT ( 'NONE',  ( -38.62815422673675414, 40.00000000000000000, -50.51519254952906124 ) ) ;
#6060 = CARTESIAN_POINT ( 'NONE',  ( 0.000000000000000000, -5.667686777401384823, -46.64153600743609474 ) ) ;
#6061 = AXIS2_PLACEMENT_3D ( 'NONE', #5093, #41301, #11447 ) ;
#6062 = ORIENTED_EDGE ( 'NONE', *, *, #2691, .F. ) ;
#6063 = AXIS2_PLACEMENT_3D ( 'NONE', #15335, #1763, #11392 ) ;
#6064 = VECTOR ( 'NONE', #42646, 1000.000000000000000 ) ;
#6065 = DIRECTION ( 'NONE',  ( 0.000000000000000000, 0.000000000000000000, -1.000000000000000000 ) ) ;
#6066 = CARTESIAN_POINT ( 'NONE',  ( 17.99999999999999645, -98.39501399267926729, -53.91376164787777014 ) ) ;
#6067 = VECTOR ( 'NONE', #37399, 1000.000000000000000 ) ;
#6069 = ORIENTED_EDGE ( 'NONE', *, *, #39271, .F. ) ;
#6068 = FACE_OUTER_BOUND ( 'NONE', #25706, .T. ) ;
#6070 = DIRECTION ( 'NONE',  ( 1.000000000000000000, 0.000000000000000000, -3.273063162220425331E-16 ) ) ;
#6071 = DIRECTION ( 'NONE',  ( -1.836909530733573776E-16, 1.000000000000000000, 0.000000000000000000 ) ) ;
#6072 = CIRCLE ( 'NONE', #41606, 47.49899999999998812 ) ;
#6073 = CARTESIAN_POINT ( 'NONE',  ( 66.75446398494719347, 39.99999999999999289, -32.91950810868348043 ) ) ;
#6074 = CARTESIAN_POINT ( 'NONE',  ( 17.99999999999999645, -114.6488492393081913, 37.09625815499973100 ) ) ;
#6075 = AXIS2_PLACEMENT_3D ( 'NONE', #1148, #31284, #28458 ) ;
#6076 = ORIENTED_EDGE ( 'NONE', *, *, #9105, .T. ) ;
#6077 = DIRECTION ( 'NONE',  ( -1.000000000000000000, -0.000000000000000000, -0.000000000000000000 ) ) ;
#6078 = ADVANCED_FACE ( 'NONE', ( #5877 ), #19233, .F. ) ;
#6079 = DIRECTION ( 'NONE',  ( 0.000000000000000000, -0.7705132427757817037, -0.6374239897486988493 ) ) ;
#6080 = EDGE_CURVE ( 'NONE', #10403, #33606, #12601, .T. ) ;
#6081 = EDGE_CURVE ( 'NONE', #41098, #39261, #22374, .T. ) ;
#6082 = ORIENTED_EDGE ( 'NONE', *, *, #31959, .F. ) ;
#6083 = EDGE_CURVE ( 'NONE', #22707, #20305, #12465, .T. ) ;
#6084 = ORIENTED_EDGE ( 'NONE', *, *, #40844, .T. ) ;
#6085 = DIRECTION ( 'NONE',  ( 0.000000000000000000, 0.000000000000000000, 1.000000000000000000 ) ) ;
#6086 = ORIENTED_EDGE ( 'NONE', *, *, #13707, .T. ) ;
#6087 = CARTESIAN_POINT ( 'NONE',  ( 17.99999999999999645, 0.000000000000000000, 0.000000000000000000 ) ) ;
#6088 = PLANE ( 'NONE',  #31849 ) ;
#6089 = AXIS2_PLACEMENT_3D ( 'NONE', #38053, #5103, #8382 ) ;
#6090 = CARTESIAN_POINT ( 'NONE',  ( 9.000000000000001776, 25.61928775981106554, -45.25098998563450436 ) ) ;
#6091 = DIRECTION ( 'NONE',  ( 1.000000000000000000, 0.000000000000000000, 0.000000000000000000 ) ) ;
#6092 = VERTEX_POINT ( 'NONE', #38831 ) ;
#6093 = VECTOR ( 'NONE', #17330, 1000.000000000000000 ) ;
#6094 = CARTESIAN_POINT ( 'NONE',  ( 17.99999999999999645, 27.83061035787113369, -117.2431154827794586 ) ) ;
#6095 = AXIS2_PLACEMENT_3D ( 'NONE', #4343, #36872, #20338 ) ;
#6096 = ORIENTED_EDGE ( 'NONE', *, *, #15351, .F. ) ;
#6098 = CARTESIAN_POINT ( 'NONE',  ( 17.99999999999999645, 0.000000000000000000, 0.000000000000000000 ) ) ;
#6097 = VECTOR ( 'NONE', #28500, 1000.000000000000000 ) ;
#6099 = ORIENTED_EDGE ( 'NONE', *, *, #9535, .F. ) ;
#6100 = LINE ( 'NONE', #42307, #2236 ) ;
#6101 = AXIS2_PLACEMENT_3D ( 'NONE', #2445, #15809, #42388 ) ;
#6102 = CYLINDRICAL_SURFACE ( 'NONE', #34159, 13.59999999999999964 ) ;
#6103 = ITEM_DEFINED_TRANSFORMATION ( 'NONE', 'NONE', #30946,  #13552 ) ;
#6104 = CARTESIAN_POINT ( 'NONE',  ( 8.673617379884035472E-16, 4.618802153517012954, -5.000000000000000000 ) ) ;
#6105 = CARTESIAN_POINT ( 'NONE',  ( -19.97695672607123640, 31.00000000000000355, -58.81104016858105155 ) ) ;
#6106 = DIRECTION ( 'NONE',  ( 0.000000000000000000, 0.7525707698561353576, 0.6585113790650422017 ) ) ;
#6107 = ORIENTED_EDGE ( 'NONE', *, *, #43108, .F. ) ;
#6108 = CARTESIAN_POINT ( 'NONE',  ( -20.36888183406315278, 31.00000000000000355, -26.63352584488936614 ) ) ;
#6109 = CARTESIAN_POINT ( 'NONE',  ( 36.74538074116732389, 40.00000000000000000, -63.64477163140654170 ) ) ;
#6110 = FACE_OUTER_BOUND ( 'NONE', #5409, .T. ) ;
#6111 = FACE_OUTER_BOUND ( 'NONE', #4371, .T. ) ;
#6112 = CIRCLE ( 'NONE', #9582, 59.00000000000000000 ) ;
#6113 = CARTESIAN_POINT ( 'NONE',  ( 17.99999999999999645, 0.000000000000000000, 0.000000000000000000 ) ) ;
#6114 = CARTESIAN_POINT ( 'NONE',  ( 17.99999999999999645, 0.000000000000000000, 0.000000000000000000 ) ) ;
#6115 = CIRCLE ( 'NONE', #31894, 59.00000000000000000 ) ;
#6116 = AXIS2_PLACEMENT_3D ( 'NONE', #40128, #27290, #13994 ) ;
#6117 = ORIENTED_EDGE ( 'NONE', *, *, #10122, .F. ) ;
#6118 = CARTESIAN_POINT ( 'NONE',  ( 43.19851606872948935, 40.00000000000000000, 14.66122656362567689 ) ) ;
#6119 = CIRCLE ( 'NONE', #29169, 120.5010000000000332 ) ;
#6120 = DIRECTION ( 'NONE',  ( 1.000000000000000000, 0.000000000000000000, 0.000000000000000000 ) ) ;
#6121 = DIRECTION ( 'NONE',  ( -1.000000000000000000, 0.000000000000000000, -0.000000000000000000 ) ) ;
#6122 = CIRCLE ( 'NONE', #10304, 19.99999999999989342 ) ;
#6123 = ORIENTED_EDGE ( 'NONE', *, *, #25337, .T. ) ;
#6124 = DIRECTION ( 'NONE',  ( -1.000000000000000000, 0.000000000000000000, -0.000000000000000000 ) ) ;
#6125 = AXIS2_PLACEMENT_3D ( 'NONE', #26423, #13340, #10032 ) ;
#6126 = DIRECTION ( 'NONE',  ( 1.000000000000000000, 0.000000000000000000, 0.000000000000000000 ) ) ;
#6127 = EDGE_CURVE ( 'NONE', #19436, #17354, #696, .T. ) ;
#6128 = ORIENTED_EDGE ( 'NONE', *, *, #32748, .F. ) ;
#6129 = LINE ( 'NONE', #9394, #5479 ) ;
#6130 = EDGE_LOOP ( 'NONE', ( #35914, #39415, #8592, #13142 ) ) ;
#6131 = ADVANCED_FACE ( 'NONE', ( #25776 ), #9157, .T. ) ;
#6132 = VERTEX_POINT ( 'NONE', #22510 ) ;
#6133 = DIRECTION ( 'NONE',  ( -3.009274222672345096E-17, -1.000000000000000000, 2.455023325076454960E-18 ) ) ;
#6134 = CARTESIAN_POINT ( 'NONE',  ( 64.90225467581601038, 31.00000000000000000, 74.17428024387139374 ) ) ;
#6135 = ORIENTED_EDGE ( 'NONE', *, *, #42606, .F. ) ;
#6136 = DIRECTION ( 'NONE',  ( 0.000000000000000000, -0.4817536741017222623, 0.8763066800438598092 ) ) ;
#6137 = VECTOR ( 'NONE', #38491, 1000.000000000000000 ) ;
#6138 = DIRECTION ( 'NONE',  ( 1.000000000000000000, 0.000000000000000000, 0.000000000000000000 ) ) ;
#6139 = CARTESIAN_POINT ( 'NONE',  ( 18.00000000000000355, 24.72041153920788403, -40.55929306992662475 ) ) ;
#6140 = VERTEX_POINT ( 'NONE', #2594 ) ;
#6141 = EDGE_CURVE ( 'NONE', #28841, #16818, #35555, .T. ) ;
#6142 = FACE_OUTER_BOUND ( 'NONE', #32478, .T. ) ;
#6143 = DIRECTION ( 'NONE',  ( -1.000000000000000000, 0.000000000000000000, 0.000000000000000000 ) ) ;
#6144 = DIRECTION ( 'NONE',  ( 1.000000000000000000, 0.000000000000000000, 0.000000000000000000 ) ) ;
#6145 = ADVANCED_FACE ( 'NONE', ( #10011 ), #6102, .T. ) ;
#6146 = VECTOR ( 'NONE', #42494, 1000.000000000000000 ) ;
#6148 = DIRECTION ( 'NONE',  ( 0.000000000000000000, 0.000000000000000000, -1.000000000000000000 ) ) ;
#6147 = DIRECTION ( 'NONE',  ( -1.000000000000000000, -0.000000000000000000, 0.000000000000000000 ) ) ;
#6149 = CARTESIAN_POINT ( 'NONE',  ( -10.00000000000000000, 0.000000000000000000, 0.000000000000000000 ) ) ;
#6150 = AXIS2_PLACEMENT_3D ( 'NONE', #32255, #28791, #2132 ) ;
#6151 = ORIENTED_EDGE ( 'NONE', *, *, #16164, .T. ) ;
#6152 = CARTESIAN_POINT ( 'NONE',  ( 19.70274684888802952, 31.00000000000000355, 17.27304525429847359 ) ) ;
#6153 = AXIS2_PLACEMENT_3D ( 'NONE', #2875, #6390, #29538 ) ;
#6154 = ORIENTED_EDGE ( 'NONE', *, *, #6001, .T. ) ;
#6155 = DIRECTION ( 'NONE',  ( -1.000000000000000000, 0.000000000000000000, 0.000000000000000000 ) ) ;
#6156 = DIRECTION ( 'NONE',  ( 0.000000000000000000, -0.7705132427757817037, -0.6374239897486988493 ) ) ;
#6157 = ORIENTED_EDGE ( 'NONE', *, *, #3246, .T. ) ;
#6158 = CARTESIAN_POINT ( 'NONE',  ( 0.000000000000000000, -111.1352304691228596, 15.40237066878559524 ) ) ;
#6159 = CARTESIAN_POINT ( 'NONE',  ( -35.44024466369167925, 40.00000000000000000, -20.45798383175513635 ) ) ;
#6160 = EDGE_CURVE ( 'NONE', #39731, #1072, #21699, .T. ) ;
#6161 = CARTESIAN_POINT ( 'NONE',  ( 23.40755275317130568, 40.00000000000000000, 30.61714766194360848 ) ) ;
#6162 = ORIENTED_EDGE ( 'NONE', *, *, #39422, .T. ) ;
#6163 = ORIENTED_EDGE ( 'NONE', *, *, #319, .T. ) ;
#6164 = CARTESIAN_POINT ( 'NONE',  ( 17.99999999999999645, -95.38615066513943930, -59.07414607872924250 ) ) ;
#6165 = DIRECTION ( 'NONE',  ( 0.000000000000000000, 0.1590634960190654978, 0.9872683547213455535 ) ) ;
#6166 = FACE_OUTER_BOUND ( 'NONE', #23004, .T. ) ;
#6167 = DIRECTION ( 'NONE',  ( 0.000000000000000000, 0.000000000000000000, 1.000000000000000000 ) ) ;
#6168 = DIRECTION ( 'NONE',  ( 1.000000000000000000, 0.000000000000000000, 0.000000000000000000 ) ) ;
#6169 = VERTEX_POINT ( 'NONE', #39883 ) ;
#6170 = DIRECTION ( 'NONE',  ( 1.000000000000000000, 0.000000000000000000, 0.000000000000000000 ) ) ;
#6171 = ORIENTED_EDGE ( 'NONE', *, *, #14526, .F. ) ;
#6172 = CARTESIAN_POINT ( 'NONE',  ( 17.99999999999999645, 0.000000000000000000, 0.000000000000000000 ) ) ;
#6173 = LINE ( 'NONE', #19732, #22876 ) ;
#6174 = CIRCLE ( 'NONE', #1972, 52.00000000000000000 ) ;
#6175 = VECTOR ( 'NONE', #4287, 1000.000000000000000 ) ;
#6176 = DIRECTION ( 'NONE',  ( -1.000000000000000000, -0.000000000000000000, 0.000000000000000000 ) ) ;
#6177 = EDGE_CURVE ( 'NONE', #36925, #25806, #34881, .T. ) ;
#6178 = LINE ( 'NONE', #19523, #34500 ) ;
#6179 = VERTEX_POINT ( 'NONE', #22949 ) ;
#6180 = CARTESIAN_POINT ( 'NONE',  ( 0.000000000000000000, -29.09613215194468694, -21.19941258140352858 ) ) ;
#6181 = VERTEX_POINT ( 'NONE', #26185 ) ;
#6182 = CIRCLE ( 'NONE', #42397, 59.00000000000000000 ) ;
#6183 = EDGE_CURVE ( 'NONE', #30690, #36459, #3489, .T. ) ;
#6184 = CARTESIAN_POINT ( 'NONE',  ( 17.99999999999999645, 100.8494052988171035, 65.95368414178945216 ) ) ;
#6185 = ORIENTED_EDGE ( 'NONE', *, *, #7899, .T. ) ;
#6187 = ORIENTED_EDGE ( 'NONE', *, *, #7719, .F. ) ;
#6186 = DIRECTION ( 'NONE',  ( -1.000000000000000000, -0.000000000000000000, 0.000000000000000000 ) ) ;
#6188 = CARTESIAN_POINT ( 'NONE',  ( 56.82522199878360425, 31.00000000000000355, 7.581518937762241173 ) ) ;
#6189 = ORIENTED_EDGE ( 'NONE', *, *, #43108, .T. ) ;
#6190 = DIRECTION ( 'NONE',  ( 1.000000000000000000, 0.000000000000000000, 0.000000000000000000 ) ) ;
#6191 = ORIENTED_EDGE ( 'NONE', *, *, #1218, .T. ) ;
#6192 = EDGE_CURVE ( 'NONE', #38171, #51, #33574, .T. ) ;
#6193 = DIRECTION ( 'NONE',  ( -1.000000000000000000, -0.000000000000000000, -0.000000000000000000 ) ) ;
#6194 = ORIENTED_EDGE ( 'NONE', *, *, #1250, .T. ) ;
#6195 = CARTESIAN_POINT ( 'NONE',  ( 50.06853320189533463, 39.99999999999999289, -56.91684085114077618 ) ) ;
#6196 = EDGE_CURVE ( 'NONE', #14824, #27141, #9092, .T. ) ;
#6198 = LINE ( 'NONE', #19544, #3933 ) ;
#6197 = CYLINDRICAL_SURFACE ( 'NONE', #9850, 59.00000000000000000 ) ;
#6199 = FACE_OUTER_BOUND ( 'NONE', #13127, .T. ) ;
#6200 = VERTEX_POINT ( 'NONE', #39458 ) ;
#6201 = CARTESIAN_POINT ( 'NONE',  ( 17.99999999999999645, -84.09610293794020208, -74.27057253243097534 ) ) ;
#6202 = EDGE_LOOP ( 'NONE', ( #20790, #7046, #427, #34379 ) ) ;
#6203 = LINE ( 'NONE', #31982, #33687 ) ;
#6204 = CARTESIAN_POINT ( 'NONE',  ( -9.000000000000005329, 0.000000000000000000, 0.000000000000000000 ) ) ;
#6205 = CARTESIAN_POINT ( 'NONE',  ( -79.89583333417640176, 31.00000000000000711, 5.235987747608064957 ) ) ;
#6206 = CIRCLE ( 'NONE', #20176, 31.49899999999999523 ) ;
#6208 = DIRECTION ( 'NONE',  ( -1.000000000000000000, -0.000000000000000000, -0.000000000000000000 ) ) ;
#6207 = LINE ( 'NONE', #19553, #14969 ) ;
#6209 = CIRCLE ( 'NONE', #1318, 116.0000000000000000 ) ;
#6210 = VERTEX_POINT ( 'NONE', #13753 ) ;
#6211 = VECTOR ( 'NONE', #37128, 1000.000000000000000 ) ;
#6212 = ADVANCED_FACE ( 'NONE', ( #23359 ), #9365, .T. ) ;
#6213 = FACE_OUTER_BOUND ( 'NONE', #24577, .T. ) ;
#6214 = EDGE_CURVE ( 'NONE', #23500, #10758, #33473, .T. ) ;
#6215 = ORIENTED_EDGE ( 'NONE', *, *, #42389, .T. ) ;
#6216 = CARTESIAN_POINT ( 'NONE',  ( 17.99999999999999645, 40.13512380274120517, -113.6206972269517905 ) ) ;
#6217 = EDGE_CURVE ( 'NONE', #3164, #32065, #39038, .T. ) ;
#6218 = CARTESIAN_POINT ( 'NONE',  ( 17.99999999999999645, 35.54274411428215075, -115.1399337407602701 ) ) ;
#6219 = CARTESIAN_POINT ( 'NONE',  ( 64.90225467581601038, 31.00000000000000000, 74.17428024387139374 ) ) ;
#6220 = CARTESIAN_POINT ( 'NONE',  ( -30.16842255227261660, 40.00000000000000000, -89.21315370691763746 ) ) ;
#6221 = CARTESIAN_POINT ( 'NONE',  ( 139.5000000000000284, -2.144538195783110118E-13, -39.99999999999994316 ) ) ;
#6222 = CARTESIAN_POINT ( 'NONE',  ( -3.413765605486552168, -14.29811891091961407, -1.199999999999999956 ) ) ;
#6223 = ORIENTED_EDGE ( 'NONE', *, *, #29105, .F. ) ;
#6224 = CARTESIAN_POINT ( 'NONE',  ( 18.00000000000000355, 32.00046193115198179, -34.40241257139653186 ) ) ;
#6225 = ORIENTED_EDGE ( 'NONE', *, *, #28948, .T. ) ;
#6226 = B_SPLINE_CURVE_WITH_KNOTS ( 'NONE', 3,
 ( #39101, #22163, #31948, #15389, #22791, #28683 ),
 .UNSPECIFIED., .F., .F.,
 ( 4, 2, 4 ),
 ( 0.002365888236228001588, 0.003551327329835089319, 0.004736766423442177049 ),
 .UNSPECIFIED. ) ;
#6227 = DIRECTION ( 'NONE',  ( 0.000000000000000000, 0.1062934856473656403, -0.9943348002101370930 ) ) ;
#6228 = FACE_OUTER_BOUND ( 'NONE', #29374, .T. ) ;
#6229 = FACE_BOUND ( 'NONE', #2823, .T. ) ;
#6230 = VERTEX_POINT ( 'NONE', #36192 ) ;
#6231 = CARTESIAN_POINT ( 'NONE',  ( 17.99999999999999645, -31.48608500567871005, 0.9019157472703476230 ) ) ;
#6232 = DIRECTION ( 'NONE',  ( 0.000000000000000000, 0.9822872507286879440, 0.1873813145857285145 ) ) ;
#6233 = DIRECTION ( 'NONE',  ( 0.000000000000000000, 0.000000000000000000, 1.000000000000000000 ) ) ;
#6234 = CIRCLE ( 'NONE', #13960, 51.99999999999999289 ) ;
#6236 = ORIENTED_EDGE ( 'NONE', *, *, #26203, .T. ) ;
#6235 = FACE_OUTER_BOUND ( 'NONE', #26805, .T. ) ;
#6237 = CARTESIAN_POINT ( 'NONE',  ( 19.49047152472852673, 31.00000000000000355, -17.07028940128360261 ) ) ;
#6238 = CIRCLE ( 'NONE', #4844, 13.59999999999999787 ) ;
#6239 = DIRECTION ( 'NONE',  ( -3.996523416598930318E-16, 2.658563593772947863E-15, 1.000000000000000000 ) ) ;
#6240 = AXIS2_PLACEMENT_3D ( 'NONE', #27727, #27283, #40553 ) ;
#6241 = EDGE_CURVE ( 'NONE', #18067, #30185, #19874, .T. ) ;
#6243 = EDGE_LOOP ( 'NONE', ( #28817, #31999, #34736, #38345 ) ) ;
#6242 = CARTESIAN_POINT ( 'NONE',  ( 17.99999999999999645, -41.33768078145568836, 104.3046912715539918 ) ) ;
#6244 = VERTEX_POINT ( 'NONE', #26614 ) ;
#6245 = CARTESIAN_POINT ( 'NONE',  ( 1.798435537469519230E-14, -1.196353617197826191E-13, -44.99999999999999289 ) ) ;
#6246 = DIRECTION ( 'NONE',  ( 0.000000000000000000, 0.000000000000000000, -1.000000000000000000 ) ) ;
#6247 = CARTESIAN_POINT ( 'NONE',  ( -32.45554871466747215, 40.00000000000000000, -28.56710966684967090 ) ) ;
#6248 = DIRECTION ( 'NONE',  ( 0.000000000000000000, 0.9980267284282717810, -0.06279051952930990443 ) ) ;
#6249 = EDGE_CURVE ( 'NONE', #23796, #32501, #41851, .T. ) ;
#6250 = DIRECTION ( 'NONE',  ( -1.000000000000000000, 0.000000000000000000, -0.000000000000000000 ) ) ;
#6251 = CARTESIAN_POINT ( 'NONE',  ( 0.000000000000000000, -50.95304419620830316, 10.38206564895644313 ) ) ;
#6252 = ORIENTED_EDGE ( 'NONE', *, *, #29105, .T. ) ;
#6253 = CARTESIAN_POINT ( 'NONE',  ( 0.000000000000000000, 0.000000000000000000, -5.000000000000000888 ) ) ;
#6254 = ORIENTED_EDGE ( 'NONE', *, *, #24685, .F. ) ;
#6255 = CARTESIAN_POINT ( 'NONE',  ( 0.000000000000000000, -41.60679253225836760, 108.2814610871944581 ) ) ;
#6256 = CYLINDRICAL_SURFACE ( 'NONE', #31749, 59.00000000000000000 ) ;
#6257 = CARTESIAN_POINT ( 'NONE',  ( -47.94314659152439617, 31.00000000000000355, -16.27230485535717719 ) ) ;
#6258 = FILL_AREA_STYLE ('',( #18984 ) ) ;
#6259 = VERTEX_POINT ( 'NONE', #16825 ) ;
#6260 = DIRECTION ( 'NONE',  ( -1.000000000000000000, 0.000000000000000000, -0.000000000000000000 ) ) ;
#6261 = CARTESIAN_POINT ( 'NONE',  ( -81.55297449308174862, 31.00000000000000711, -40.20044092665353475 ) ) ;
#6262 = AXIS2_PLACEMENT_3D ( 'NONE', #5402, #18328, #31589 ) ;
#6264 = ADVANCED_FACE ( 'NONE', ( #3002 ), #30108, .T. ) ;
#6263 = AXIS2_PLACEMENT_3D ( 'NONE', #29281, #2196, #2399 ) ;
#6265 = DIRECTION ( 'NONE',  ( -1.000000000000000000, -0.000000000000000000, -0.000000000000000000 ) ) ;
#6266 = ORIENTED_EDGE ( 'NONE', *, *, #8276, .T. ) ;
#6267 = CARTESIAN_POINT ( 'NONE',  ( -20.51812799676685373, 31.00000000000000355, -60.74091093256831897 ) ) ;
#6268 = EDGE_CURVE ( 'NONE', #10288, #30398, #15426, .T. ) ;
#6269 = CARTESIAN_POINT ( 'NONE',  ( 64.03668805593822810, 39.99999999999999289, 21.85318084037336561 ) ) ;
#6270 = CARTESIAN_POINT ( 'NONE',  ( 86.04713929520032423, 39.99999999999999289, 42.41619695850760507 ) ) ;
#6271 = ORIENTED_EDGE ( 'NONE', *, *, #29299, .T. ) ;
#6272 = CARTESIAN_POINT ( 'NONE',  ( -3.540020015735593439, -2.810662092924100630, -3.602146406945814672 ) ) ;
#6273 = CARTESIAN_POINT ( 'NONE',  ( 9.000000000000001776, 19.74581912682909390, -48.10512059033372623 ) ) ;
#6274 = CARTESIAN_POINT ( 'NONE',  ( 18.00000000000000355, 0.000000000000000000, 0.000000000000000000 ) ) ;
#6275 = EDGE_CURVE ( 'NONE', #37206, #17989, #18928, .T. ) ;
#6277 = ORIENTED_EDGE ( 'NONE', *, *, #37983, .F. ) ;
#6276 = CARTESIAN_POINT ( 'NONE',  ( -10.00000000000000000, 0.000000000000000000, 130.0000000000000000 ) ) ;
#6278 = CYLINDRICAL_SURFACE ( 'NONE', #42763, 31.49899999999999878 ) ;
#6279 = DIRECTION ( 'NONE',  ( 0.000000000000000000, 0.5877852522924742473, -0.8090169943749465631 ) ) ;
#6280 = EDGE_CURVE ( 'NONE', #30344, #12090, #722, .T. ) ;
#6281 = CARTESIAN_POINT ( 'NONE',  ( -69.75709431192164800, 40.00000000000000711, -9.183449035091399537 ) ) ;
#6282 = DIRECTION ( 'NONE',  ( 0.000000000000000000, -0.9980267284282708928, -0.06279051952932446223 ) ) ;
#6283 = VERTEX_POINT ( 'NONE', #29904 ) ;
#6284 = AXIS2_PLACEMENT_3D ( 'NONE', #42309, #8728, #2369 ) ;
#6285 = CARTESIAN_POINT ( 'NONE',  ( 17.99999999999999645, -29.68570942776464960, -10.53307442156965656 ) ) ;
#6286 = DIRECTION ( 'NONE',  ( -1.000000000000000000, 0.000000000000000000, 0.000000000000000000 ) ) ;
#6287 = ORIENTED_EDGE ( 'NONE', *, *, #24453, .T. ) ;
#6288 = CIRCLE ( 'NONE', #35558, 20.00000000000000355 ) ;
#6289 = EDGE_CURVE ( 'NONE', #40994, #19328, #17513, .T. ) ;
#6290 = ORIENTED_EDGE ( 'NONE', *, *, #8562, .F. ) ;
#6291 = FACE_OUTER_BOUND ( 'NONE', #17517, .T. ) ;
#6292 = ORIENTED_EDGE ( 'NONE', *, *, #20083, .T. ) ;
#6293 = CARTESIAN_POINT ( 'NONE',  ( 8.999999999999998224, 32.49609705003727100, -15.49205204337239827 ) ) ;
#6294 = AXIS2_PLACEMENT_3D ( 'NONE', #24809, #37628, #7748 ) ;
#6295 = DIRECTION ( 'NONE',  ( 0.000000000000000000, 0.000000000000000000, 1.000000000000000000 ) ) ;
#6296 = ADVANCED_FACE ( 'NONE', ( #34429 ), #3874, .T. ) ;
#6297 = DIRECTION ( 'NONE',  ( -1.000000000000000000, -0.000000000000000000, -0.000000000000000000 ) ) ;
#6298 = CIRCLE ( 'NONE', #42510, 47.49900000000000233 ) ;
#6299 = CYLINDRICAL_SURFACE ( 'NONE', #11598, 120.5010000000000190 ) ;
#6300 = ORIENTED_EDGE ( 'NONE', *, *, #15296, .F. ) ;
#6301 = CARTESIAN_POINT ( 'NONE',  ( -91.96080130434580724, -40.05525454449572464, 14.45886780445738218 ) ) ;
#6302 = UNCERTAINTY_MEASURE_WITH_UNIT (LENGTH_MEASURE( 1.000000000000000082E-05 ), #25879, 'distance_accuracy_value', 'NONE');
#6303 = ORIENTED_EDGE ( 'NONE', *, *, #3371, .F. ) ;
#6304 = DIRECTION ( 'NONE',  ( 0.000000000000000000, 0.000000000000000000, 1.000000000000000000 ) ) ;
#6305 = EDGE_CURVE ( 'NONE', #815, #36642, #36262, .T. ) ;
#6306 = EDGE_LOOP ( 'NONE', ( #20074, #8360, #26279, #12684 ) ) ;
#6307 = CARTESIAN_POINT ( 'NONE',  ( 9.000000000000001776, -50.95304419620832448, 10.38206564895643957 ) ) ;
#6308 = CARTESIAN_POINT ( 'NONE',  ( 17.99999999999999645, 29.68570942776486987, -10.53307442156903662 ) ) ;
#6309 = SHAPE_DEFINITION_REPRESENTATION ( #2543, #13509 ) ;
#6310 = DIRECTION ( 'NONE',  ( 1.000000000000000000, 0.000000000000000000, 0.000000000000000000 ) ) ;
#6311 = CARTESIAN_POINT ( 'NONE',  ( -4.090615425948576522, 31.00000000000000355, -62.39583333438447710 ) ) ;
#6312 = ADVANCED_FACE ( 'NONE', ( #24231, #17911, #20746, #31186, #4776, #30544, #1042, #34655, #27473, #37497 ), #1275, .T. ) ;
#6313 = AXIS2_PLACEMENT_3D ( 'NONE', #19659, #32926, #16371 ) ;
#6314 = EDGE_CURVE ( 'NONE', #4637, #18138, #11931, .T. ) ;
#6315 = VERTEX_POINT ( 'NONE', #7607 ) ;
#6316 = CARTESIAN_POINT ( 'NONE',  ( -28.46928290085317315, 31.00000000000000355, -16.49637127829624106 ) ) ;
#6317 = EDGE_CURVE ( 'NONE', #26249, #2667, #4216, .T. ) ;
#6318 = EDGE_CURVE ( 'NONE', #11189, #10403, #27926, .T. ) ;
#6319 = CARTESIAN_POINT ( 'NONE',  ( -70.10416666575086708, 40.00000000000000711, -4.581489278090966621 ) ) ;
#6320 = CIRCLE ( 'NONE', #38398, 120.5010000000000332 ) ;
#6321 = AXIS2_PLACEMENT_3D ( 'NONE', #13035, #9734, #42235 ) ;
#6322 = AXIS2_PLACEMENT_3D ( 'NONE', #12977, #33242, #14058 ) ;
#6323 = CARTESIAN_POINT ( 'NONE',  ( 0.000000000000000000, 0.000000000000000000, 0.000000000000000000 ) ) ;
#6324 = DIRECTION ( 'NONE',  ( 0.000000000000000000, 0.000000000000000000, 1.000000000000000000 ) ) ;
#6325 = AXIS2_PLACEMENT_3D ( 'NONE', #17243, #41382, #11106 ) ;
#6326 = CIRCLE ( 'NONE', #36280, 4.000000000000000000 ) ;
#6327 = DIRECTION ( 'NONE',  ( 0.000000000000000000, -0.1253332335642905193, -0.9921147013144796523 ) ) ;
#6328 = CARTESIAN_POINT ( 'NONE',  ( -10.00000000000000000, 0.000000000000000000, 0.000000000000000000 ) ) ;
#6329 = ORIENTED_EDGE ( 'NONE', *, *, #30217, .F. ) ;
#6330 = CARTESIAN_POINT ( 'NONE',  ( 3.108867721649529958, 40.00000000000000000, 47.39583333474234905 ) ) ;
#6331 = FACE_OUTER_BOUND ( 'NONE', #38808, .T. ) ;
#6332 = DIRECTION ( 'NONE',  ( 0.9654856287475623855, 0.000000000000000000, -0.2604563316218754254 ) ) ;
#6333 = AXIS2_PLACEMENT_3D ( 'NONE', #8722, #9589, #22077 ) ;
#6334 = EDGE_LOOP ( 'NONE', ( #27411, #28099, #42166, #41563 ) ) ;
#6335 = DIRECTION ( 'NONE',  ( -1.000000000000000000, 0.000000000000000000, 0.000000000000000000 ) ) ;
#6336 = CYLINDRICAL_SURFACE ( 'NONE', #13874, 10.50000000000000178 ) ;
#6337 = ORIENTED_EDGE ( 'NONE', *, *, #19099, .F. ) ;
#6338 = FACE_OUTER_BOUND ( 'NONE', #7420, .T. ) ;
#6339 = ORIENTED_EDGE ( 'NONE', *, *, #41841, .F. ) ;
#6340 = ORIENTED_EDGE ( 'NONE', *, *, #4345, .T. ) ;
#6341 = CARTESIAN_POINT ( 'NONE',  ( 17.99999999999999645, 22.66088087769211157, -21.87856208362532939 ) ) ;
#6342 = CARTESIAN_POINT ( 'NONE',  ( 49.34100556531812742, 31.00000000000000355, 85.68208892729249726 ) ) ;
#6343 = VERTEX_POINT ( 'NONE', #41181 ) ;
#6344 = DIRECTION ( 'NONE',  ( -1.000000000000000000, -0.000000000000000000, -0.000000000000000000 ) ) ;
#6345 = EDGE_CURVE ( 'NONE', #30314, #10921, #28647, .T. ) ;
#6346 = DIRECTION ( 'NONE',  ( 0.000000000000000000, 0.000000000000000000, -1.000000000000000000 ) ) ;
#6347 = EDGE_CURVE ( 'NONE', #41792, #18580, #7166, .T. ) ;
#6348 = AXIS2_PLACEMENT_3D ( 'NONE', #21771, #18491, #17628 ) ;
#6349 = CYLINDRICAL_SURFACE ( 'NONE', #36598, 59.00000000000000000 ) ;
#6350 = ORIENTED_EDGE ( 'NONE', *, *, #8955, .F. ) ;
#6351 = CARTESIAN_POINT ( 'NONE',  ( 17.99999999999999645, 0.000000000000000000, 0.000000000000000000 ) ) ;
#6352 = CIRCLE ( 'NONE', #40476, 15.99999999999998934 ) ;
#6353 = DIRECTION ( 'NONE',  ( -1.000000000000000000, 0.000000000000000000, 0.000000000000000000 ) ) ;
#6355 = DIRECTION ( 'NONE',  ( -1.000000000000000000, 0.000000000000000000, 0.000000000000000000 ) ) ;
#6354 = LINE ( 'NONE', #28864, #40518 ) ;
#6356 = VECTOR ( 'NONE', #35888, 1000.000000000000000 ) ;
#6357 = DIRECTION ( 'NONE',  ( 1.000000000000000000, -3.469446951953614189E-17, 0.000000000000000000 ) ) ;
#6358 = ORIENTED_EDGE ( 'NONE', *, *, #39652, .T. ) ;
#6359 = CARTESIAN_POINT ( 'NONE',  ( -7.231618336280544845, 31.00000000000000355, 27.02512817425793656 ) ) ;
#6360 = AXIS2_PLACEMENT_3D ( 'NONE', #6405, #12555, #16478 ) ;
#6361 = ORIENTED_EDGE ( 'NONE', *, *, #26526, .F. ) ;
#6362 = DIRECTION ( 'NONE',  ( -1.000000000000000000, 0.000000000000000000, 0.000000000000000000 ) ) ;
#6363 = DIRECTION ( 'NONE',  ( 0.000000000000000000, 0.000000000000000000, 1.000000000000000000 ) ) ;
#6364 = EDGE_LOOP ( 'NONE', ( #10639, #808, #37020, #513 ) ) ;
#6365 = EDGE_CURVE ( 'NONE', #7922, #11917, #40531, .T. ) ;
#6366 = EDGE_CURVE ( 'NONE', #27833, #27156, #26546, .T. ) ;
#6367 = FACE_OUTER_BOUND ( 'NONE', #11408, .T. ) ;
#6368 = CARTESIAN_POINT ( 'NONE',  ( -29.26739590608564967, 40.00000000000000000, 25.68069354617348665 ) ) ;
#6369 = CARTESIAN_POINT ( 'NONE',  ( -6.590854309045714565, 40.00000000000000000, 49.37518673228670707 ) ) ;
#6370 = EDGE_CURVE ( 'NONE', #33962, #3149, #8326, .T. ) ;
#6371 = ORIENTED_EDGE ( 'NONE', *, *, #8792, .F. ) ;
#6372 = ORIENTED_EDGE ( 'NONE', *, *, #37248, .F. ) ;
#6373 = CYLINDRICAL_SURFACE ( 'NONE', #8190, 0.7500000000000006661 ) ;
#6374 = LINE ( 'NONE', #23217, #42109 ) ;
#6375 = CYLINDRICAL_SURFACE ( 'NONE', #36366, 15.00000000000000000 ) ;
#6376 = CARTESIAN_POINT ( 'NONE',  ( 17.99999999999999645, 0.000000000000000000, 0.000000000000000000 ) ) ;
#6377 = ORIENTED_EDGE ( 'NONE', *, *, #16253, .F. ) ;
#6378 = CARTESIAN_POINT ( 'NONE',  ( 17.99999999999999645, -57.40245293794601622, -96.40140491896693220 ) ) ;
#6379 = ORIENTED_EDGE ( 'NONE', *, *, #2911, .T. ) ;
#6380 = LINE ( 'NONE', #16682, #25062 ) ;
#6381 = AXIS2_PLACEMENT_3D ( 'NONE', #35166, #31694, #1795 ) ;
#6382 = CARTESIAN_POINT ( 'NONE',  ( 17.99999999999999645, 0.000000000000000000, 0.000000000000000000 ) ) ;
#6383 = CIRCLE ( 'NONE', #12000, 4.500000000000002665 ) ;
#6384 = ADVANCED_FACE ( 'NONE', ( #31398 ), #37701, .F. ) ;
#6385 = VERTEX_POINT ( 'NONE', #7820 ) ;
#6386 = CARTESIAN_POINT ( 'NONE',  ( 17.99999999999999645, 84.77518783075197462, -73.49448960231268302 ) ) ;
#6387 = CIRCLE ( 'NONE', #2201, 116.0000000000000000 ) ;
#6388 = DIRECTION ( 'NONE',  ( -1.000000000000000000, -0.000000000000000000, -0.000000000000000000 ) ) ;
#6389 = ORIENTED_EDGE ( 'NONE', *, *, #22877, .F. ) ;
#6390 = DIRECTION ( 'NONE',  ( -1.000000000000000000, -0.000000000000000000, -0.000000000000000000 ) ) ;
#6391 = ORIENTED_EDGE ( 'NONE', *, *, #24742, .T. ) ;
#6392 = DIRECTION ( 'NONE',  ( 1.000000000000000000, 0.000000000000000000, 0.000000000000000000 ) ) ;
#6393 = AXIS2_PLACEMENT_3D ( 'NONE', #19702, #32967, #26443 ) ;
#6394 = VERTEX_POINT ( 'NONE', #17471 ) ;
#6396 = ORIENTED_EDGE ( 'NONE', *, *, #41089, .F. ) ;
#6395 = LINE ( 'NONE', #9244, #41776 ) ;
#6397 = CARTESIAN_POINT ( 'NONE',  ( 18.91139405008774688, 31.00000000000000355, 55.99505798891475195 ) ) ;
#6398 = ORIENTED_EDGE ( 'NONE', *, *, #19618, .F. ) ;
#6399 = CARTESIAN_POINT ( 'NONE',  ( -4.000000000000000000, -2.309401076758512694, -3.433295621305382461 ) ) ;
#6400 = ORIENTED_EDGE ( 'NONE', *, *, #15539, .F. ) ;
#6401 = CYLINDRICAL_SURFACE ( 'NONE', #9809, 10.49999999999998934 ) ;
#6402 = PRODUCT_DEFINITION_SHAPE ( 'NONE', 'NONE',  #2408 ) ;
#6403 = VERTEX_POINT ( 'NONE', #37059 ) ;
#6404 = CARTESIAN_POINT ( 'NONE',  ( 86.62806645044916820, 39.99999999999999289, 11.52843970785434990 ) ) ;
#6406 = DIRECTION ( 'NONE',  ( 1.000000000000000000, 0.000000000000000000, 0.000000000000000000 ) ) ;
#6405 = CARTESIAN_POINT ( 'NONE',  ( 22.90854556226722138, -12.05525454449572464, -74.83297477053847047 ) ) ;
#6407 = LINE ( 'NONE', #25875, #1086 ) ;
#6408 = VERTEX_POINT ( 'NONE', #30749 ) ;
#6409 = DIRECTION ( 'NONE',  ( -1.000000000000000000, 0.000000000000000000, 0.000000000000000000 ) ) ;
#6410 = VERTEX_POINT ( 'NONE', #11328 ) ;
#6411 = APPLICATION_PROTOCOL_DEFINITION ( 'draft international standard', 'automotive_design', 1998, #33406 ) ;
#6412 = CARTESIAN_POINT ( 'NONE',  ( 0.000000000000000000, -35.78425302087541127, 3.935382540232673865 ) ) ;
#6413 = DIRECTION ( 'NONE',  ( 3.996523416598930318E-16, -2.658563593772947863E-15, -1.000000000000000000 ) ) ;
#6414 = CIRCLE ( 'NONE', #30821, 125.9999999999993605 ) ;
#6415 = CARTESIAN_POINT ( 'NONE',  ( -53.76583044639610165, 31.00000000000000355, -61.28633540801820345 ) ) ;
#6417 = CARTESIAN_POINT ( 'NONE',  ( 17.99999999999999645, 0.000000000000000000, 0.000000000000000000 ) ) ;
#6416 = CARTESIAN_POINT ( 'NONE',  ( 0.000000000000000000, -22.43957647427189528, 41.27978878573620847 ) ) ;
#6418 = VERTEX_POINT ( 'NONE', #20521 ) ;
#6419 = ADVANCED_FACE ( 'NONE', ( #37916 ), #36300, .T. ) ;
#6420 = DIRECTION ( 'NONE',  ( 1.000000000000000000, 0.000000000000000000, -0.000000000000000000 ) ) ;
#6421 = AXIS2_PLACEMENT_3D ( 'NONE', #28821, #2794, #5465 ) ;
#6422 = ORIENTED_EDGE ( 'NONE', *, *, #21583, .T. ) ;
#6423 = CARTESIAN_POINT ( 'NONE',  ( 0.000000000000000000, 20.99948489194422763, 42.60488980472788256 ) ) ;
#6424 = CARTESIAN_POINT ( 'NONE',  ( 0.000000000000000000, -32.00046193115174731, 34.40241257139675923 ) ) ;
#6425 = CARTESIAN_POINT ( 'NONE',  ( -12.22491041698737746, 31.00000000000000355, -93.69500887688226953 ) ) ;
#6426 = EDGE_CURVE ( 'NONE', #39003, #38848, #32789, .T. ) ;
#6427 = DIRECTION ( 'NONE',  ( -0.000000000000000000, -0.000000000000000000, -1.000000000000000000 ) ) ;
#6428 = EDGE_CURVE ( 'NONE', #34324, #10921, #14008, .T. ) ;
#6429 = DIRECTION ( 'NONE',  ( 0.000000000000000000, 0.8443279255020161855, -0.5358267949789946583 ) ) ;
#6430 = ORIENTED_EDGE ( 'NONE', *, *, #38552, .T. ) ;
#6431 = DIRECTION ( 'NONE',  ( 1.000000000000000000, 0.000000000000000000, 0.000000000000000000 ) ) ;
#6432 = EDGE_LOOP ( 'NONE', ( #4650, #35982, #42516, #3049 ) ) ;
#6433 = CYLINDRICAL_SURFACE ( 'NONE', #16573, 116.0000000000000000 ) ;
#6434 = EDGE_CURVE ( 'NONE', #33305, #19546, #15121, .T. ) ;
#6435 = CARTESIAN_POINT ( 'NONE',  ( 0.000000000000000000, 63.24564713401931471, -102.5693868539688793 ) ) ;
#6436 = LINE ( 'NONE', #3366, #3113 ) ;
#6437 = ORIENTED_EDGE ( 'NONE', *, *, #41282, .T. ) ;
#6438 = DIRECTION ( 'NONE',  ( 1.000000000000000000, 0.000000000000000000, 0.000000000000000000 ) ) ;
#6439 = FACE_OUTER_BOUND ( 'NONE', #25381, .T. ) ;
#6440 = CIRCLE ( 'NONE', #30849, 58.99999999999999289 ) ;
#6441 = CYLINDRICAL_SURFACE ( 'NONE', #42421, 59.00000000000000000 ) ;
#6443 = VERTEX_POINT ( 'NONE', #15626 ) ;
#6442 = DIRECTION ( 'NONE',  ( -1.000000000000000000, 0.000000000000000000, 0.000000000000000000 ) ) ;
#6444 = CARTESIAN_POINT ( 'NONE',  ( -31.36635120280995537, 31.00000000000000355, -8.451140850656344128 ) ) ;
#6445 = DIRECTION ( 'NONE',  ( -3.996523416598930318E-16, 2.658563593772947863E-15, 1.000000000000000000 ) ) ;
#6447 = VERTEX_POINT ( 'NONE', #15845 ) ;
#6446 = LINE ( 'NONE', #16528, #2113 ) ;
#6448 = ORIENTED_EDGE ( 'NONE', *, *, #24907, .T. ) ;
#6449 = CARTESIAN_POINT ( 'NONE',  ( 17.99999999999999645, 31.81777574834305966, 10.70123563439457293 ) ) ;
#6450 = EDGE_CURVE ( 'NONE', #11670, #7587, #28131, .T. ) ;
#6451 = DIRECTION ( 'NONE',  ( -1.000000000000000000, -0.000000000000000000, -0.000000000000000000 ) ) ;
#6453 = CARTESIAN_POINT ( 'NONE',  ( 50.61746024623599993, 40.00000000000000000, -24.85206051842255093 ) ) ;
#6452 = AXIS2_PLACEMENT_3D ( 'NONE', #4097, #9799, #10456 ) ;
#6454 = DIRECTION ( 'NONE',  ( 0.000000000000000000, 0.000000000000000000, 1.000000000000000000 ) ) ;
#6455 = DIRECTION ( 'NONE',  ( 1.000000000000000000, 0.000000000000000000, 0.000000000000000000 ) ) ;
#6456 = DIRECTION ( 'NONE',  ( 0.000000000000000000, -0.3612416661871404866, -0.9324722294043605864 ) ) ;
#6457 = EDGE_LOOP ( 'NONE', ( #24731, #2631, #43148, #11821 ) ) ;
#6458 = CARTESIAN_POINT ( 'NONE',  ( 17.99999999999999645, 0.5156212287294736907, -112.1962860721878315 ) ) ;
#6459 = VERTEX_POINT ( 'NONE', #9704 ) ;
#6460 = DIRECTION ( 'NONE',  ( -1.000000000000000000, 0.000000000000000000, -0.000000000000000000 ) ) ;
#6461 = FACE_OUTER_BOUND ( 'NONE', #24266, .T. ) ;
#6462 = CARTESIAN_POINT ( 'NONE',  ( 3.436116956419347002, 31.00000000000000355, -52.60416666537189911 ) ) ;
#6463 = FACE_OUTER_BOUND ( 'NONE', #117, .T. ) ;
#6464 = ORIENTED_EDGE ( 'NONE', *, *, #19880, .F. ) ;
#6465 = DIRECTION ( 'NONE',  ( -3.009274222672345096E-17, -1.000000000000000000, 2.455023325076454960E-18 ) ) ;
#6466 = ORIENTED_EDGE ( 'NONE', *, *, #19144, .T. ) ;
#6467 = AXIS2_PLACEMENT_3D ( 'NONE', #15223, #18494, #24602 ) ;
#6468 = CARTESIAN_POINT ( 'NONE',  ( -55.79431841392906222, 31.00000000000000355, -72.71543055464235294 ) ) ;
#6469 = CARTESIAN_POINT ( 'NONE',  ( -4.211140560182196957, -2.431303136016552013, -3.745885042887436178 ) ) ;
#6470 = VERTEX_POINT ( 'NONE', #18931 ) ;
#6471 = CARTESIAN_POINT ( 'NONE',  ( -4.113979049837550583, 31.00000000000000355, -64.40000927351897531 ) ) ;
#6472 = CARTESIAN_POINT ( 'NONE',  ( -4.660665814384791439, 40.00000000000000000, 69.59371722953135020 ) ) ;
#6473 = CARTESIAN_POINT ( 'NONE',  ( 63.67823170517923614, 39.99999999999999289, 72.58713758494482704 ) ) ;
#6474 = EDGE_CURVE ( 'NONE', #7274, #2948, #3902, .T. ) ;
#6475 = ORIENTED_EDGE ( 'NONE', *, *, #12603, .T. ) ;
#6476 = VERTEX_POINT ( 'NONE', #38720 ) ;
#6477 = AXIS2_PLACEMENT_3D ( 'NONE', #32874, #40038, #327 ) ;
#6478 = CARTESIAN_POINT ( 'NONE',  ( -0.5636800770129166693, -4.293361309317430319, -3.531542292955206275 ) ) ;
#6479 = DIRECTION ( 'NONE',  ( -1.000000000000000000, 0.000000000000000000, 0.000000000000000000 ) ) ;
#6480 = DIRECTION ( 'NONE',  ( -1.000000000000000000, 0.000000000000000000, 0.000000000000000000 ) ) ;
#6482 = ORIENTED_EDGE ( 'NONE', *, *, #21725, .T. ) ;
#6481 = CARTESIAN_POINT ( 'NONE',  ( 18.00000000000000355, -34.03046037009231384, -33.13733193845841640 ) ) ;
#6483 = EDGE_CURVE ( 'NONE', #6869, #38968, #9266, .T. ) ;
#6484 = DIRECTION ( 'NONE',  ( -1.000000000000000000, -0.000000000000000000, 0.000000000000000000 ) ) ;
#6485 = ORIENTED_EDGE ( 'NONE', *, *, #37444, .F. ) ;
#6486 = CARTESIAN_POINT ( 'NONE',  ( -104.8158553526607477, 40.00000000000000711, 3.963965400206364453 ) ) ;
#6487 = CARTESIAN_POINT ( 'NONE',  ( -39.25113411183426848, 40.00000000000000000, 67.98392962655870519 ) ) ;
#6488 = CARTESIAN_POINT ( 'NONE',  ( 18.00000000000000355, 22.82995208772746665, -41.06517797613638976 ) ) ;
#6489 = VERTEX_POINT ( 'NONE', #2482 ) ;
#6490 = CYLINDRICAL_SURFACE ( 'NONE', #34537, 59.00000000000000000 ) ;
#6491 = DIRECTION ( 'NONE',  ( -1.734723475976807834E-16, 1.000000000000000000, 0.000000000000000000 ) ) ;
#6492 = VERTEX_POINT ( 'NONE', #32190 ) ;
#6493 = VECTOR ( 'NONE', #4117, 1000.000000000000000 ) ;
#6494 = ORIENTED_EDGE ( 'NONE', *, *, #35349, .T. ) ;
#6495 = DIRECTION ( 'NONE',  ( 0.000000000000000000, -0.7980172272802321665, -0.6026346363792660643 ) ) ;
#6497 = ORIENTED_EDGE ( 'NONE', *, *, #13001, .T. ) ;
#6496 = EDGE_CURVE ( 'NONE', #38321, #32995, #8827, .T. ) ;
#6498 = LINE ( 'NONE', #810, #23474 ) ;
#6499 = FACE_OUTER_BOUND ( 'NONE', #31306, .T. ) ;
#6500 = DIRECTION ( 'NONE',  ( -1.000000000000000000, 0.000000000000000000, 0.000000000000000000 ) ) ;
#6501 = EDGE_CURVE ( 'NONE', #16404, #24756, #26958, .T. ) ;
#6502 = CARTESIAN_POINT ( 'NONE',  ( 18.00000000000000355, 20.99948489194481738, -42.60488980472760545 ) ) ;
#6503 = DIRECTION ( 'NONE',  ( -1.000000000000000000, 0.000000000000000000, -0.000000000000000000 ) ) ;
#6504 = VERTEX_POINT ( 'NONE', #2269 ) ;
#6506 = LINE ( 'NONE', #154, #28668 ) ;
#6505 = STYLED_ITEM ( 'NONE', ( #31931 ), #4160 ) ;
#6507 = ORIENTED_EDGE ( 'NONE', *, *, #22971, .T. ) ;
#6508 = VECTOR ( 'NONE', #16715, 1000.000000000000000 ) ;
#6509 = DIRECTION ( 'NONE',  ( -1.847415842360817977E-16, 1.000000000000000000, 0.000000000000000000 ) ) ;
#6510 = DIRECTION ( 'NONE',  ( -1.000000000000000000, 0.000000000000000000, -0.000000000000000000 ) ) ;
#6511 = ORIENTED_EDGE ( 'NONE', *, *, #38520, .T. ) ;
#6512 = CARTESIAN_POINT ( 'NONE',  ( 0.000000000000000000, -84.62908780824929522, 85.78116633471262276 ) ) ;
#6513 = DIRECTION ( 'NONE',  ( 1.000000000000000000, 0.000000000000000000, 0.000000000000000000 ) ) ;
#6514 = AXIS2_PLACEMENT_3D ( 'NONE', #16242, #22809, #19318 ) ;
#6515 = APPLICATION_PROTOCOL_DEFINITION ( 'draft international standard', 'automotive_design', 1998, #26721 ) ;
#6516 = LINE ( 'NONE', #2596, #21224 ) ;
#6517 = CARTESIAN_POINT ( 'NONE',  ( -7.547223091130065953, 31.00000000000000355, 57.33767041057931380 ) ) ;
#6518 = CIRCLE ( 'NONE', #31613, 59.00000000000000000 ) ;
#6519 = ORIENTED_EDGE ( 'NONE', *, *, #36834, .T. ) ;
#6520 = CARTESIAN_POINT ( 'NONE',  ( -17.88900094061790469, 31.00000000000000355, 36.12696699725170646 ) ) ;
#6521 = AXIS2_PLACEMENT_3D ( 'NONE', #34015, #4101, #24450 ) ;
#6522 = CARTESIAN_POINT ( 'NONE',  ( 57.13603463884887645, 40.00000000000000000, 32.98675068510902264 ) ) ;
#6523 = EDGE_CURVE ( 'NONE', #35253, #41289, #42837, .T. ) ;
#6524 = CARTESIAN_POINT ( 'NONE',  ( 4.121423858225410797, -12.61643262889541006, 0.000000000000000000 ) ) ;
#6525 = EDGE_CURVE ( 'NONE', #40651, #35461, #23491, .T. ) ;
#6526 = CARTESIAN_POINT ( 'NONE',  ( 17.99999999999999645, 98.39501399267960835, -53.91376164787712355 ) ) ;
#6527 = CYLINDRICAL_SURFACE ( 'NONE', #29996, 116.0000000000000000 ) ;
#6528 = AXIS2_PLACEMENT_3D ( 'NONE', #27973, #20359, #3703 ) ;
#6529 = VERTEX_POINT ( 'NONE', #35864 ) ;
#6530 = CARTESIAN_POINT ( 'NONE',  ( -31.00354902519490352, 40.00000000000000000, -27.18544651223506392 ) ) ;
#6531 = FACE_OUTER_BOUND ( 'NONE', #18503, .T. ) ;
#6532 = AXIS2_PLACEMENT_3D ( 'NONE', #7801, #11101, #4295 ) ;
#6533 = DIRECTION ( 'NONE',  ( -1.000000000000000000, 0.000000000000000000, 0.000000000000000000 ) ) ;
#6534 = ORIENTED_EDGE ( 'NONE', *, *, #11617, .T. ) ;
#6535 = DIRECTION ( 'NONE',  ( -1.000000000000000000, -0.000000000000000000, -0.000000000000000000 ) ) ;
#6536 = CYLINDRICAL_SURFACE ( 'NONE', #34750, 13.60000000000000142 ) ;
#6537 = ORIENTED_EDGE ( 'NONE', *, *, #21725, .F. ) ;
#6538 = CYLINDRICAL_SURFACE ( 'NONE', #19404, 51.99999999999999289 ) ;
#6539 = VERTEX_POINT ( 'NONE', #25681 ) ;
#6540 = AXIS2_PLACEMENT_3D ( 'NONE', #40306, #23772, #34411 ) ;
#6541 = CIRCLE ( 'NONE', #5192, 13.60000000000000142 ) ;
#6542 = ORIENTED_EDGE ( 'NONE', *, *, #1784, .T. ) ;
#6543 = AXIS2_PLACEMENT_3D ( 'NONE', #10576, #23266, #23702 ) ;
#6544 = DIRECTION ( 'NONE',  ( -1.000000000000000000, -0.000000000000000000, -0.000000000000000000 ) ) ;
#6545 = EDGE_CURVE ( 'NONE', #14651, #8183, #33894, .T. ) ;
#6546 = CARTESIAN_POINT ( 'NONE',  ( 96.90013369365226481, 31.00000000000000000, -6.223598210838602540 ) ) ;
#6547 = ORIENTED_EDGE ( 'NONE', *, *, #5722, .T. ) ;
#6548 = FACE_OUTER_BOUND ( 'NONE', #13207, .T. ) ;
#6549 = EDGE_CURVE ( 'NONE', #1059, #4637, #19346, .T. ) ;
#6550 = EDGE_CURVE ( 'NONE', #43080, #34294, #39447, .T. ) ;
#6551 = ADVANCED_FACE ( 'NONE', ( #12140 ), #32616, .T. ) ;
#6552 = AXIS2_PLACEMENT_3D ( 'NONE', #20051, #13265, #17638 ) ;
#6553 = CYLINDRICAL_SURFACE ( 'NONE', #31014, 2.500000000000000444 ) ;
#6554 = CARTESIAN_POINT ( 'NONE',  ( 17.99999999999999645, -25.52601536738579213, -19.21447964122724272 ) ) ;
#6555 = ORIENTED_EDGE ( 'NONE', *, *, #4116, .T. ) ;
#6556 = FACE_OUTER_BOUND ( 'NONE', #18742, .T. ) ;
#6557 = AXIS2_PLACEMENT_3D ( 'NONE', #4501, #27891, #17874 ) ;
#6558 = DIRECTION ( 'NONE',  ( -1.000000000000000000, 0.000000000000000000, -0.000000000000000000 ) ) ;
#6560 = DIRECTION ( 'NONE',  ( -1.000000000000000000, 0.000000000000000000, 0.000000000000000000 ) ) ;
#6559 = FACE_OUTER_BOUND ( 'NONE', #5954, .T. ) ;
#6561 = CARTESIAN_POINT ( 'NONE',  ( -19.99999999999999645, 31.00000000000000355, 0.000000000000000000 ) ) ;
#6562 = LINE ( 'NONE', #13152, #36569 ) ;
#6563 = VERTEX_POINT ( 'NONE', #8846 ) ;
#6564 = CARTESIAN_POINT ( 'NONE',  ( -28.63582912838407069, 31.00000000000000355, 7.677129336082076705 ) ) ;
#6565 = AXIS2_PLACEMENT_3D ( 'NONE', #41685, #7873, #35131 ) ;
#6566 = ORIENTED_EDGE ( 'NONE', *, *, #9611, .F. ) ;
#6567 = CARTESIAN_POINT ( 'NONE',  ( 0.000000000000000000, -5.492704054967489924, 115.8698847939556202 ) ) ;
#6568 = DIRECTION ( 'NONE',  ( 0.000000000000000000, 0.4132121857683791477, -0.9106347728549126774 ) ) ;
#6569 = VERTEX_POINT ( 'NONE', #9058 ) ;
#6570 = CLOSED_SHELL ( 'NONE', ( #17527, #8939, #18650, #17169, #651, #20611, #7454, #13247, #24876, #33588, #15300, #4190, #39708, #2307, #26676, #21432, #7158, #30137, #41052, #14137, #32648, #36567, #26012, #28588, #4566, #10564, #20823, #29772, #6626, #20715, #11503, #985 ) ) ;
#6571 = CARTESIAN_POINT ( 'NONE',  ( -22.00000000000000000, 17.11489954122026447, 1.283214542831021765 ) ) ;
#6572 = CARTESIAN_POINT ( 'NONE',  ( -9.824444021593908616, 40.00000000000000000, 36.70529466175499778 ) ) ;
#6573 = CARTESIAN_POINT ( 'NONE',  ( 46.89968353242633015, 40.00000000000000000, -2.988513402017745069 ) ) ;
#6574 = AXIS2_PLACEMENT_3D ( 'NONE', #12867, #36389, #13095 ) ;
#6575 = ADVANCED_FACE ( 'NONE', ( #22204 ), #2697, .T. ) ;
#6576 = EDGE_LOOP ( 'NONE', ( #36896, #32679, #25136, #2161 ) ) ;
#6577 = AXIS2_PLACEMENT_3D ( 'NONE', #7725, #18042, #31079 ) ;
#6578 = VERTEX_POINT ( 'NONE', #39780 ) ;
#6579 = SURFACE_STYLE_USAGE ( .BOTH. , #13169 ) ;
#6580 = FACE_OUTER_BOUND ( 'NONE', #28729, .T. ) ;
#6581 = ADVANCED_FACE ( 'NONE', ( #23256 ), #26937, .F. ) ;
#6582 = DIRECTION ( 'NONE',  ( 0.000000000000000000, 1.881733940042638318E-15, -1.000000000000000000 ) ) ;
#6583 = CYLINDRICAL_SURFACE ( 'NONE', #41258, 19.99999999999999645 ) ;
#6584 = CARTESIAN_POINT ( 'NONE',  ( 17.99999999999999645, 118.8387007424473580, -19.94628303336373065 ) ) ;
#6585 = AXIS2_PLACEMENT_3D ( 'NONE', #26737, #43085, #30227 ) ;
#6586 = ORIENTED_EDGE ( 'NONE', *, *, #4325, .T. ) ;
#6587 = FACE_OUTER_BOUND ( 'NONE', #25710, .T. ) ;
#6588 = ORIENTED_EDGE ( 'NONE', *, *, #23595, .F. ) ;
#6589 = CARTESIAN_POINT ( 'NONE',  ( -9.000000000000005329, 1.543054966925665076E-15, 12.59999999999999964 ) ) ;
#6590 = DIRECTION ( 'NONE',  ( 0.000000000000000000, 0.1253332335643046747, -0.9921147013144777649 ) ) ;
#6591 = ORIENTED_EDGE ( 'NONE', *, *, #42266, .T. ) ;
#6592 = CARTESIAN_POINT ( 'NONE',  ( 6.200000000000001066, 19.19999999999999929, 0.000000000000000000 ) ) ;
#6593 = DIRECTION ( 'NONE',  ( -1.000000000000000000, -0.000000000000000000, 0.000000000000000000 ) ) ;
#6594 = VERTEX_POINT ( 'NONE', #718 ) ;
#6595 = CARTESIAN_POINT ( 'NONE',  ( 18.00000000000000355, -12.30077720129131791, 50.52416135122076923 ) ) ;
#6596 = ORIENTED_EDGE ( 'NONE', *, *, #42956, .T. ) ;
#6597 = CARTESIAN_POINT ( 'NONE',  ( 18.00000000000000355, 0.2227391519123156360, -46.98410307550729215 ) ) ;
#6598 = AXIS2_PLACEMENT_3D ( 'NONE', #14075, #13640, #27366 ) ;
#6599 = VERTEX_POINT ( 'NONE', #24116 ) ;
#6601 = ORIENTED_EDGE ( 'NONE', *, *, #1152, .T. ) ;
#6600 = LINE ( 'NONE', #3968, #32014 ) ;
#6602 = CARTESIAN_POINT ( 'NONE',  ( 15.22596115864829791, 31.00000000000000355, 57.21640888978779316 ) ) ;
#6603 = ORIENTED_EDGE ( 'NONE', *, *, #39520, .T. ) ;
#6604 = CARTESIAN_POINT ( 'NONE',  ( 0.000000000000000000, 0.000000000000000000, 0.000000000000000000 ) ) ;
#6605 = EDGE_CURVE ( 'NONE', #22812, #39801, #1845, .T. ) ;
#6606 = EDGE_CURVE ( 'NONE', #2710, #4270, #13019, .T. ) ;
#6607 = EDGE_CURVE ( 'NONE', #25436, #21133, #42939, .T. ) ;
#6608 = MECHANICAL_DESIGN_GEOMETRIC_PRESENTATION_REPRESENTATION (  '', ( #28942 ), #28266 ) ;
#6609 = CIRCLE ( 'NONE', #41461, 59.00000000000000711 ) ;
#6610 = ORIENTED_EDGE ( 'NONE', *, *, #2772, .F. ) ;
#6611 = CARTESIAN_POINT ( 'NONE',  ( 0.000000000000000000, -79.94368240339484544, 90.16373242487880191 ) ) ;
#6612 = EDGE_CURVE ( 'NONE', #42150, #19793, #20011, .T. ) ;
#6613 = ORIENTED_EDGE ( 'NONE', *, *, #27240, .T. ) ;
#6614 = CARTESIAN_POINT ( 'NONE',  ( 86.90011881125597881, 39.99999999999999289, -5.573058087428396590 ) ) ;
#6615 = AXIS2_PLACEMENT_3D ( 'NONE', #28375, #1930, #35519 ) ;
#6617 = DIRECTION ( 'NONE',  ( 0.000000000000000000, -1.000000000000000000, 5.297542245118643184E-16 ) ) ;
#6616 = CARTESIAN_POINT ( 'NONE',  ( 0.000000000000000000, 0.000000000000000000, 0.000000000000000000 ) ) ;
#6618 = CIRCLE ( 'NONE', #3827, 120.5010000000000190 ) ;
#6619 = ADVANCED_FACE ( 'NONE', ( #3993, #30428 ), #14077, .F. ) ;
#6620 = DIRECTION ( 'NONE',  ( -1.000000000000000000, 0.000000000000000000, 0.000000000000000000 ) ) ;
#6621 = VERTEX_POINT ( 'NONE', #17369 ) ;
#6622 = DIRECTION ( 'NONE',  ( 0.000000000000000000, 0.000000000000000000, 1.000000000000000000 ) ) ;
#6623 = ORIENTED_EDGE ( 'NONE', *, *, #18658, .T. ) ;
#6624 = B_SPLINE_CURVE_WITH_KNOTS ( 'NONE', 3,
 ( #18419, #41483, #11630, #8545, #5059, #5276, #18644, #2824 ),
 .UNSPECIFIED., .F., .F.,
 ( 4, 2, 2, 4 ),
 ( 0.000000000000000000, 0.002450665683189819262, 0.003675998524784728893, 0.004901331366379639391 ),
 .UNSPECIFIED. ) ;
#6625 = DIRECTION ( 'NONE',  ( -1.000000000000000000, -0.000000000000000000, -0.000000000000000000 ) ) ;
#6626 = ADVANCED_FACE ( 'NONE', ( #36508 ), #18509, .F. ) ;
#6627 = CARTESIAN_POINT ( 'NONE',  ( 24.81019160154284720, 31.00000000000000355, 73.04493173762017477 ) ) ;
#6629 = DIRECTION ( 'NONE',  ( -1.000000000000000000, 3.469446951953614189E-17, 0.000000000000000000 ) ) ;
#6628 = DIRECTION ( 'NONE',  ( -1.000000000000000000, -0.000000000000000000, -0.000000000000000000 ) ) ;
#6630 = ORIENTED_EDGE ( 'NONE', *, *, #5132, .F. ) ;
#6631 = CARTESIAN_POINT ( 'NONE',  ( 0.000000000000000000, -19.69434969228090893, 24.58291258574042004 ) ) ;
#6632 = CIRCLE ( 'NONE', #3809, 31.49899999999999523 ) ;
#6633 = ORIENTED_EDGE ( 'NONE', *, *, #3820, .F. ) ;
#6634 = CARTESIAN_POINT ( 'NONE',  ( 17.99999999999999645, -6.486220790509180212, 112.0098273076987283 ) ) ;
#6635 = CARTESIAN_POINT ( 'NONE',  ( 18.00000000000000355, -19.74581912682808493, -48.10512059033413124 ) ) ;
#6637 = DIRECTION ( 'NONE',  ( -1.000000000000000000, -0.000000000000000000, 0.000000000000000000 ) ) ;
#6636 = CIRCLE ( 'NONE', #13649, 120.5010000000000332 ) ;
#6638 = CIRCLE ( 'NONE', #12249, 158.4999999999992042 ) ;
#6639 = DIRECTION ( 'NONE',  ( -1.000000000000000000, 0.000000000000000000, 0.000000000000000000 ) ) ;
#6640 = EDGE_CURVE ( 'NONE', #1957, #35650, #24184, .T. ) ;
#6641 = AXIS2_PLACEMENT_3D ( 'NONE', #20346, #3040, #16410 ) ;
#6642 = AXIS2_PLACEMENT_3D ( 'NONE', #19613, #2546, #9114 ) ;
#6643 = CARTESIAN_POINT ( 'NONE',  ( 17.99999999999999645, 0.000000000000000000, 0.000000000000000000 ) ) ;
#6644 = ORIENTED_EDGE ( 'NONE', *, *, #38571, .F. ) ;
#6645 = FACE_OUTER_BOUND ( 'NONE', #14197, .T. ) ;
#6646 = ORIENTED_EDGE ( 'NONE', *, *, #17278, .T. ) ;
#6647 = DIRECTION ( 'NONE',  ( -0.06345332152672161774, 1.058048417131579272E-15, 0.9979848074931934043 ) ) ;
#6648 = AXIS2_PLACEMENT_3D ( 'NONE', #31567, #14581, #14795 ) ;
#6649 = AXIS2_PLACEMENT_3D ( 'NONE', #402, #21189, #17924 ) ;
#6650 = DIRECTION ( 'NONE',  ( 1.000000000000000000, 0.000000000000000000, -6.546126324440850663E-16 ) ) ;
#6651 = CARTESIAN_POINT ( 'NONE',  ( 17.99999999999999645, 0.000000000000000000, 0.000000000000000000 ) ) ;
#6652 = EDGE_LOOP ( 'NONE', ( #39273, #13375, #31887, #38445 ) ) ;
#6653 = ORIENTED_EDGE ( 'NONE', *, *, #11316, .F. ) ;
#6654 = CARTESIAN_POINT ( 'NONE',  ( 0.000000000000000000, 0.000000000000000000, -20.00000000000000000 ) ) ;
#6655 = DIRECTION ( 'NONE',  ( 0.000000000000000000, -0.4132121857683850874, 0.9106347728549100129 ) ) ;
#6656 = AXIS2_PLACEMENT_3D ( 'NONE', #24085, #30618, #37573 ) ;
#6657 = FACE_OUTER_BOUND ( 'NONE', #33150, .T. ) ;
#6659 = ORIENTED_EDGE ( 'NONE', *, *, #27078, .T. ) ;
#6658 = CARTESIAN_POINT ( 'NONE',  ( 0.000000000000000000, 119.8996782608629985, 12.02323392193396856 ) ) ;
#6660 = CARTESIAN_POINT ( 'NONE',  ( -2.197745971918068530, 31.00000000000000355, -34.39891587002171036 ) ) ;
#6661 = DIRECTION ( 'NONE',  ( -1.000000000000000000, -0.000000000000000000, -0.000000000000000000 ) ) ;
#6662 = EDGE_CURVE ( 'NONE', #6179, #31565, #31829, .T. ) ;
#6664 = ORIENTED_EDGE ( 'NONE', *, *, #26349, .F. ) ;
#6663 = CARTESIAN_POINT ( 'NONE',  ( 0.000000000000000000, 0.000000000000000000, 0.000000000000000000 ) ) ;
#6665 = ORIENTED_EDGE ( 'NONE', *, *, #11380, .T. ) ;
#6666 = DIRECTION ( 'NONE',  ( 1.000000000000000000, 0.000000000000000000, 0.000000000000000000 ) ) ;
#6667 = FACE_OUTER_BOUND ( 'NONE', #34063, .T. ) ;
#6668 = CARTESIAN_POINT ( 'NONE',  ( 48.78760054484346398, 40.00000000000000000, -28.06521077754944926 ) ) ;
#6669 = LINE ( 'NONE', #40029, #30645 ) ;
#6670 = CIRCLE ( 'NONE', #5951, 51.99999999999999289 ) ;
#6671 = DIRECTION ( 'NONE',  ( -1.000000000000000000, 0.000000000000000000, 0.000000000000000000 ) ) ;
#6672 = AXIS2_PLACEMENT_3D ( 'NONE', #12469, #32290, #2375 ) ;
#6673 = DIRECTION ( 'NONE',  ( 0.000000000000000000, -0.8183027759081622499, -0.5747874102144165942 ) ) ;
#6675 = ORIENTED_EDGE ( 'NONE', *, *, #7822, .T. ) ;
#6674 = VECTOR ( 'NONE', #30099, 1000.000000000000114 ) ;
#6676 = DIRECTION ( 'NONE',  ( -0.000000000000000000, -0.000000000000000000, 1.000000000000000000 ) ) ;
#6677 = EDGE_CURVE ( 'NONE', #8548, #11411, #12339, .T. ) ;
#6678 = CIRCLE ( 'NONE', #4588, 20.00000000000001066 ) ;
#6679 = ORIENTED_EDGE ( 'NONE', *, *, #36590, .F. ) ;
#6680 = CIRCLE ( 'NONE', #2488, 52.00000000000000000 ) ;
#6681 = CARTESIAN_POINT ( 'NONE',  ( 18.00000000000000355, -46.87740477351720614, 3.172455868805039270 ) ) ;
#6682 = CARTESIAN_POINT ( 'NONE',  ( 18.00000000000000355, 0.000000000000000000, 0.000000000000000000 ) ) ;
#6683 = EDGE_CURVE ( 'NONE', #12272, #25229, #4644, .T. ) ;
#6684 = AXIS2_PLACEMENT_3D ( 'NONE', #9054, #12564, #33258 ) ;
#6685 = CARTESIAN_POINT ( 'NONE',  ( -29.60425243605831724, 31.00000000000000355, 38.59963703562669934 ) ) ;
#6686 = CYLINDRICAL_SURFACE ( 'NONE', #21183, 51.99999999999999289 ) ;
#6688 = EDGE_LOOP ( 'NONE', ( #27743, #22177, #33528, #21853 ) ) ;
#6687 = AXIS2_PLACEMENT_3D ( 'NONE', #38154, #38788, #31611 ) ;
#6689 = AXIS2_PLACEMENT_3D ( 'NONE', #38602, #31441, #34914 ) ;
#6691 = VECTOR ( 'NONE', #11754, 1000.000000000000000 ) ;
#6690 = DIRECTION ( 'NONE',  ( 0.000000000000000000, 0.000000000000000000, 1.000000000000000000 ) ) ;
#6692 = ORIENTED_EDGE ( 'NONE', *, *, #15852, .F. ) ;
#6693 = CARTESIAN_POINT ( 'NONE',  ( -18.08361268445098347, 40.00000000000000000, -10.43497034982449456 ) ) ;
#6694 = VERTEX_POINT ( 'NONE', #7061 ) ;
#6695 = DIRECTION ( 'NONE',  ( -1.000000000000000000, -0.000000000000000000, 0.000000000000000000 ) ) ;
#6696 = ORIENTED_EDGE ( 'NONE', *, *, #33011, .F. ) ;
#6697 = CARTESIAN_POINT ( 'NONE',  ( 66.75914267695947046, 31.00000000000000000, 8.899205196610871837 ) ) ;
#6698 = CARTESIAN_POINT ( 'NONE',  ( 40.05902963217418744, 40.00000000000000000, -52.04757428485088866 ) ) ;
#6699 = DIRECTION ( 'NONE',  ( 1.000000000000000000, 0.000000000000000000, 0.000000000000000000 ) ) ;
#6700 = ORIENTED_EDGE ( 'NONE', *, *, #31609, .T. ) ;
#6701 = EDGE_LOOP ( 'NONE', ( #37988, #10263, #35275, #11956 ) ) ;
#6702 = CARTESIAN_POINT ( 'NONE',  ( 17.99999999999999645, -40.37724737309996215, -104.6802291180871265 ) ) ;
#6703 = DIRECTION ( 'NONE',  ( 0.000000000000000000, 0.000000000000000000, -1.000000000000000000 ) ) ;
#6704 = DIRECTION ( 'NONE',  ( -1.000000000000000000, 0.000000000000000000, -0.000000000000000000 ) ) ;
#6705 = CIRCLE ( 'NONE', #19297, 116.0000000000000000 ) ;
#6707 = ORIENTED_EDGE ( 'NONE', *, *, #40336, .T. ) ;
#6706 = CARTESIAN_POINT ( 'NONE',  ( 17.99999999999999645, -27.24480646643597126, -15.80846360676612861 ) ) ;
#6708 = VECTOR ( 'NONE', #17021, 1000.000000000000000 ) ;
#6709 = DIRECTION ( 'NONE',  ( 0.000000000000000000, 0.000000000000000000, 1.000000000000000000 ) ) ;
#6710 = ORIENTED_EDGE ( 'NONE', *, *, #4869, .T. ) ;
#6711 = CARTESIAN_POINT ( 'NONE',  ( 17.99999999999999645, -40.13512380273891011, -113.6206972269525863 ) ) ;
#6712 = CIRCLE ( 'NONE', #19996, 10.99999999999998934 ) ;
#6713 = CARTESIAN_POINT ( 'NONE',  ( 50.95389515256417923, 40.00000000000000000, -66.42840393140320998 ) ) ;
#6714 = CARTESIAN_POINT ( 'NONE',  ( -75.96080130434582145, -12.05525454449571043, 14.45886780445738218 ) ) ;
#6715 = ORIENTED_EDGE ( 'NONE', *, *, #39039, .F. ) ;
#6716 = DIRECTION ( 'NONE',  ( -1.000000000000000000, 0.000000000000000000, 0.000000000000000000 ) ) ;
#6717 = LINE ( 'NONE', #27033, #29458 ) ;
#6718 = EDGE_CURVE ( 'NONE', #29708, #26637, #20634, .T. ) ;
#6719 = EDGE_LOOP ( 'NONE', ( #7514, #4905, #19906, #5870 ) ) ;
#6720 = ADVANCED_FACE ( 'NONE', ( #27590 ), #15166, .F. ) ;
#6721 = AXIS2_PLACEMENT_3D ( 'NONE', #39446, #9352, #9581 ) ;
#6722 = ORIENTED_EDGE ( 'NONE', *, *, #4307, .F. ) ;
#6723 = DIRECTION ( 'NONE',  ( 0.000000000000000000, 0.000000000000000000, 1.000000000000000000 ) ) ;
#6724 = ORIENTED_EDGE ( 'NONE', *, *, #19734, .T. ) ;
#6725 = CARTESIAN_POINT ( 'NONE',  ( 23.62253089228586944, 40.00000000000000000, -11.62353008834529255 ) ) ;
#6726 = CARTESIAN_POINT ( 'NONE',  ( 8.919999999999999929, 0.000000000000000000, 0.000000000000000000 ) ) ;
#6727 = DIRECTION ( 'NONE',  ( 3.009274222672345096E-17, 1.000000000000000000, -2.455023325076454960E-18 ) ) ;
#6728 = AXIS2_PLACEMENT_3D ( 'NONE', #19132, #2905, #5990 ) ;
#6729 = CARTESIAN_POINT ( 'NONE',  ( 17.99999999999999645, 7.220349212960956997, -35.26849241522656797 ) ) ;
#6730 = CARTESIAN_POINT ( 'NONE',  ( 0.000000000000000000, -95.38615066514023511, 59.07414607872794932 ) ) ;
#6731 = ORIENTED_EDGE ( 'NONE', *, *, #13712, .F. ) ;
#6732 = CARTESIAN_POINT ( 'NONE',  ( 0.000000000000000000, 19.47322409167312429, -30.27859877001379374 ) ) ;
#6733 = EDGE_CURVE ( 'NONE', #36312, #41379, #31138, .T. ) ;
#6734 = ORIENTED_EDGE ( 'NONE', *, *, #27091, .F. ) ;
#6735 = FILL_AREA_STYLE_COLOUR ( '', #193 ) ;
#6736 = CARTESIAN_POINT ( 'NONE',  ( 17.99999999999999645, -3.803237743091689715, -31.26855263151018960 ) ) ;
#6737 = ADVANCED_FACE ( 'NONE', ( #11880 ), #17795, .T. ) ;
#6738 = DIRECTION ( 'NONE',  ( -1.000000000000000000, -0.000000000000000000, -0.000000000000000000 ) ) ;
#6740 = VERTEX_POINT ( 'NONE', #31713 ) ;
#6739 = VECTOR ( 'NONE', #38318, 1000.000000000000000 ) ;
#6741 = DIRECTION ( 'NONE',  ( 1.000000000000000000, 0.000000000000000000, 0.000000000000000000 ) ) ;
#6742 = CARTESIAN_POINT ( 'NONE',  ( 0.000000000000000000, -0.5156212287272186057, -112.1962860721878172 ) ) ;
#6743 = CIRCLE ( 'NONE', #30462, 158.5000000000000284 ) ;
#6744 = DIRECTION ( 'NONE',  ( 1.000000000000000000, 0.000000000000000000, 0.000000000000000000 ) ) ;
#6745 = CARTESIAN_POINT ( 'NONE',  ( 66.75446398494719347, 31.00000000000000000, -32.91950810868348043 ) ) ;
#6746 = AXIS2_PLACEMENT_3D ( 'NONE', #9607, #22959, #36200 ) ;
#6747 = VERTEX_POINT ( 'NONE', #41292 ) ;
#6749 = CARTESIAN_POINT ( 'NONE',  ( 27.04960320298028620, 31.00000000000000355, -23.64836272119223892 ) ) ;
#6748 = AXIS2_PLACEMENT_3D ( 'NONE', #8811, #8175, #38471 ) ;
#6750 = CARTESIAN_POINT ( 'NONE',  ( -56.48955861152074220, 40.00000000000000711, -43.32902275383659685 ) ) ;
#6751 = AXIS2_PLACEMENT_3D ( 'NONE', #19016, #41435, #8504 ) ;
#6752 = EDGE_CURVE ( 'NONE', #34203, #42167, #30854, .T. ) ;
#6753 = CYLINDRICAL_SURFACE ( 'NONE', #9465, 59.00000000000000711 ) ;
#6754 = AXIS2_PLACEMENT_3D ( 'NONE', #30845, #34106, #33251 ) ;
#6755 = CARTESIAN_POINT ( 'NONE',  ( 17.99999999999999645, 110.1579703617966430, 21.29539948940285043 ) ) ;
#6756 = EDGE_CURVE ( 'NONE', #37390, #39824, #11415, .T. ) ;
#6757 = ORIENTED_EDGE ( 'NONE', *, *, #20205, .F. ) ;
#6758 = CARTESIAN_POINT ( 'NONE',  ( 9.000000000000001776, -37.07968990261553444, 109.9140418541956308 ) ) ;
#6759 = DIRECTION ( 'NONE',  ( 0.000000000000000000, 0.000000000000000000, 1.000000000000000000 ) ) ;
#6760 = PRODUCT_DEFINITION_SHAPE ( 'NONE', 'NONE',  #8157 ) ;
#6761 = ORIENTED_EDGE ( 'NONE', *, *, #36375, .T. ) ;
#6762 = CARTESIAN_POINT ( 'NONE',  ( -46.87443272357899815, 40.00000000000000000, 35.96965017775951878 ) ) ;
#6763 = DIRECTION ( 'NONE',  ( 0.000000000000000000, -1.000000000000000000, 0.000000000000000000 ) ) ;
#6764 = DIRECTION ( 'NONE',  ( 1.000000000000000000, 0.000000000000000000, 0.000000000000000000 ) ) ;
#6765 = ORIENTED_EDGE ( 'NONE', *, *, #4670, .T. ) ;
#6766 = AXIS2_PLACEMENT_3D ( 'NONE', #21096, #4677, #24362 ) ;
#6767 = DIRECTION ( 'NONE',  ( 0.000000000000000000, -1.000000000000000000, 5.297542245118643184E-16 ) ) ;
#6768 = CARTESIAN_POINT ( 'NONE',  ( 0.000000000000000000, 0.000000000000000000, 0.000000000000000000 ) ) ;
#6769 = EDGE_LOOP ( 'NONE', ( #17557, #40124, #36540, #28473 ) ) ;
#6770 = DIRECTION ( 'NONE',  ( 0.000000000000000000, 0.000000000000000000, 1.000000000000000000 ) ) ;
#6771 = ORIENTED_EDGE ( 'NONE', *, *, #3696, .F. ) ;
#6772 = VECTOR ( 'NONE', #8323, 1000.000000000000000 ) ;
#6773 = VECTOR ( 'NONE', #2395, 1000.000000000000000 ) ;
#6774 = VERTEX_POINT ( 'NONE', #8154 ) ;
#6775 = CIRCLE ( 'NONE', #37422, 58.99999999999999289 ) ;
#6776 = CYLINDRICAL_SURFACE ( 'NONE', #31359, 59.00000000000000000 ) ;
#6777 = AXIS2_PLACEMENT_3D ( 'NONE', #12751, #29978, #2877 ) ;
#6778 = CARTESIAN_POINT ( 'NONE',  ( -24.28006566512905451, 31.00000000000000355, -91.10131089348453770 ) ) ;
#6779 = ORIENTED_EDGE ( 'NONE', *, *, #39520, .F. ) ;
#6780 = DIRECTION ( 'NONE',  ( 1.000000000000000000, -0.000000000000000000, -0.000000000000000000 ) ) ;
#6781 = CARTESIAN_POINT ( 'NONE',  ( 17.99999999999999645, 29.36437154451999021, 116.8684075565137164 ) ) ;
#6782 = AXIS2_PLACEMENT_3D ( 'NONE', #39725, #20363, #6568 ) ;
#6783 = LINE ( 'NONE', #30148, #20646 ) ;
#6784 = VERTEX_POINT ( 'NONE', #34543 ) ;
#6785 = DIRECTION ( 'NONE',  ( 0.000000000000000000, 0.000000000000000000, 1.000000000000000000 ) ) ;
#6786 = ADVANCED_FACE ( 'NONE', ( #4653 ), #34769, .T. ) ;
#6787 = PLANE ( 'NONE',  #10176 ) ;
#6788 = EDGE_CURVE ( 'NONE', #4027, #12125, #24672, .T. ) ;
#6790 = CARTESIAN_POINT ( 'NONE',  ( 18.00000000000000355, -46.77034588191287412, -22.72740077717278595 ) ) ;
#6789 = CARTESIAN_POINT ( 'NONE',  ( -10.00000000000000000, 0.000000000000000000, 0.000000000000000000 ) ) ;
#6791 = DIRECTION ( 'NONE',  ( -1.000000000000000000, 0.000000000000000000, 0.000000000000000000 ) ) ;
#6792 = VERTEX_POINT ( 'NONE', #21727 ) ;
#6793 = CARTESIAN_POINT ( 'NONE',  ( 8.528031178950213231, 31.00000000000000355, -31.86521141804621493 ) ) ;
#6794 = ORIENTED_EDGE ( 'NONE', *, *, #31413, .F. ) ;
#6795 = DIRECTION ( 'NONE',  ( -1.000000000000000000, 0.000000000000000000, -0.000000000000000000 ) ) ;
#6796 = FACE_OUTER_BOUND ( 'NONE', #37297, .T. ) ;
#6797 = AXIS2_PLACEMENT_3D ( 'NONE', #12535, #29119, #42392 ) ;
#6798 = ORIENTED_EDGE ( 'NONE', *, *, #40797, .F. ) ;
#6799 = DIRECTION ( 'NONE',  ( 0.000000000000000000, 0.000000000000000000, -1.000000000000000000 ) ) ;
#6800 = CARTESIAN_POINT ( 'NONE',  ( -18.51709390187839688, 40.00000000000000000, -37.54239277154294996 ) ) ;
#6801 = CIRCLE ( 'NONE', #31216, 4.250000000000000000 ) ;
#6802 = CARTESIAN_POINT ( 'NONE',  ( -41.03896728212566103, 40.00000000000000000, -11.06873348903577892 ) ) ;
#6803 = CIRCLE ( 'NONE', #43011, 20.00000000000000711 ) ;
#6804 = AXIS2_PLACEMENT_3D ( 'NONE', #42768, #40151, #10287 ) ;
#6805 = CIRCLE ( 'NONE', #33290, 120.5010000000000190 ) ;
#6806 = VERTEX_POINT ( 'NONE', #11439 ) ;
#6807 = VERTEX_POINT ( 'NONE', #28247 ) ;
#6808 = DIRECTION ( 'NONE',  ( 0.000000000000000000, 0.000000000000000000, 1.000000000000000000 ) ) ;
#6809 = DIRECTION ( 'NONE',  ( 1.000000000000000000, 0.000000000000000000, 0.000000000000000000 ) ) ;
#6810 = EDGE_CURVE ( 'NONE', #27138, #5471, #19804, .T. ) ;
#6811 = AXIS2_PLACEMENT_3D ( 'NONE', #36916, #36471, #6590 ) ;
#6812 = EDGE_CURVE ( 'NONE', #17691, #41039, #4879, .T. ) ;
#6813 = LINE ( 'NONE', #15802, #29424 ) ;
#6814 = EDGE_LOOP ( 'NONE', ( #37903, #18960, #22455, #2363 ) ) ;
#6815 = DIRECTION ( 'NONE',  ( -1.000000000000000000, 0.000000000000000000, 0.000000000000000000 ) ) ;
#6816 = VERTEX_POINT ( 'NONE', #11016 ) ;
#6817 = FACE_OUTER_BOUND ( 'NONE', #22890, .T. ) ;
#6818 = DIRECTION ( 'NONE',  ( 0.000000000000000000, 0.000000000000000000, 1.000000000000000000 ) ) ;
#6819 = AXIS2_PLACEMENT_3D ( 'NONE', #27199, #16965, #24156 ) ;
#6820 = ORIENTED_EDGE ( 'NONE', *, *, #30353, .T. ) ;
#6821 = CYLINDRICAL_SURFACE ( 'NONE', #29813, 59.00000000000000000 ) ;
#6822 = CARTESIAN_POINT ( 'NONE',  ( 5.639656061357294803, -10.48075544252183100, 0.000000000000000000 ) ) ;
#6823 = ORIENTED_EDGE ( 'NONE', *, *, #34847, .F. ) ;
#6824 = DIRECTION ( 'NONE',  ( 1.000000000000000000, 0.000000000000000000, 0.000000000000000000 ) ) ;
#6825 = ORIENTED_EDGE ( 'NONE', *, *, #8743, .T. ) ;
#6826 = CYLINDRICAL_SURFACE ( 'NONE', #23976, 2.649999999999979039 ) ;
#6827 = ORIENTED_EDGE ( 'NONE', *, *, #31058, .F. ) ;
#6829 = ORIENTED_EDGE ( 'NONE', *, *, #12813, .T. ) ;
#6828 = CARTESIAN_POINT ( 'NONE',  ( 17.99999999999999645, -87.92975456462950490, 69.68953103478128241 ) ) ;
#6830 = CARTESIAN_POINT ( 'NONE',  ( -19.43072497042362556, 31.00000000000000355, 56.92208038676059800 ) ) ;
#6831 = ORIENTED_EDGE ( 'NONE', *, *, #11091, .F. ) ;
#6832 = DIRECTION ( 'NONE',  ( -1.000000000000000000, 0.000000000000000000, 0.000000000000000000 ) ) ;
#6833 = CIRCLE ( 'NONE', #13121, 59.00000000000000000 ) ;
#6834 = VECTOR ( 'NONE', #37612, 1000.000000000000000 ) ;
#6835 = EDGE_LOOP ( 'NONE', ( #35609, #3619, #39600, #15456 ) ) ;
#6836 = LINE ( 'NONE', #20194, #28722 ) ;
#6837 = EDGE_CURVE ( 'NONE', #3479, #25483, #40643, .T. ) ;
#6838 = ORIENTED_EDGE ( 'NONE', *, *, #18158, .T. ) ;
#6839 = VECTOR ( 'NONE', #34761, 1000.000000000000000 ) ;
#6840 = CARTESIAN_POINT ( 'NONE',  ( 20.39742982868580157, 40.00000000000000000, 76.57971376067894198 ) ) ;
#6841 = CIRCLE ( 'NONE', #18057, 47.49899999999999523 ) ;
#6842 = EDGE_CURVE ( 'NONE', #12550, #22817, #6518, .T. ) ;
#6843 = AXIS2_PLACEMENT_3D ( 'NONE', #9619, #5692, #19678 ) ;
#6845 = CARTESIAN_POINT ( 'NONE',  ( 0.000000000000000000, 0.000000000000000000, 0.000000000000000000 ) ) ;
#6844 = CARTESIAN_POINT ( 'NONE',  ( 18.00000000000000355, 9.744342220504043084, -46.48873837489787064 ) ) ;
#6846 = DIRECTION ( 'NONE',  ( -1.000000000000000000, -0.000000000000000000, 0.000000000000000000 ) ) ;
#6847 = ORIENTED_EDGE ( 'NONE', *, *, #15871, .T. ) ;
#6848 = DIRECTION ( 'NONE',  ( 0.000000000000000000, 0.000000000000000000, 1.000000000000000000 ) ) ;
#6849 = VERTEX_POINT ( 'NONE', #5084 ) ;
#6850 = FACE_OUTER_BOUND ( 'NONE', #25759, .T. ) ;
#6851 = CARTESIAN_POINT ( 'NONE',  ( -75.41724699911947027, 31.00000000000000711, 25.61573074746135248 ) ) ;
#6853 = DIRECTION ( 'NONE',  ( -1.000000000000000000, 0.000000000000000000, 0.000000000000000000 ) ) ;
#6852 = DIRECTION ( 'NONE',  ( -1.000000000000000000, 0.000000000000000000, 0.000000000000000000 ) ) ;
#6854 = VERTEX_POINT ( 'NONE', #24345 ) ;
#6855 = DIRECTION ( 'NONE',  ( 0.000000000000000000, 0.5963673585385027565, -0.8027116379309627847 ) ) ;
#6856 = EDGE_CURVE ( 'NONE', #35938, #12319, #35751, .T. ) ;
#6857 = ORIENTED_EDGE ( 'NONE', *, *, #31360, .F. ) ;
#6858 = CARTESIAN_POINT ( 'NONE',  ( 0.000000000000000000, -6.486220790507708500, -112.0098273076987994 ) ) ;
#6859 = CARTESIAN_POINT ( 'NONE',  ( 0.000000000000000000, 0.000000000000000000, -5.000000000000000000 ) ) ;
#6860 = EDGE_CURVE ( 'NONE', #40285, #19624, #23981, .T. ) ;
#6861 = CARTESIAN_POINT ( 'NONE',  ( 18.00000000000000355, 51.19683565102456413, -9.104066087302928878 ) ) ;
#6862 = AXIS2_PLACEMENT_3D ( 'NONE', #35101, #29225, #38580 ) ;
#6863 = EDGE_CURVE ( 'NONE', #9503, #35353, #26724, .T. ) ;
#6864 = ADVANCED_FACE ( 'NONE', ( #37809 ), #38452, .F. ) ;
#6865 = CARTESIAN_POINT ( 'NONE',  ( 17.99999999999999645, 29.09613215194482905, 21.19941258140334028 ) ) ;
#6866 = AXIS2_PLACEMENT_3D ( 'NONE', #11456, #27607, #1392 ) ;
#6867 = EDGE_LOOP ( 'NONE', ( #32271, #29422, #773, #36267 ) ) ;
#6868 = DIRECTION ( 'NONE',  ( 0.000000000000000000, -0.2113826236296315053, 0.9774033898178651203 ) ) ;
#6869 = VERTEX_POINT ( 'NONE', #17581 ) ;
#6870 = CARTESIAN_POINT ( 'NONE',  ( 0.000000000000000000, 0.000000000000000000, 0.000000000000000000 ) ) ;
#6871 = CARTESIAN_POINT ( 'NONE',  ( 0.000000000000000000, 31.08872492059957793, 41.68322423723110148 ) ) ;
#6872 = CARTESIAN_POINT ( 'NONE',  ( 9.000000000000001776, 110.8621702203453339, -34.14058016547421914 ) ) ;
#6873 = ORIENTED_EDGE ( 'NONE', *, *, #37104, .T. ) ;
#6874 = ORIENTED_EDGE ( 'NONE', *, *, #2413, .T. ) ;
#6875 = CYLINDRICAL_SURFACE ( 'NONE', #5650, 129.9999999999993463 ) ;
#6876 = DIRECTION ( 'NONE',  ( 1.000000000000000000, 1.836909530733573776E-16, 0.000000000000000000 ) ) ;
#6877 = DIRECTION ( 'NONE',  ( -1.000000000000000000, 0.000000000000000000, 0.000000000000000000 ) ) ;
#6879 = EDGE_LOOP ( 'NONE', ( #21079, #30222, #25018, #21706 ) ) ;
#6878 = DIRECTION ( 'NONE',  ( -1.000000000000000000, -0.000000000000000000, 0.000000000000000000 ) ) ;
#6880 = CARTESIAN_POINT ( 'NONE',  ( 35.42814233785335176, 31.00000000000000355, -9.427541829740359702 ) ) ;
#6881 = DIRECTION ( 'NONE',  ( 1.000000000000000000, 0.000000000000000000, 0.000000000000000000 ) ) ;
#6883 = EDGE_LOOP ( 'NONE', ( #26429, #32343, #3196, #18251 ) ) ;
#6882 = CARTESIAN_POINT ( 'NONE',  ( 17.99999999999999645, 112.5220807139884016, 28.19186676675879255 ) ) ;
#6884 = ORIENTED_EDGE ( 'NONE', *, *, #12070, .T. ) ;
#6885 = DIRECTION ( 'NONE',  ( -3.009274222672345096E-17, -1.000000000000000000, 2.455023325076454960E-18 ) ) ;
#6886 = DIRECTION ( 'NONE',  ( -1.000000000000000000, 0.000000000000000000, 0.000000000000000000 ) ) ;
#6887 = CARTESIAN_POINT ( 'NONE',  ( -42.11670055800494339, 40.00000000000000000, -32.42481051986320040 ) ) ;
#6888 = ADVANCED_FACE ( 'NONE', ( #22356 ), #29510, .F. ) ;
#6889 = DIRECTION ( 'NONE',  ( -1.000000000000000000, 0.000000000000000000, 0.000000000000000000 ) ) ;
#6890 = LINE ( 'NONE', #33304, #42919 ) ;
#6891 = ORIENTED_EDGE ( 'NONE', *, *, #6606, .F. ) ;
#6892 = AXIS2_PLACEMENT_3D ( 'NONE', #8756, #41907, #32307 ) ;
#6893 = DIRECTION ( 'NONE',  ( 0.000000000000000000, -0.7865515558026479059, 0.6175246149461850464 ) ) ;
#6894 = ORIENTED_EDGE ( 'NONE', *, *, #25287, .T. ) ;
#6895 = CYLINDRICAL_SURFACE ( 'NONE', #32941, 20.00000000000000355 ) ;
#6896 = CARTESIAN_POINT ( 'NONE',  ( 9.000000000000001776, -29.86146780999875716, -112.0905559814581665 ) ) ;
#6897 = CARTESIAN_POINT ( 'NONE',  ( -49.88601606984090608, 31.00000000000000355, -6.565487524765669214 ) ) ;
#6898 = CARTESIAN_POINT ( 'NONE',  ( 17.99999999999999645, 0.000000000000000000, 0.000000000000000000 ) ) ;
#6899 = VERTEX_POINT ( 'NONE', #25622 ) ;
#6900 = DIRECTION ( 'NONE',  ( 0.000000000000000000, -0.4817536741017036661, -0.8763066800438700232 ) ) ;
#6901 = ORIENTED_EDGE ( 'NONE', *, *, #15925, .T. ) ;
#6902 = CARTESIAN_POINT ( 'NONE',  ( -15.93581279029885422, 40.00000000000000000, -13.96891150189262021 ) ) ;
#6903 = ORIENTED_EDGE ( 'NONE', *, *, #36381, .F. ) ;
#6904 = FACE_OUTER_BOUND ( 'NONE', #41201, .T. ) ;
#6905 = CARTESIAN_POINT ( 'NONE',  ( 10.26812810425290579, 31.00000000000000355, 78.79123036457541218 ) ) ;
#6906 = CARTESIAN_POINT ( 'NONE',  ( -73.09555549758189841, 40.00000000000000711, 35.91380138263622257 ) ) ;
#6907 = EDGE_CURVE ( 'NONE', #42608, #27860, #26025, .T. ) ;
#6908 = EDGE_CURVE ( 'NONE', #10741, #15182, #10710, .T. ) ;
#6909 = CARTESIAN_POINT ( 'NONE',  ( 0.000000000000000000, 0.000000000000000000, 0.000000000000000000 ) ) ;
#6910 = ADVANCED_FACE ( 'NONE', ( #9212 ), #18676, .F. ) ;
#6911 = EDGE_LOOP ( 'NONE', ( #42117, #8591, #19085, #19729 ) ) ;
#6912 = ORIENTED_EDGE ( 'NONE', *, *, #33271, .T. ) ;
#6913 = DIRECTION ( 'NONE',  ( 1.000000000000000000, -0.000000000000000000, -0.000000000000000000 ) ) ;
#6914 = LINE ( 'NONE', #34131, #17381 ) ;
#6915 = DIRECTION ( 'NONE',  ( -1.000000000000000000, 0.000000000000000000, 0.000000000000000000 ) ) ;
#6916 = AXIS2_PLACEMENT_3D ( 'NONE', #41269, #28444, #21493 ) ;
#6917 = AXIS2_PLACEMENT_3D ( 'NONE', #33703, #7298, #3786 ) ;
#6919 = VERTEX_POINT ( 'NONE', #35604 ) ;
#6918 = DIRECTION ( 'NONE',  ( -1.000000000000000000, -0.000000000000000000, 0.000000000000000000 ) ) ;
#6920 = CARTESIAN_POINT ( 'NONE',  ( 17.99999999999999645, 31.81777574834305966, -2.898764365605425830 ) ) ;
#6921 = VERTEX_POINT ( 'NONE', #15378 ) ;
#6922 = CARTESIAN_POINT ( 'NONE',  ( 4.121423858225410797, -12.61643262889541006, 0.000000000000000000 ) ) ;
#6923 = AXIS2_PLACEMENT_3D ( 'NONE', #13339, #3468, #13129 ) ;
#6924 = EDGE_CURVE ( 'NONE', #36681, #42716, #8619, .T. ) ;
#6925 = CARTESIAN_POINT ( 'NONE',  ( 38.45889818826288575, 40.00000000000000000, 77.98987599019784511 ) ) ;
#6926 = CARTESIAN_POINT ( 'NONE',  ( -150.4999999999986926, -2.921102061156358310E-13, 10.00000000000004441 ) ) ;
#6927 = VERTEX_POINT ( 'NONE', #19501 ) ;
#6928 = EDGE_CURVE ( 'NONE', #21082, #26674, #32291, .T. ) ;
#6929 = CARTESIAN_POINT ( 'NONE',  ( 17.99999999999999645, -5.822172717930031993, -31.41458249383147106 ) ) ;
#6930 = CARTESIAN_POINT ( 'NONE',  ( 18.00000000000000355, -46.21320724403656044, 10.97699764141937173 ) ) ;
#6931 = ORIENTED_EDGE ( 'NONE', *, *, #22927, .T. ) ;
#6932 = CARTESIAN_POINT ( 'NONE',  ( 0.000000000000000000, 0.000000000000000000, 0.000000000000000000 ) ) ;
#6933 = ORIENTED_EDGE ( 'NONE', *, *, #30191, .F. ) ;
#6934 = CARTESIAN_POINT ( 'NONE',  ( 17.99999999999999645, -31.81777574834303124, -2.898764365605651427 ) ) ;
#6935 = ORIENTED_EDGE ( 'NONE', *, *, #39888, .F. ) ;
#6936 = CARTESIAN_POINT ( 'NONE',  ( 26.62151981922250243, 40.00000000000000000, -3.482817046706076169 ) ) ;
#6937 = DIRECTION ( 'NONE',  ( 0.000000000000000000, 0.000000000000000000, -1.000000000000000000 ) ) ;
#6938 = FACE_OUTER_BOUND ( 'NONE', #28430, .T. ) ;
#6939 = DIRECTION ( 'NONE',  ( 0.000000000000000000, 0.000000000000000000, 1.000000000000000000 ) ) ;
#6940 = EDGE_CURVE ( 'NONE', #34149, #28377, #17006, .T. ) ;
#6941 = DIRECTION ( 'NONE',  ( -1.000000000000000000, 0.000000000000000000, 0.000000000000000000 ) ) ;
#6942 = ORIENTED_EDGE ( 'NONE', *, *, #2892, .T. ) ;
#6944 = CARTESIAN_POINT ( 'NONE',  ( 17.99999999999999645, 26.29521155129873833, -17.34211205339320117 ) ) ;
#6943 = DIRECTION ( 'NONE',  ( -1.000000000000000000, 0.000000000000000000, 0.000000000000000000 ) ) ;
#6945 = ORIENTED_EDGE ( 'NONE', *, *, #34059, .T. ) ;
#6946 = CIRCLE ( 'NONE', #36904, 31.49900000000000233 ) ;
#6947 = SURFACE_STYLE_USAGE ( .BOTH. , #27864 ) ;
#6948 = CYLINDRICAL_SURFACE ( 'NONE', #38455, 20.00000000000000355 ) ;
#6949 = VECTOR ( 'NONE', #17211, 1000.000000000000000 ) ;
#6951 = CARTESIAN_POINT ( 'NONE',  ( -13.09503298281258132, 31.00000000000000355, -17.05789676611946959 ) ) ;
#6950 = AXIS2_PLACEMENT_3D ( 'NONE', #24322, #4628, #18004 ) ;
#6952 = VERTEX_POINT ( 'NONE', #2016 ) ;
#6953 = DIRECTION ( 'NONE',  ( 0.000000000000000000, 0.6845471059286899473, -0.7289686274214103312 ) ) ;
#6954 = DIRECTION ( 'NONE',  ( 3.009274222672345096E-17, 1.000000000000000000, -2.455023325076454960E-18 ) ) ;
#6955 = CONTEXT_DEPENDENT_SHAPE_REPRESENTATION ( #30111, #22464 ) ;
#6956 = DIRECTION ( 'NONE',  ( -1.000000000000000000, -0.000000000000000000, -0.000000000000000000 ) ) ;
#6957 = CARTESIAN_POINT ( 'NONE',  ( -47.15756294055117337, 31.00000000000000355, -53.75246728999482571 ) ) ;
#6958 = ORIENTED_EDGE ( 'NONE', *, *, #19279, .T. ) ;
#6959 = CARTESIAN_POINT ( 'NONE',  ( 20.11321884379921343, 31.00000000000000355, -40.61652209561064097 ) ) ;
#6960 = EDGE_CURVE ( 'NONE', #11221, #23796, #12515, .T. ) ;
#6961 = CARTESIAN_POINT ( 'NONE',  ( -47.90394619311608437, 40.00000000000000000, 62.45286580340285099 ) ) ;
#6962 = DIRECTION ( 'NONE',  ( 0.000000000000000000, 0.000000000000000000, 1.000000000000000000 ) ) ;
#6963 = DIRECTION ( 'NONE',  ( 0.000000000000000000, 0.000000000000000000, 1.000000000000000000 ) ) ;
#6964 = EDGE_CURVE ( 'NONE', #4247, #33656, #39241, .T. ) ;
#6965 = ORIENTED_EDGE ( 'NONE', *, *, #39822, .T. ) ;
#6966 = LINE ( 'NONE', #178, #2314 ) ;
#6967 = DIRECTION ( 'NONE',  ( 0.000000000000000000, 0.000000000000000000, 1.000000000000000000 ) ) ;
#6968 = EDGE_CURVE ( 'NONE', #17810, #25329, #37856, .T. ) ;
#6969 = EDGE_LOOP ( 'NONE', ( #40720, #11249, #43014, #20666 ) ) ;
#6970 = CARTESIAN_POINT ( 'NONE',  ( -35.70415035507907930, 40.00000000000000000, 46.55071329160319493 ) ) ;
#6971 = DIRECTION ( 'NONE',  ( -1.000000000000000000, 0.000000000000000000, 0.000000000000000000 ) ) ;
#6973 = CARTESIAN_POINT ( 'NONE',  ( 18.00000000000000355, -46.21320724403641833, -10.97699764142002188 ) ) ;
#6972 = AXIS2_PLACEMENT_3D ( 'NONE', #20980, #9866, #23219 ) ;
#6974 = CIRCLE ( 'NONE', #20263, 10.49999999999999467 ) ;
#6975 = VERTEX_POINT ( 'NONE', #5523 ) ;
#6976 = ADVANCED_FACE ( 'NONE', ( #42777 ), #38889, .F. ) ;
#6977 = DIRECTION ( 'NONE',  ( 0.000000000000000000, 0.000000000000000000, 1.000000000000000000 ) ) ;
#6978 = DIRECTION ( 'NONE',  ( 3.009274222672345096E-17, 1.000000000000000000, -2.455023325076454960E-18 ) ) ;
#6979 = CIRCLE ( 'NONE', #30708, 116.0000000000000000 ) ;
#6980 = ORIENTED_EDGE ( 'NONE', *, *, #17101, .F. ) ;
#6981 = CYLINDRICAL_SURFACE ( 'NONE', #6095, 31.49899999999999878 ) ;
#6982 = ORIENTED_EDGE ( 'NONE', *, *, #35256, .T. ) ;
#6983 = ORIENTED_EDGE ( 'NONE', *, *, #39345, .F. ) ;
#6984 = CARTESIAN_POINT ( 'NONE',  ( 17.99999999999999645, 11.49545354908936545, 29.80986809967263085 ) ) ;
#6985 = CARTESIAN_POINT ( 'NONE',  ( -79.17211737996690601, 31.00000000000000711, 45.58486055166099504 ) ) ;
#6986 = ORIENTED_EDGE ( 'NONE', *, *, #16651, .F. ) ;
#6987 = CARTESIAN_POINT ( 'NONE',  ( 20.00000000000000000, 2.449293598294706513E-15, -20.00000000000000000 ) ) ;
#6988 = DIRECTION ( 'NONE',  ( -1.000000000000000000, 0.000000000000000000, -0.000000000000000000 ) ) ;
#6989 = DIRECTION ( 'NONE',  ( -1.000000000000000000, -0.000000000000000000, -0.000000000000000000 ) ) ;
#6990 = ORIENTED_EDGE ( 'NONE', *, *, #42389, .F. ) ;
#6991 = EDGE_CURVE ( 'NONE', #27839, #30260, #18880, .T. ) ;
#6992 = DIRECTION ( 'NONE',  ( 1.000000000000000000, 0.000000000000000000, -6.546126324440850663E-16 ) ) ;
#6993 = ADVANCED_FACE ( 'NONE', ( #2647 ), #39092, .F. ) ;
#6994 = DIRECTION ( 'NONE',  ( 0.000000000000000000, -0.7980172272802321665, -0.6026346363792660643 ) ) ;
#6995 = CIRCLE ( 'NONE', #41121, 47.49899999999999523 ) ;
#6996 = EDGE_CURVE ( 'NONE', #7217, #12907, #15578, .T. ) ;
#6998 = DIRECTION ( 'NONE',  ( 0.000000000000000000, 0.000000000000000000, 1.000000000000000000 ) ) ;
#6997 = CARTESIAN_POINT ( 'NONE',  ( 0.000000000000000000, -84.09610293794020208, -74.27057253243097534 ) ) ;
#6999 = AXIS2_PLACEMENT_3D ( 'NONE', #26761, #10164, #6893 ) ;
#7000 = FACE_OUTER_BOUND ( 'NONE', #19164, .T. ) ;
#7001 = ORIENTED_EDGE ( 'NONE', *, *, #12745, .T. ) ;
#7002 = DIRECTION ( 'NONE',  ( 0.000000000000000000, 0.000000000000000000, 1.000000000000000000 ) ) ;
#7003 = CARTESIAN_POINT ( 'NONE',  ( 31.10108666877329853, 31.00000000000000355, 17.95223046116557697 ) ) ;
#7004 = CIRCLE ( 'NONE', #41129, 2.649999999999971934 ) ;
#7005 = ORIENTED_EDGE ( 'NONE', *, *, #7327, .T. ) ;
#7006 = DIRECTION ( 'NONE',  ( -3.996523416598930318E-16, 2.658563593772947863E-15, 1.000000000000000000 ) ) ;
#7007 = AXIS2_PLACEMENT_3D ( 'NONE', #6604, #33449, #17352 ) ;
#7008 = VECTOR ( 'NONE', #20732, 1000.000000000000000 ) ;
#7009 = DIRECTION ( 'NONE',  ( 0.000000000000000000, 0.000000000000000000, 1.000000000000000000 ) ) ;
#7010 = ORIENTED_EDGE ( 'NONE', *, *, #5669, .F. ) ;
#7011 = AXIS2_PLACEMENT_3D ( 'NONE', #23975, #27024, #3423 ) ;
#7012 = CARTESIAN_POINT ( 'NONE',  ( 0.000000000000000000, 58.30069736313799211, -100.2847380560561419 ) ) ;
#7013 = CARTESIAN_POINT ( 'NONE',  ( 20.73284993368543638, 40.00000000000000000, 42.03655757353646294 ) ) ;
#7014 = EDGE_CURVE ( 'NONE', #7783, #14470, #39771, .T. ) ;
#7015 = CARTESIAN_POINT ( 'NONE',  ( -41.92568936861482598, 40.00000000000000000, -5.596851440153165491 ) ) ;
#7016 = EDGE_LOOP ( 'NONE', ( #20071, #3761, #31295, #27188 ) ) ;
#7017 = CARTESIAN_POINT ( 'NONE',  ( 17.99999999999999645, 0.000000000000000000, 0.000000000000000000 ) ) ;
#7018 = CARTESIAN_POINT ( 'NONE',  ( 5.657435538624008755E-15, 4.615443851143735910E-16, 367.6955262170047263 ) ) ;
#7019 = CARTESIAN_POINT ( 'NONE',  ( 8.999999999999998224, -69.72480978689983999, -92.70626138606085931 ) ) ;
#7020 = EDGE_CURVE ( 'NONE', #35191, #16394, #12301, .T. ) ;
#7021 = VERTEX_POINT ( 'NONE', #22563 ) ;
#7022 = CARTESIAN_POINT ( 'NONE',  ( 24.63052733448982323, 40.00000000000000000, -3.251868155982907904 ) ) ;
#7023 = ORIENTED_EDGE ( 'NONE', *, *, #6968, .T. ) ;
#7024 = DIRECTION ( 'NONE',  ( -1.000000000000000000, -0.000000000000000000, -0.000000000000000000 ) ) ;
#7025 = CARTESIAN_POINT ( 'NONE',  ( 17.99999999999999645, 97.19627249181095863, 71.22763238166520239 ) ) ;
#7026 = EDGE_LOOP ( 'NONE', ( #2298, #26518, #18903, #17958 ) ) ;
#7027 = FACE_OUTER_BOUND ( 'NONE', #6031, .T. ) ;
#7028 = CARTESIAN_POINT ( 'NONE',  ( -5.991980000000000750, 2.341154836636396601E-15, -19.11697999999999809 ) ) ;
#7029 = ADVANCED_FACE ( 'NONE', ( #16005 ), #2159, .T. ) ;
#7030 = VERTEX_POINT ( 'NONE', #454 ) ;
#7031 = DIRECTION ( 'NONE',  ( 0.000000000000000000, 0.000000000000000000, 1.000000000000000000 ) ) ;
#7032 = ORIENTED_EDGE ( 'NONE', *, *, #34378, .T. ) ;
#7033 = AXIS2_PLACEMENT_3D ( 'NONE', #2474, #29145, #15618 ) ;
#7034 = CARTESIAN_POINT ( 'NONE',  ( 0.000000000000000000, 73.78980555658606022, 95.26571049922013401 ) ) ;
#7035 = AXIS2_PLACEMENT_3D ( 'NONE', #13460, #10152, #23505 ) ;
#7036 = EDGE_LOOP ( 'NONE', ( #6389, #21781, #2234, #42687 ) ) ;
#7038 = ORIENTED_EDGE ( 'NONE', *, *, #33624, .T. ) ;
#7037 = DIRECTION ( 'NONE',  ( 1.000000000000000000, 0.000000000000000000, 0.000000000000000000 ) ) ;
#7039 = AXIS2_PLACEMENT_3D ( 'NONE', #8455, #21605, #15266 ) ;
#7040 = CARTESIAN_POINT ( 'NONE',  ( 52.50410707182467718, 31.00000000000000000, -40.15145572480454916 ) ) ;
#7041 = EDGE_LOOP ( 'NONE', ( #4014, #35497, #9920, #27224 ) ) ;
#7042 = CARTESIAN_POINT ( 'NONE',  ( 17.99999999999999645, -64.69195966009822030, -96.28577441832322847 ) ) ;
#7043 = AXIS2_PLACEMENT_3D ( 'NONE', #13886, #33052, #27182 ) ;
#7044 = VERTEX_POINT ( 'NONE', #13813 ) ;
#7045 = DIRECTION ( 'NONE',  ( -1.000000000000000000, 0.000000000000000000, -0.000000000000000000 ) ) ;
#7046 = ORIENTED_EDGE ( 'NONE', *, *, #42457, .F. ) ;
#7047 = CARTESIAN_POINT ( 'NONE',  ( -64.43604943162229404, 40.00000000000000711, 49.29347324003091302 ) ) ;
#7048 = ADVANCED_FACE ( 'NONE', ( #6796 ), #30598, .F. ) ;
#7049 = AXIS2_PLACEMENT_3D ( 'NONE', #24222, #5563, #32176 ) ;
#7050 = EDGE_CURVE ( 'NONE', #13399, #40171, #30372, .T. ) ;
#7052 = CARTESIAN_POINT ( 'NONE',  ( 9.000000000000001776, 5.871425383721550872, 51.66745943012283959 ) ) ;
#7051 = CARTESIAN_POINT ( 'NONE',  ( 126.0000000000000284, 1.589209405437102375E-14, 0.000000000000000000 ) ) ;
#7053 = FACE_OUTER_BOUND ( 'NONE', #30563, .T. ) ;
#7054 = ORIENTED_EDGE ( 'NONE', *, *, #6940, .T. ) ;
#7055 = DIRECTION ( 'NONE',  ( -1.000000000000000000, -0.000000000000000000, 0.000000000000000000 ) ) ;
#7056 = VERTEX_POINT ( 'NONE', #13374 ) ;
#7057 = DIRECTION ( 'NONE',  ( -1.000000000000000000, 0.000000000000000000, -0.000000000000000000 ) ) ;
#7058 = ORIENTED_EDGE ( 'NONE', *, *, #29466, .F. ) ;
#7059 = DIRECTION ( 'NONE',  ( -1.000000000000000000, -0.000000000000000000, 0.000000000000000000 ) ) ;
#7060 = CARTESIAN_POINT ( 'NONE',  ( 84.66040299356156140, 31.00000000000000000, 11.14692016787551765 ) ) ;
#7061 = CARTESIAN_POINT ( 'NONE',  ( 17.99999999999999645, -35.89808275599443732, -2.706964063997608694 ) ) ;
#7062 = EDGE_CURVE ( 'NONE', #31919, #9735, #10068, .T. ) ;
#7063 = VERTEX_POINT ( 'NONE', #27112 ) ;
#7064 = EDGE_CURVE ( 'NONE', #11917, #17450, #27114, .T. ) ;
#7065 = CARTESIAN_POINT ( 'NONE',  ( 0.000000000000000000, 0.000000000000000000, 0.000000000000000000 ) ) ;
#7066 = AXIS2_PLACEMENT_3D ( 'NONE', #21707, #21915, #4635 ) ;
#7067 = AXIS2_PLACEMENT_3D ( 'NONE', #36334, #19801, #42663 ) ;
#7068 = ORIENTED_EDGE ( 'NONE', *, *, #25814, .T. ) ;
#7069 = CARTESIAN_POINT ( 'NONE',  ( 0.6920835326022565237, 4.454600218803884459, -3.597382984111579862 ) ) ;
#7070 = DIRECTION ( 'NONE',  ( 0.000000000000000000, 0.000000000000000000, 1.000000000000000000 ) ) ;
#7071 = DIRECTION ( 'NONE',  ( -0.5000000000000051070, 1.060575238724903217E-16, -0.8660254037844355990 ) ) ;
#7072 = CIRCLE ( 'NONE', #31487, 47.49900000000000233 ) ;
#7073 = DIRECTION ( 'NONE',  ( -1.000000000000000000, -0.000000000000000000, -0.000000000000000000 ) ) ;
#7074 = ADVANCED_FACE ( 'NONE', ( #16880 ), #3934, .T. ) ;
#7075 = ORIENTED_EDGE ( 'NONE', *, *, #16584, .F. ) ;
#7076 = CARTESIAN_POINT ( 'NONE',  ( 0.000000000000000000, 0.000000000000000000, -20.00000000000000000 ) ) ;
#7077 = ORIENTED_EDGE ( 'NONE', *, *, #26985, .F. ) ;
#7078 = AXIS2_PLACEMENT_3D ( 'NONE', #20404, #11004, #27578 ) ;
#7079 = CARTESIAN_POINT ( 'NONE',  ( 0.000000000000000000, 0.000000000000000000, 0.000000000000000000 ) ) ;
#7080 = EDGE_CURVE ( 'NONE', #5150, #12532, #36252, .T. ) ;
#7081 = DIRECTION ( 'NONE',  ( -3.996523416598930318E-16, 2.658563593772947863E-15, 1.000000000000000000 ) ) ;
#7082 = LINE ( 'NONE', #36525, #29634 ) ;
#7083 = ORIENTED_EDGE ( 'NONE', *, *, #39545, .F. ) ;
#7084 = ORIENTED_EDGE ( 'NONE', *, *, #2425, .T. ) ;
#7085 = DIRECTION ( 'NONE',  ( -1.000000000000000000, 0.000000000000000000, 0.000000000000000000 ) ) ;
#7086 = DIRECTION ( 'NONE',  ( 0.000000000000000000, -1.243708525996931132E-14, -1.000000000000000000 ) ) ;
#7087 = CARTESIAN_POINT ( 'NONE',  ( 4.000000000001088907, 1.658577278524410170, -3.531553309554541720 ) ) ;
#7089 = EDGE_LOOP ( 'NONE', ( #15824, #34928, #2506, #5938 ) ) ;
#7088 = DIRECTION ( 'NONE',  ( 0.000000000000000000, -0.7980172272802321665, -0.6026346363792661753 ) ) ;
#7090 = CARTESIAN_POINT ( 'NONE',  ( 9.106956811745659408, 31.00000000000000355, -33.78410985267935018 ) ) ;
#7091 = FACE_OUTER_BOUND ( 'NONE', #16629, .T. ) ;
#7093 = ORIENTED_EDGE ( 'NONE', *, *, #17909, .F. ) ;
#7092 = FACE_OUTER_BOUND ( 'NONE', #11632, .T. ) ;
#7094 = VERTEX_POINT ( 'NONE', #32976 ) ;
#7095 = CARTESIAN_POINT ( 'NONE',  ( 17.99999999999999645, -88.56657216608570593, -68.87840567546012949 ) ) ;
#7096 = AXIS2_PLACEMENT_3D ( 'NONE', #36436, #30586, #27303 ) ;
#7097 = LINE ( 'NONE', #23509, #33548 ) ;
#7098 = CARTESIAN_POINT ( 'NONE',  ( -51.85848278221650531, 40.00000000000000000, -6.921372802089502230 ) ) ;
#7099 = AXIS2_PLACEMENT_3D ( 'NONE', #10971, #33429, #13601 ) ;
#7100 = ADVANCED_FACE ( 'NONE', ( #40377 ), #17319, .T. ) ;
#7101 = EDGE_CURVE ( 'NONE', #19749, #29952, #3708, .T. ) ;
#7102 = FACE_OUTER_BOUND ( 'NONE', #7503, .T. ) ;
#7103 = EDGE_CURVE ( 'NONE', #4270, #4705, #13587, .T. ) ;
#7104 = EDGE_CURVE ( 'NONE', #23547, #2401, #11924, .T. ) ;
#7105 = VECTOR ( 'NONE', #13990, 1000.000000000000000 ) ;
#7106 = LINE ( 'NONE', #17409, #4547 ) ;
#7107 = ORIENTED_EDGE ( 'NONE', *, *, #32284, .T. ) ;
#7108 = CYLINDRICAL_SURFACE ( 'NONE', #37679, 59.00000000000000000 ) ;
#7109 = EDGE_LOOP ( 'NONE', ( #41018, #21984, #19106, #8766 ) ) ;
#7110 = VECTOR ( 'NONE', #16205, 1000.000000000000000 ) ;
#7111 = CARTESIAN_POINT ( 'NONE',  ( 0.000000000000000000, 11.65176648921190150, -115.4133282497341355 ) ) ;
#7112 = CARTESIAN_POINT ( 'NONE',  ( 17.99999999999999645, 57.40245293794667703, 96.40140491896650587 ) ) ;
#7113 = CARTESIAN_POINT ( 'NONE',  ( 4.090615425948669781, 31.00000000000000355, -62.60416666561555132 ) ) ;
#7114 = DIRECTION ( 'NONE',  ( 0.000000000000000000, 0.000000000000000000, 1.000000000000000000 ) ) ;
#7115 = VERTEX_POINT ( 'NONE', #27319 ) ;
#7116 = CARTESIAN_POINT ( 'NONE',  ( 146.1418929693599580, -2.055254544495727309, -53.89157828313137344 ) ) ;
#7117 = ORIENTED_EDGE ( 'NONE', *, *, #10567, .T. ) ;
#7118 = CARTESIAN_POINT ( 'NONE',  ( -65.18298466990795248, 31.00000000000000711, 74.32329070269128124 ) ) ;
#7119 = ORIENTED_EDGE ( 'NONE', *, *, #21769, .T. ) ;
#7120 = CYLINDRICAL_SURFACE ( 'NONE', #22900, 59.00000000000000000 ) ;
#7121 = DIRECTION ( 'NONE',  ( 1.000000000000000000, 0.000000000000000000, 0.000000000000000000 ) ) ;
#7122 = CARTESIAN_POINT ( 'NONE',  ( 73.52353481979008620, 31.00000000000000000, 25.08131146961490998 ) ) ;
#7123 = CARTESIAN_POINT ( 'NONE',  ( 77.09314031436157677, 39.99999999999999289, 5.156213784760051766 ) ) ;
#7124 = CARTESIAN_POINT ( 'NONE',  ( 0.000000000000000000, 0.000000000000000000, 0.000000000000000000 ) ) ;
#7125 = EDGE_CURVE ( 'NONE', #15611, #31395, #4213, .T. ) ;
#7126 = ORIENTED_EDGE ( 'NONE', *, *, #27280, .F. ) ;
#7127 = DIRECTION ( 'NONE',  ( 1.000000000000000000, 0.000000000000000000, 0.000000000000000000 ) ) ;
#7128 = ORIENTED_EDGE ( 'NONE', *, *, #6289, .T. ) ;
#7129 = DIRECTION ( 'NONE',  ( 1.000000000000000000, 0.000000000000000000, 0.000000000000000000 ) ) ;
#7130 = AXIS2_PLACEMENT_3D ( 'NONE', #21474, #18408, #5483 ) ;
#7131 = DIRECTION ( 'NONE',  ( 0.000000000000000000, 1.331914804436429787E-14, -1.000000000000000000 ) ) ;
#7132 = CIRCLE ( 'NONE', #18350, 58.99999999999998579 ) ;
#7134 = ORIENTED_EDGE ( 'NONE', *, *, #39605, .F. ) ;
#7133 = CARTESIAN_POINT ( 'NONE',  ( 17.99999999999999645, -21.48775762007842260, -23.64423737150161031 ) ) ;
#7135 = DIRECTION ( 'NONE',  ( 0.000000000000000000, 0.000000000000000000, 1.000000000000000000 ) ) ;
#7136 = ORIENTED_EDGE ( 'NONE', *, *, #22618, .T. ) ;
#7137 = CARTESIAN_POINT ( 'NONE',  ( 0.000000000000000000, -110.3490479609630910, 38.71798610214488434 ) ) ;
#7138 = CARTESIAN_POINT ( 'NONE',  ( -21.28946418274055929, 40.00000000000000000, -79.45670318283352174 ) ) ;
#7139 = CARTESIAN_POINT ( 'NONE',  ( 0.000000000000000000, 35.78425302087543969, -3.935382540232422510 ) ) ;
#7140 = AXIS2_PLACEMENT_3D ( 'NONE', #1744, #8084, #37747 ) ;
#7141 = EDGE_LOOP ( 'NONE', ( #37664, #38819, #32957, #42464 ) ) ;
#7142 = LINE ( 'NONE', #40510, #17170 ) ;
#7143 = DIRECTION ( 'NONE',  ( 0.000000000000000000, 0.000000000000000000, 1.000000000000000000 ) ) ;
#7144 = EDGE_LOOP ( 'NONE', ( #16694, #32181 ) ) ;
#7145 = EDGE_LOOP ( 'NONE', ( #35469, #3560, #17875, #32543 ) ) ;
#7146 = CARTESIAN_POINT ( 'NONE',  ( 0.000000000000000000, 0.000000000000000000, 52.00000000000000711 ) ) ;
#7147 = ORIENTED_EDGE ( 'NONE', *, *, #26349, .T. ) ;
#7148 = CYLINDRICAL_SURFACE ( 'NONE', #4622, 36.00000000000000000 ) ;
#7149 = CARTESIAN_POINT ( 'NONE',  ( 42.80287614962790599, -34.05525454449571754, 69.29271901957253021 ) ) ;
#7150 = DIRECTION ( 'NONE',  ( -1.000000000000000000, 0.000000000000000000, 0.000000000000000000 ) ) ;
#7151 = DIRECTION ( 'NONE',  ( 0.000000000000000000, -6.887872625202028030E-15, 1.000000000000000000 ) ) ;
#7152 = EDGE_CURVE ( 'NONE', #29060, #31074, #3058, .T. ) ;
#7153 = EDGE_CURVE ( 'NONE', #25529, #30264, #42279, .T. ) ;
#7154 = LINE ( 'NONE', #4523, #13033 ) ;
#7155 = VERTEX_POINT ( 'NONE', #33204 ) ;
#7157 = LINE ( 'NONE', #34003, #16492 ) ;
#7156 = CYLINDRICAL_SURFACE ( 'NONE', #17534, 116.0000000000000000 ) ;
#7158 = ADVANCED_FACE ( 'NONE', ( #29951 ), #40184, .T. ) ;
#7159 = ORIENTED_EDGE ( 'NONE', *, *, #13876, .F. ) ;
#7160 = AXIS2_PLACEMENT_3D ( 'NONE', #43114, #33080, #30480 ) ;
#7161 = CARTESIAN_POINT ( 'NONE',  ( 0.000000000000000000, 0.000000000000000000, 0.000000000000000000 ) ) ;
#7162 = CARTESIAN_POINT ( 'NONE',  ( -9.654069774896838041, 31.00000000000000355, -19.56573356436190636 ) ) ;
#7163 = ORIENTED_EDGE ( 'NONE', *, *, #19658, .F. ) ;
#7164 = CYLINDRICAL_SURFACE ( 'NONE', #41296, 59.00000000000000000 ) ;
#7165 = AXIS2_PLACEMENT_3D ( 'NONE', #8011, #21808, #2096 ) ;
#7166 = LINE ( 'NONE', #21406, #41763 ) ;
#7167 = DIRECTION ( 'NONE',  ( -1.000000000000000000, -0.000000000000000000, -0.000000000000000000 ) ) ;
#7168 = CARTESIAN_POINT ( 'NONE',  ( -41.80404827410195168, 31.00000000000000355, 54.50178954758867889 ) ) ;
#7169 = CIRCLE ( 'NONE', #169, 116.0000000000000000 ) ;
#7170 = ADVANCED_FACE ( 'NONE', ( #16429 ), #4, .T. ) ;
#7171 = EDGE_LOOP ( 'NONE', ( #11799, #34309, #36782, #30069 ) ) ;
#7172 = CARTESIAN_POINT ( 'NONE',  ( 12.64472494877221997, 31.00000000000000355, 47.53373494968589341 ) ) ;
#7173 = CARTESIAN_POINT ( 'NONE',  ( -5.399612364985466151, 40.00000000000000000, -82.39583333413678190 ) ) ;
#7174 = CARTESIAN_POINT ( 'NONE',  ( 0.000000000000000000, 0.000000000000000000, 0.000000000000000000 ) ) ;
#7175 = DIRECTION ( 'NONE',  ( 0.000000000000000000, 0.3641605752528230266, -0.9313361774523380987 ) ) ;
#7176 = ORIENTED_EDGE ( 'NONE', *, *, #8988, .T. ) ;
#7177 = CARTESIAN_POINT ( 'NONE',  ( 17.99999999999999645, 23.21237537461745859, 109.7700237000592836 ) ) ;
#7178 = ADVANCED_FACE ( 'NONE', ( #8098 ), #7446, .F. ) ;
#7179 = CARTESIAN_POINT ( 'NONE',  ( 52.26814377733353467, -2.055254544495723756, -19.42827587850796434 ) ) ;
#7180 = AXIS2_PLACEMENT_3D ( 'NONE', #41986, #15423, #15622 ) ;
#7181 = VERTEX_POINT ( 'NONE', #31012 ) ;
#7182 = CARTESIAN_POINT ( 'NONE',  ( -15.01009539198478748, 40.00000000000000000, 56.06562763604418365 ) ) ;
#7183 = DIRECTION ( 'NONE',  ( 0.000000000000000000, 0.000000000000000000, 1.000000000000000000 ) ) ;
#7184 = CARTESIAN_POINT ( 'NONE',  ( 0.000000000000000000, 0.000000000000000000, -25.00000000000000000 ) ) ;
#7185 = ORIENTED_EDGE ( 'NONE', *, *, #11532, .F. ) ;
#7186 = FACE_OUTER_BOUND ( 'NONE', #37879, .T. ) ;
#7187 = CARTESIAN_POINT ( 'NONE',  ( -17.44537629401975920, 31.00000000000000711, 4.261559264950522952 ) ) ;
#7188 = VERTEX_POINT ( 'NONE', #4597 ) ;
#7189 = DIRECTION ( 'NONE',  ( -1.000000000000000000, 0.000000000000000000, 0.000000000000000000 ) ) ;
#7190 = VERTEX_POINT ( 'NONE', #30803 ) ;
#7191 = COLOUR_RGB ( '', 0.08235294, 0.09019608, 0.10196078) ;
#7192 = CYLINDRICAL_SURFACE ( 'NONE', #41334, 59.00000000000000000 ) ;
#7193 = VECTOR ( 'NONE', #23304, 1000.000000000000000 ) ;
#7194 = ORIENTED_EDGE ( 'NONE', *, *, #17419, .T. ) ;
#7195 = FACE_OUTER_BOUND ( 'NONE', #35684, .T. ) ;
#7196 = CYLINDRICAL_SURFACE ( 'NONE', #41575, 120.5010000000000190 ) ;
#7197 = ORIENTED_EDGE ( 'NONE', *, *, #7062, .T. ) ;
#7198 = CARTESIAN_POINT ( 'NONE',  ( 17.99999999999999645, 111.8797445107944810, -8.437727291343108504 ) ) ;
#7199 = EDGE_CURVE ( 'NONE', #42739, #26154, #19350, .T. ) ;
#7200 = DIRECTION ( 'NONE',  ( 0.000000000000000000, -0.9618256431728219313, 0.2736629900720728981 ) ) ;
#7202 = ORIENTED_EDGE ( 'NONE', *, *, #25448, .F. ) ;
#7201 = AXIS2_PLACEMENT_3D ( 'NONE', #34044, #4347, #24268 ) ;
#7203 = DIRECTION ( 'NONE',  ( 0.000000000000000000, 0.9714298932647106311, -0.2373266998711119624 ) ) ;
#7204 =( REPRESENTATION_RELATIONSHIP ('NONE','NONE', #330, #9026 ) REPRESENTATION_RELATIONSHIP_WITH_TRANSFORMATION ( #34431 )SHAPE_REPRESENTATION_RELATIONSHIP( ) );
#7205 = FACE_OUTER_BOUND ( 'NONE', #20226, .T. ) ;
#7206 = AXIS2_PLACEMENT_3D ( 'NONE', #27818, #18031, #40861 ) ;
#7208 = CARTESIAN_POINT ( 'NONE',  ( 0.000000000000000000, 0.000000000000000000, -1.199999999999999956 ) ) ;
#7207 = DIRECTION ( 'NONE',  ( -1.000000000000000000, 0.000000000000000000, 0.000000000000000000 ) ) ;
#7209 = AXIS2_PLACEMENT_3D ( 'NONE', #38402, #31446, #5246 ) ;
#7210 = CARTESIAN_POINT ( 'NONE',  ( -19.99999999999999645, 17.11489954122026447, 0.000000000000000000 ) ) ;
#7211 = ORIENTED_EDGE ( 'NONE', *, *, #15710, .T. ) ;
#7212 = EDGE_CURVE ( 'NONE', #16407, #35106, #13761, .T. ) ;
#7213 = DIRECTION ( 'NONE',  ( -4.329780281177428835E-17, 1.000000000000000000, 4.329780281177504023E-17 ) ) ;
#7215 = AXIS2_PLACEMENT_3D ( 'NONE', #14897, #31025, #14684 ) ;
#7214 = DIRECTION ( 'NONE',  ( -1.000000000000000000, -0.000000000000000000, -0.000000000000000000 ) ) ;
#7216 = CARTESIAN_POINT ( 'NONE',  ( -35.29531037056285214, 31.00000000000000355, 17.40921588598563119 ) ) ;
#7217 = VERTEX_POINT ( 'NONE', #34487 ) ;
#7218 = CARTESIAN_POINT ( 'NONE',  ( 17.99999999999999645, 21.48775762007893420, -23.64423737150114135 ) ) ;
#7219 = EDGE_CURVE ( 'NONE', #30344, #42093, #33945, .T. ) ;
#7220 = DIRECTION ( 'NONE',  ( -1.000000000000000000, 0.000000000000000000, 0.000000000000000000 ) ) ;
#7221 = ORIENTED_EDGE ( 'NONE', *, *, #21450, .F. ) ;
#7222 = EDGE_CURVE ( 'NONE', #31709, #41179, #476, .T. ) ;
#7223 = CYLINDRICAL_SURFACE ( 'NONE', #8742, 59.00000000000000000 ) ;
#7224 = CARTESIAN_POINT ( 'NONE',  ( 48.77780477658175329, 40.00000000000000000, -24.05648398140741406 ) ) ;
#7225 = CARTESIAN_POINT ( 'NONE',  ( 6.367266499441480931, 40.00000000000000000, 48.98256792610028754 ) ) ;
#7226 = AXIS2_PLACEMENT_3D ( 'NONE', #10959, #24290, #29794 ) ;
#7227 = VERTEX_POINT ( 'NONE', #31243 ) ;
#7228 = LINE ( 'NONE', #33856, #6093 ) ;
#7229 = VECTOR ( 'NONE', #28599, 1000.000000000000000 ) ;
#7230 = CYLINDRICAL_SURFACE ( 'NONE', #42624, 12.50000000000000000 ) ;
#7231 = ORIENTED_EDGE ( 'NONE', *, *, #30431, .F. ) ;
#7232 = CARTESIAN_POINT ( 'NONE',  ( -19.47536345555549886, 40.00000000000000000, -6.605835105517199324 ) ) ;
#7233 = ORIENTED_EDGE ( 'NONE', *, *, #39803, .T. ) ;
#7234 = CARTESIAN_POINT ( 'NONE',  ( 17.99999999999999645, -28.57802095670076881, -14.28532136906702732 ) ) ;
#7235 = EDGE_CURVE ( 'NONE', #4843, #33515, #14889, .T. ) ;
#7236 = DIRECTION ( 'NONE',  ( -1.000000000000000000, 1.577021341797063787E-16, 0.000000000000000000 ) ) ;
#7237 = CIRCLE ( 'NONE', #36504, 10.99999999999998934 ) ;
#7238 = EDGE_LOOP ( 'NONE', ( #24982, #23979, #34518, #26798 ) ) ;
#7239 = DIRECTION ( 'NONE',  ( 1.000000000000000000, 0.000000000000000000, 0.000000000000000000 ) ) ;
#7240 = AXIS2_PLACEMENT_3D ( 'NONE', #2798, #23360, #22513 ) ;
#7241 = DIRECTION ( 'NONE',  ( 3.996523416598930318E-16, -2.658563593772947863E-15, -1.000000000000000000 ) ) ;
#7242 = ORIENTED_EDGE ( 'NONE', *, *, #3906, .F. ) ;
#7243 = CARTESIAN_POINT ( 'NONE',  ( -19.99999999999998224, -6.025457873503436795E-14, -40.00000000000000711 ) ) ;
#7244 = ORIENTED_EDGE ( 'NONE', *, *, #133, .F. ) ;
#7245 = CARTESIAN_POINT ( 'NONE',  ( 18.00000000000000355, -13.85708833599999856, 45.43276465116660745 ) ) ;
#7246 = VECTOR ( 'NONE', #25949, 1000.000000000000000 ) ;
#7247 = ORIENTED_EDGE ( 'NONE', *, *, #6141, .F. ) ;
#7249 = VERTEX_POINT ( 'NONE', #11171 ) ;
#7248 = CARTESIAN_POINT ( 'NONE',  ( 0.000000000000000000, 0.000000000000000000, 0.000000000000000000 ) ) ;
#7250 = CARTESIAN_POINT ( 'NONE',  ( -31.81746463534672387, 31.00000000000000355, -55.29958784370775504 ) ) ;
#7251 = ORIENTED_EDGE ( 'NONE', *, *, #38344, .F. ) ;
#7252 = DIRECTION ( 'NONE',  ( 0.000000000000000000, 0.000000000000000000, 1.000000000000000000 ) ) ;
#7253 = AXIS2_PLACEMENT_3D ( 'NONE', #24286, #4589, #24501 ) ;
#7254 = EDGE_CURVE ( 'NONE', #2432, #41661, #20761, .T. ) ;
#7255 = EDGE_LOOP ( 'NONE', ( #38382, #26897, #42841, #11842 ) ) ;
#7256 = CARTESIAN_POINT ( 'NONE',  ( 0.000000000000000000, 0.000000000000000000, 0.000000000000000000 ) ) ;
#7257 = EDGE_LOOP ( 'NONE', ( #38505, #28046, #33452, #11319 ) ) ;
#7258 = CARTESIAN_POINT ( 'NONE',  ( -30.16842255227261660, 40.00000000000000000, -89.21315370691763746 ) ) ;
#7260 = CARTESIAN_POINT ( 'NONE',  ( 0.000000000000000000, 0.000000000000000000, 0.000000000000000000 ) ) ;
#7259 = CARTESIAN_POINT ( 'NONE',  ( 0.000000000000000000, 49.65209126885784485, -15.44894276735497485 ) ) ;
#7261 = DIRECTION ( 'NONE',  ( 0.000000000000000000, 0.000000000000000000, 1.000000000000000000 ) ) ;
#7262 = VERTEX_POINT ( 'NONE', #1329 ) ;
#7263 = DIRECTION ( 'NONE',  ( 0.000000000000000000, 0.000000000000000000, 1.000000000000000000 ) ) ;
#7264 = AXIS2_PLACEMENT_3D ( 'NONE', #2100, #38537, #8661 ) ;
#7265 = ORIENTED_EDGE ( 'NONE', *, *, #356, .F. ) ;
#7266 = ADVANCED_FACE ( 'NONE', ( #7661 ), #4154, .F. ) ;
#7267 = AXIS2_PLACEMENT_3D ( 'NONE', #41009, #34257, #17724 ) ;
#7268 = SURFACE_SIDE_STYLE ('',( #31289 ) ) ;
#7269 = CIRCLE ( 'NONE', #13596, 116.0000000000000000 ) ;
#7270 = DIRECTION ( 'NONE',  ( -1.000000000000000000, -0.000000000000000000, -0.000000000000000000 ) ) ;
#7271 = EDGE_CURVE ( 'NONE', #3192, #6092, #37426, .T. ) ;
#7272 = CARTESIAN_POINT ( 'NONE',  ( 12.12865573427490062, 31.00000000000000355, -92.11205733446308841 ) ) ;
#7273 = CARTESIAN_POINT ( 'NONE',  ( 4.140404888673277384, 2.228338276487440428, -3.686887068327033390 ) ) ;
#7274 = VERTEX_POINT ( 'NONE', #24292 ) ;
#7275 = AXIS2_PLACEMENT_3D ( 'NONE', #34433, #25309, #8680 ) ;
#7276 = EDGE_CURVE ( 'NONE', #23500, #26596, #13351, .T. ) ;
#7277 = CARTESIAN_POINT ( 'NONE',  ( 1.598609366639573350E-14, -1.063425437509180407E-13, -40.00000000000000000 ) ) ;
#7278 = AXIS2_PLACEMENT_3D ( 'NONE', #10425, #30511, #8233 ) ;
#7279 = ORIENTED_EDGE ( 'NONE', *, *, #33479, .F. ) ;
#7280 = FACE_OUTER_BOUND ( 'NONE', #36602, .T. ) ;
#7281 = CARTESIAN_POINT ( 'NONE',  ( 17.99999999999999645, 15.21076497709875497, -119.5371223922153519 ) ) ;
#7282 = DIRECTION ( 'NONE',  ( -1.000000000000000000, 0.000000000000000000, 0.000000000000000000 ) ) ;
#7283 = CARTESIAN_POINT ( 'NONE',  ( 17.99999999999999645, -71.21168426767167148, 86.70160608319299911 ) ) ;
#7284 = ORIENTED_EDGE ( 'NONE', *, *, #31822, .T. ) ;
#7285 = CARTESIAN_POINT ( 'NONE',  ( 0.000000000000000000, -17.33727698085101565, -110.8498592715975519 ) ) ;
#7286 = EDGE_LOOP ( 'NONE', ( #29648, #41949, #311, #5827 ) ) ;
#7287 = EDGE_CURVE ( 'NONE', #5566, #26405, #42579, .T. ) ;
#7288 = DIRECTION ( 'NONE',  ( 0.000000000000000000, 0.000000000000000000, 1.000000000000000000 ) ) ;
#7289 = ADVANCED_FACE ( 'NONE', ( #7876 ), #41242, .F. ) ;
#7290 = FACE_OUTER_BOUND ( 'NONE', #5577, .T. ) ;
#7291 = CARTESIAN_POINT ( 'NONE',  ( 17.99999999999999645, 0.000000000000000000, 0.000000000000000000 ) ) ;
#7292 = ORIENTED_EDGE ( 'NONE', *, *, #8749, .T. ) ;
#7293 = ORIENTED_EDGE ( 'NONE', *, *, #30326, .F. ) ;
#7294 = DIRECTION ( 'NONE',  ( 0.000000000000000000, -1.000000000000000000, 5.297542245118643184E-16 ) ) ;
#7295 = AXIS2_PLACEMENT_3D ( 'NONE', #9526, #2522, #29187 ) ;
#7296 = DIRECTION ( 'NONE',  ( -3.996523416598930318E-16, 2.658563593772947863E-15, 1.000000000000000000 ) ) ;
#7297 = AXIS2_PLACEMENT_3D ( 'NONE', #21167, #33998, #27459 ) ;
#7298 = DIRECTION ( 'NONE',  ( -1.000000000000000000, -0.000000000000000000, 0.000000000000000000 ) ) ;
#7299 = AXIS2_PLACEMENT_3D ( 'NONE', #16572, #2969, #9766 ) ;
#7301 = ORIENTED_EDGE ( 'NONE', *, *, #40139, .F. ) ;
#7300 = FACE_OUTER_BOUND ( 'NONE', #26915, .T. ) ;
#7302 = CARTESIAN_POINT ( 'NONE',  ( 1.888402776346428835, 31.00000000000000355, 29.39821258742166066 ) ) ;
#7303 = VECTOR ( 'NONE', #3278, 1000.000000000000000 ) ;
#7304 = CARTESIAN_POINT ( 'NONE',  ( 0.000000000000000000, 0.000000000000000000, 0.000000000000000000 ) ) ;
#7306 = EDGE_LOOP ( 'NONE', ( #6707, #24571, #7640, #5277 ) ) ;
#7305 = CARTESIAN_POINT ( 'NONE',  ( 17.99999999999999645, -109.3506818544112917, 38.70953859160975696 ) ) ;
#7307 = AXIS2_PLACEMENT_3D ( 'NONE', #10141, #529, #13883 ) ;
#7308 = ORIENTED_EDGE ( 'NONE', *, *, #13297, .F. ) ;
#7309 = CARTESIAN_POINT ( 'NONE',  ( 17.99999999999999645, 0.000000000000000000, 0.000000000000000000 ) ) ;
#7310 = CARTESIAN_POINT ( 'NONE',  ( 46.08863070263672057, 40.00000000000000000, 35.47900410130833393 ) ) ;
#7311 = DIRECTION ( 'NONE',  ( -1.000000000000000000, 0.000000000000000000, 0.000000000000000000 ) ) ;
#7312 = UNCERTAINTY_MEASURE_WITH_UNIT (LENGTH_MEASURE( 1.000000000000000082E-05 ), #38714, 'distance_accuracy_value', 'NONE');
#7313 = CYLINDRICAL_SURFACE ( 'NONE', #35206, 51.99999999999999289 ) ;
#7314 = ORIENTED_EDGE ( 'NONE', *, *, #21729, .T. ) ;
#7315 = CARTESIAN_POINT ( 'NONE',  ( 17.99999999999999645, -111.9370513079672520, 44.61600100275137493 ) ) ;
#7316 = ORIENTED_EDGE ( 'NONE', *, *, #6496, .T. ) ;
#7317 = EDGE_CURVE ( 'NONE', #21574, #36583, #23168, .T. ) ;
#7318 = AXIS2_PLACEMENT_3D ( 'NONE', #21289, #1808, #41733 ) ;
#7319 = CARTESIAN_POINT ( 'NONE',  ( 17.99999999999999645, -74.56001736500675747, 88.86396238369010803 ) ) ;
#7320 = CARTESIAN_POINT ( 'NONE',  ( -10.00000000000000000, 0.000000000000000000, 0.000000000000000000 ) ) ;
#7321 = EDGE_CURVE ( 'NONE', #29070, #22351, #5894, .T. ) ;
#7322 = CARTESIAN_POINT ( 'NONE',  ( 50.09382087749727930, 31.00000000000000355, 24.69014870349942825 ) ) ;
#7323 = DIRECTION ( 'NONE',  ( 0.000000000000000000, 0.000000000000000000, -1.000000000000000000 ) ) ;
#7324 = AXIS2_PLACEMENT_3D ( 'NONE', #19545, #16050, #19335 ) ;
#7325 = EDGE_LOOP ( 'NONE', ( #19158, #18409 ) ) ;
#7326 = CIRCLE ( 'NONE', #1756, 116.0000000000000000 ) ;
#7327 = EDGE_CURVE ( 'NONE', #28038, #20877, #1483, .T. ) ;
#7328 = AXIS2_PLACEMENT_3D ( 'NONE', #7874, #4595, #31241 ) ;
#7329 = VECTOR ( 'NONE', #28651, 1000.000000000000000 ) ;
#7330 = LINE ( 'NONE', #565, #35124 ) ;
#7331 = EDGE_LOOP ( 'NONE', ( #17431, #34256, #4673, #25255 ) ) ;
#7332 = CARTESIAN_POINT ( 'NONE',  ( -25.38139813252123034, 31.00000000000000355, 94.78629358389331117 ) ) ;
#7333 = CIRCLE ( 'NONE', #20620, 120.5010000000000332 ) ;
#7334 = ORIENTED_EDGE ( 'NONE', *, *, #25839, .T. ) ;
#7336 = CIRCLE ( 'NONE', #35918, 120.5010000000000190 ) ;
#7335 = DIRECTION ( 'NONE',  ( -1.000000000000000000, 0.000000000000000000, 0.000000000000000000 ) ) ;
#7337 = CARTESIAN_POINT ( 'NONE',  ( 18.00000000000000355, -44.25018368420762016, 27.31155879685165999 ) ) ;
#7338 = CARTESIAN_POINT ( 'NONE',  ( -36.82253293460209420, 31.00000000000000355, -63.98115709646774718 ) ) ;
#7340 = CARTESIAN_POINT ( 'NONE',  ( -55.03444096782886419, 40.00000000000000000, -48.41538206857744342 ) ) ;
#7339 = AXIS2_PLACEMENT_3D ( 'NONE', #7510, #14088, #27381 ) ;
#7341 = DIRECTION ( 'NONE',  ( 0.000000000000000000, 0.000000000000000000, 1.000000000000000000 ) ) ;
#7342 = AXIS2_PLACEMENT_3D ( 'NONE', #12747, #5953, #31961 ) ;
#7343 = ORIENTED_EDGE ( 'NONE', *, *, #2745, .F. ) ;
#7344 = CARTESIAN_POINT ( 'NONE',  ( 17.99999999999999645, -30.78424799127072120, 6.672111855473074726 ) ) ;
#7345 = ORIENTED_EDGE ( 'NONE', *, *, #16067, .T. ) ;
#7346 = DIRECTION ( 'NONE',  ( -1.000000000000000000, 0.000000000000000000, 0.000000000000000000 ) ) ;
#7347 = EDGE_CURVE ( 'NONE', #1606, #4068, #23823, .T. ) ;
#7348 = DIRECTION ( 'NONE',  ( 0.000000000000000000, 0.000000000000000000, -1.000000000000000000 ) ) ;
#7349 = EDGE_CURVE ( 'NONE', #2475, #5016, #19890, .T. ) ;
#7350 = EDGE_CURVE ( 'NONE', #9086, #1020, #16153, .T. ) ;
#7351 = EDGE_CURVE ( 'NONE', #2623, #34294, #16855, .T. ) ;
#7353 = ORIENTED_EDGE ( 'NONE', *, *, #29125, .F. ) ;
#7352 = DIRECTION ( 'NONE',  ( -1.000000000000000000, 0.000000000000000000, -0.000000000000000000 ) ) ;
#7354 = CYLINDRICAL_SURFACE ( 'NONE', #27485, 59.00000000000000000 ) ;
#7355 = ORIENTED_EDGE ( 'NONE', *, *, #28512, .T. ) ;
#7356 = CARTESIAN_POINT ( 'NONE',  ( 2.000000000000005329, -3.464101615137751722, 0.000000000000000000 ) ) ;
#7357 = CARTESIAN_POINT ( 'NONE',  ( -40.93297376624923345, 40.00000000000000000, -70.86912620794510076 ) ) ;
#7358 = CARTESIAN_POINT ( 'NONE',  ( 0.000000000000000000, 98.39501399267960835, -53.91376164787712355 ) ) ;
#7359 = ORIENTED_EDGE ( 'NONE', *, *, #2534, .T. ) ;
#7360 = DIRECTION ( 'NONE',  ( -0.9470131699890049770, -3.405258028344997528E-16, -0.3211947320043963550 ) ) ;
#7361 = CARTESIAN_POINT ( 'NONE',  ( 9.000000000000001776, -115.5737863835462917, 9.934782381633290527 ) ) ;
#7362 = AXIS2_PLACEMENT_3D ( 'NONE', #21071, #20625, #23464 ) ;
#7363 = EDGE_LOOP ( 'NONE', ( #42998, #4797, #35638, #24445 ) ) ;
#7364 = AXIS2_PLACEMENT_3D ( 'NONE', #42941, #29894, #9999 ) ;
#7365 = AXIS2_PLACEMENT_3D ( 'NONE', #33738, #23312, #43123 ) ;
#7366 = CARTESIAN_POINT ( 'NONE',  ( 0.000000000000000000, 54.09091620264857880, -102.6166301549512525 ) ) ;
#7367 = ORIENTED_EDGE ( 'NONE', *, *, #36779, .F. ) ;
#7368 = DIRECTION ( 'NONE',  ( 0.000000000000000000, 0.000000000000000000, 1.000000000000000000 ) ) ;
#7369 = ORIENTED_EDGE ( 'NONE', *, *, #29885, .F. ) ;
#7370 = DIRECTION ( 'NONE',  ( 0.8660254037844374864, -0.5000000000000018874, 0.000000000000000000 ) ) ;
#7371 = CYLINDRICAL_SURFACE ( 'NONE', #34806, 47.49900000000000233 ) ;
#7372 = CIRCLE ( 'NONE', #403, 116.0000000000000000 ) ;
#7373 = CIRCLE ( 'NONE', #31783, 116.0000000000000000 ) ;
#7374 = DIRECTION ( 'NONE',  ( 0.000000000000000000, 0.4817536741017162671, -0.8763066800438630288 ) ) ;
#7375 = AXIS2_PLACEMENT_3D ( 'NONE', #24591, #3859, #17245 ) ;
#7376 = CARTESIAN_POINT ( 'NONE',  ( 9.000000000000000000, -7.220349212960696761, 35.26849241522661771 ) ) ;
#7377 = ORIENTED_EDGE ( 'NONE', *, *, #31649, .T. ) ;
#7379 = CARTESIAN_POINT ( 'NONE',  ( 8.999999999999998224, 90.81729652456265001, -72.16798910853526650 ) ) ;
#7378 = CARTESIAN_POINT ( 'NONE',  ( 0.000000000000000000, 0.000000000000000000, 0.000000000000000000 ) ) ;
#7381 = ORIENTED_EDGE ( 'NONE', *, *, #40228, .F. ) ;
#7380 = AXIS2_PLACEMENT_3D ( 'NONE', #899, #20834, #41263 ) ;
#7382 = EDGE_CURVE ( 'NONE', #38293, #23352, #26309, .T. ) ;
#7383 = LINE ( 'NONE', #607, #25969 ) ;
#7384 = EDGE_CURVE ( 'NONE', #27389, #36617, #42534, .T. ) ;
#7385 = CARTESIAN_POINT ( 'NONE',  ( 22.42277067908921850, 31.00000000000000355, 12.94072372014797701 ) ) ;
#7386 = ORIENTED_EDGE ( 'NONE', *, *, #31905, .T. ) ;
#7387 = CARTESIAN_POINT ( 'NONE',  ( 8.999999999999998224, 94.52951811191559273, 67.23221107124935259 ) ) ;
#7388 = DIRECTION ( 'NONE',  ( 0.000000000000000000, 0.2113826236296247607, -0.9774033898178666746 ) ) ;
#7389 = CARTESIAN_POINT ( 'NONE',  ( 17.99999999999999645, -23.85344185397118011, -113.5209818126993611 ) ) ;
#7390 = CARTESIAN_POINT ( 'NONE',  ( 49.83821931962687302, 31.00000000000000355, 43.70611527624207326 ) ) ;
#7392 = ORIENTED_EDGE ( 'NONE', *, *, #30286, .F. ) ;
#7391 = CIRCLE ( 'NONE', #33180, 120.5010000000000190 ) ;
#7393 = CARTESIAN_POINT ( 'NONE',  ( -38.37160831357631707, 31.00000000000000355, -19.00137192356237392 ) ) ;
#7394 = AXIS2_PLACEMENT_3D ( 'NONE', #5072, #9201, #35393 ) ;
#7395 = CARTESIAN_POINT ( 'NONE',  ( -61.13902149641835138, 40.00000000000000000, -53.61851653479526902 ) ) ;
#7396 = CIRCLE ( 'NONE', #36628, 59.00000000000000000 ) ;
#7397 = VECTOR ( 'NONE', #33911, 1000.000000000000000 ) ;
#7398 = DIRECTION ( 'NONE',  ( 0.000000000000000000, 0.000000000000000000, 1.000000000000000000 ) ) ;
#7399 = EDGE_CURVE ( 'NONE', #33710, #23971, #16780, .T. ) ;
#7400 = LINE ( 'NONE', #20765, #29134 ) ;
#7401 = CARTESIAN_POINT ( 'NONE',  ( 18.00000000000000355, 0.000000000000000000, 0.000000000000000000 ) ) ;
#7402 = EDGE_CURVE ( 'NONE', #20302, #32639, #37629, .T. ) ;
#7403 = CIRCLE ( 'NONE', #11608, 1.000000000000000666 ) ;
#7404 = EDGE_CURVE ( 'NONE', #9027, #22175, #21682, .T. ) ;
#7405 = EDGE_CURVE ( 'NONE', #10476, #6849, #41840, .T. ) ;
#7407 = ORIENTED_EDGE ( 'NONE', *, *, #38040, .T. ) ;
#7406 = CARTESIAN_POINT ( 'NONE',  ( 0.000000000000000000, -12.30077720129131258, 50.52416135122076923 ) ) ;
#7408 = DIRECTION ( 'NONE',  ( 0.000000000000000000, -0.9048270524660145808, -0.4257792915650830956 ) ) ;
#7409 = DIRECTION ( 'NONE',  ( 1.000000000000000000, 0.000000000000000000, 0.000000000000000000 ) ) ;
#7410 = EDGE_CURVE ( 'NONE', #24289, #38409, #13124, .T. ) ;
#7411 = CIRCLE ( 'NONE', #15786, 20.00000000000000711 ) ;
#7412 = EDGE_LOOP ( 'NONE', ( #17057, #36600 ) ) ;
#7413 = CARTESIAN_POINT ( 'NONE',  ( 42.89889459577944564, 40.00000000000000000, -32.91970121835214513 ) ) ;
#7414 = FACE_OUTER_BOUND ( 'NONE', #14579, .T. ) ;
#7415 = CARTESIAN_POINT ( 'NONE',  ( 17.99999999999999645, 0.000000000000000000, 0.000000000000000000 ) ) ;
#7416 = EDGE_LOOP ( 'NONE', ( #18453, #8451 ) ) ;
#7417 = CARTESIAN_POINT ( 'NONE',  ( 0.000000000000000000, -42.87700105098682002, 107.7847984684003393 ) ) ;
#7418 = CYLINDRICAL_SURFACE ( 'NONE', #15270, 20.00000000000000355 ) ;
#7419 = AXIS2_PLACEMENT_3D ( 'NONE', #13868, #20864, #20208 ) ;
#7420 = EDGE_LOOP ( 'NONE', ( #8523, #35725, #39660, #33761 ) ) ;
#7421 = FACE_OUTER_BOUND ( 'NONE', #34288, .T. ) ;
#7422 = VERTEX_POINT ( 'NONE', #2385 ) ;
#7423 = DIRECTION ( 'NONE',  ( 0.000000000000000000, 0.000000000000000000, 1.000000000000000000 ) ) ;
#7424 = ORIENTED_EDGE ( 'NONE', *, *, #6053, .T. ) ;
#7425 = CARTESIAN_POINT ( 'NONE',  ( 2.649999999999987477, -150.5000000000000284, 10.00000000000000000 ) ) ;
#7426 = CYLINDRICAL_SURFACE ( 'NONE', #35318, 120.5010000000000190 ) ;
#7427 = ORIENTED_EDGE ( 'NONE', *, *, #30677, .T. ) ;
#7428 = DIRECTION ( 'NONE',  ( 0.000000000000000000, 0.000000000000000000, 1.000000000000000000 ) ) ;
#7430 = DIRECTION ( 'NONE',  ( -3.009274222672345096E-17, -1.000000000000000000, 2.455023325076454960E-18 ) ) ;
#7429 = TOROIDAL_SURFACE ( 'NONE', #26941, 14.91999999999999815, 0.08000000000000020983 ) ;
#7431 = ORIENTED_EDGE ( 'NONE', *, *, #3878, .F. ) ;
#7432 = AXIS2_PLACEMENT_3D ( 'NONE', #725, #14086, #18247 ) ;
#7433 = CARTESIAN_POINT ( 'NONE',  ( 0.000000000000000000, 21.56073507908645936, 23.57770962728572428 ) ) ;
#7434 = AXIS2_PLACEMENT_3D ( 'NONE', #40284, #29687, #25987 ) ;
#7435 = CARTESIAN_POINT ( 'NONE',  ( 17.99999999999999645, 11.58753559615485251, 29.77419532459266449 ) ) ;
#7436 = DIRECTION ( 'NONE',  ( 1.000000000000000000, 0.000000000000000000, -0.000000000000000000 ) ) ;
#7437 = CIRCLE ( 'NONE', #37394, 59.00000000000000711 ) ;
#7438 = FACE_OUTER_BOUND ( 'NONE', #28502, .T. ) ;
#7439 = ORIENTED_EDGE ( 'NONE', *, *, #24633, .T. ) ;
#7440 = CARTESIAN_POINT ( 'NONE',  ( 0.000000000000000000, 0.000000000000000000, 0.000000000000000000 ) ) ;
#7441 = VECTOR ( 'NONE', #38812, 1000.000000000000000 ) ;
#7442 = DIRECTION ( 'NONE',  ( 0.000000000000000000, 0.000000000000000000, 1.000000000000000000 ) ) ;
#7443 = CARTESIAN_POINT ( 'NONE',  ( -31.00354902519490352, 31.00000000000000355, -27.18544651223506392 ) ) ;
#7444 = EDGE_LOOP ( 'NONE', ( #36460, #14540, #37342, #6032 ) ) ;
#7445 = VECTOR ( 'NONE', #12127, 1000.000000000000000 ) ;
#7446 = CYLINDRICAL_SURFACE ( 'NONE', #38830, 59.00000000000000000 ) ;
#7447 = ORIENTED_EDGE ( 'NONE', *, *, #1044, .F. ) ;
#7448 = DIRECTION ( 'NONE',  ( -1.000000000000000000, -0.000000000000000000, 0.000000000000000000 ) ) ;
#7449 = CARTESIAN_POINT ( 'NONE',  ( -42.66459923921424036, 40.00000000000000000, 24.64557685607233140 ) ) ;
#7450 = CARTESIAN_POINT ( 'NONE',  ( -48.52617905696451572, 40.00000000000000000, 37.10499320822106029 ) ) ;
#7451 = CARTESIAN_POINT ( 'NONE',  ( 22.90854556226710415, -40.05525454449572464, -74.83297477053821467 ) ) ;
#7452 = DIRECTION ( 'NONE',  ( -1.000000000000000000, 0.000000000000000000, 0.000000000000000000 ) ) ;
#7453 = AXIS2_PLACEMENT_3D ( 'NONE', #37182, #289, #10582 ) ;
#7454 = ADVANCED_FACE ( 'NONE', ( #42327 ), #35762, .F. ) ;
#7455 = ADVANCED_FACE ( 'NONE', ( #36413 ), #12682, .F. ) ;
#7456 = CARTESIAN_POINT ( 'NONE',  ( 18.00000000000000355, -5.871425383721897262, 51.66745943012279696 ) ) ;
#7457 = DIRECTION ( 'NONE',  ( -3.009274222672345096E-17, -1.000000000000000000, 2.455023325076455345E-18 ) ) ;
#7458 = CIRCLE ( 'NONE', #34656, 116.0000000000000000 ) ;
#7459 = CIRCLE ( 'NONE', #14505, 59.00000000000000000 ) ;
#7460 = ADVANCED_FACE ( 'NONE', ( #35568 ), #6527, .F. ) ;
#7461 = ORIENTED_EDGE ( 'NONE', *, *, #22463, .F. ) ;
#7462 = CARTESIAN_POINT ( 'NONE',  ( -28.63582912838407069, 40.00000000000000000, 7.677129336082076705 ) ) ;
#7463 = EDGE_LOOP ( 'NONE', ( #17351, #12263, #14343, #4367 ) ) ;
#7464 = DIRECTION ( 'NONE',  ( -1.000000000000000000, -0.000000000000000000, 0.000000000000000000 ) ) ;
#7465 = FACE_OUTER_BOUND ( 'NONE', #42255, .T. ) ;
#7466 = VECTOR ( 'NONE', #16939, 1000.000000000000000 ) ;
#7467 = AXIS2_PLACEMENT_3D ( 'NONE', #30771, #27498, #40770 ) ;
#7468 = ORIENTED_EDGE ( 'NONE', *, *, #41312, .T. ) ;
#7469 = AXIS2_PLACEMENT_3D ( 'NONE', #21744, #28692, #38685 ) ;
#7470 = DIRECTION ( 'NONE',  ( 0.000000000000000000, 0.4817536741017100499, 0.8763066800438663595 ) ) ;
#7471 = DIRECTION ( 'NONE',  ( 0.000000000000000000, 0.000000000000000000, 1.000000000000000000 ) ) ;
#7472 = ORIENTED_EDGE ( 'NONE', *, *, #25257, .T. ) ;
#7473 = CARTESIAN_POINT ( 'NONE',  ( 9.000000000000001776, -19.12429268481792732, 114.4126803693778669 ) ) ;
#7474 = ORIENTED_EDGE ( 'NONE', *, *, #25003, .T. ) ;
#7475 = FACE_OUTER_BOUND ( 'NONE', #13927, .T. ) ;
#7476 = EDGE_CURVE ( 'NONE', #28925, #7021, #22358, .T. ) ;
#7477 = EDGE_LOOP ( 'NONE', ( #10023, #34154, #23674, #11104 ) ) ;
#7479 = ORIENTED_EDGE ( 'NONE', *, *, #31172, .F. ) ;
#7478 = CYLINDRICAL_SURFACE ( 'NONE', #15346, 116.0000000000000000 ) ;
#7480 = CARTESIAN_POINT ( 'NONE',  ( 76.90008882636698218, 31.00000000000000000, -4.923574515426284215 ) ) ;
#7481 = ORIENTED_EDGE ( 'NONE', *, *, #400, .F. ) ;
#7482 = DIRECTION ( 'NONE',  ( 1.000000000000000000, 0.000000000000000000, 0.000000000000000000 ) ) ;
#7483 = ORIENTED_EDGE ( 'NONE', *, *, #21302, .T. ) ;
#7484 = CARTESIAN_POINT ( 'NONE',  ( 18.00000000000000355, 46.21320724403663860, -10.97699764141904843 ) ) ;
#7485 = VERTEX_POINT ( 'NONE', #26419 ) ;
#7486 = CARTESIAN_POINT ( 'NONE',  ( 24.72345498302142630, 40.00000000000000000, -91.84610802670698604 ) ) ;
#7487 = CIRCLE ( 'NONE', #527, 52.00000000000000000 ) ;
#7489 = DIRECTION ( 'NONE',  ( 0.000000000000000000, 0.000000000000000000, 1.000000000000000000 ) ) ;
#7488 = CARTESIAN_POINT ( 'NONE',  ( 17.99999999999999645, -103.5682682299991342, 43.14958040911493242 ) ) ;
#7490 = DIRECTION ( 'NONE',  ( 0.000000000000000000, 0.000000000000000000, 1.000000000000000000 ) ) ;
#7491 = CARTESIAN_POINT ( 'NONE',  ( 0.000000000000000000, 68.61497464550593861, 99.05794392877625398 ) ) ;
#7492 = AXIS2_PLACEMENT_3D ( 'NONE', #8747, #21886, #15540 ) ;
#7493 = VERTEX_POINT ( 'NONE', #9816 ) ;
#7494 = CIRCLE ( 'NONE', #9590, 31.49899999999999523 ) ;
#7495 =( NAMED_UNIT ( * ) PLANE_ANGLE_UNIT ( ) SI_UNIT ( $, .RADIAN. ) );
#7496 = AXIS2_PLACEMENT_3D ( 'NONE', #42997, #23841, #19706 ) ;
#7497 = LINE ( 'NONE', #506, #28276 ) ;
#7498 = AXIS2_PLACEMENT_3D ( 'NONE', #23065, #30223, #40230 ) ;
#7499 = DIRECTION ( 'NONE',  ( -1.000000000000000000, -0.000000000000000000, -0.000000000000000000 ) ) ;
#7500 = CARTESIAN_POINT ( 'NONE',  ( -5.726861599740728614, 31.00000000000000355, 87.60416666588449175 ) ) ;
#7501 = CARTESIAN_POINT ( 'NONE',  ( 0.5636800770130377947, 4.293361309317166530, -3.531542292954102713 ) ) ;
#7503 = EDGE_LOOP ( 'NONE', ( #34663, #17288, #4289, #23338 ) ) ;
#7502 = VECTOR ( 'NONE', #23656, 1000.000000000000000 ) ;
#7504 = CARTESIAN_POINT ( 'NONE',  ( 3.245924575715140481, 40.00000000000000000, -24.54795925723446359 ) ) ;
#7505 = ORIENTED_EDGE ( 'NONE', *, *, #26558, .F. ) ;
#7506 = AXIS2_PLACEMENT_3D ( 'NONE', #16538, #33073, #9304 ) ;
#7507 = EDGE_LOOP ( 'NONE', ( #31674, #25176, #11373, #29442 ) ) ;
#7508 =( LENGTH_UNIT ( ) NAMED_UNIT ( * ) SI_UNIT ( .MILLI., .METRE. ) );
#7509 = DIRECTION ( 'NONE',  ( 0.000000000000000000, 0.5528000653611945259, -0.8333139190825141762 ) ) ;
#7510 = CARTESIAN_POINT ( 'NONE',  ( 0.000000000000000000, -39.55064067543046491, -25.36340625197400200 ) ) ;
#7511 = ADVANCED_FACE ( 'NONE', ( #33805 ), #20535, .F. ) ;
#7512 = DIRECTION ( 'NONE',  ( 3.996523416598930318E-16, -2.658563593772947863E-15, -1.000000000000000000 ) ) ;
#7513 = ADVANCED_FACE ( 'NONE', ( #4334 ), #13770, .F. ) ;
#7514 = ORIENTED_EDGE ( 'NONE', *, *, #39271, .T. ) ;
#7515 = DIRECTION ( 'NONE',  ( 2.932542530036133930E-17, 1.000000000000000000, -5.216001792149171863E-18 ) ) ;
#7516 = VERTEX_POINT ( 'NONE', #3465 ) ;
#7517 = CARTESIAN_POINT ( 'NONE',  ( -103.7695705685742240, -106.4195705685773135, 9.999999999999751310 ) ) ;
#7518 = AXIS2_PLACEMENT_3D ( 'NONE', #32311, #35575, #2619 ) ;
#7519 = LINE ( 'NONE', #24791, #27007 ) ;
#7520 = FACE_OUTER_BOUND ( 'NONE', #30458, .T. ) ;
#7521 = ORIENTED_EDGE ( 'NONE', *, *, #39650, .T. ) ;
#7522 = ORIENTED_EDGE ( 'NONE', *, *, #9634, .F. ) ;
#7523 = DIRECTION ( 'NONE',  ( 1.000000000000000000, 0.000000000000000000, 0.000000000000000000 ) ) ;
#7524 = AXIS2_PLACEMENT_3D ( 'NONE', #18355, #18568, #38362 ) ;
#7525 = DIRECTION ( 'NONE',  ( 1.000000000000000000, 0.000000000000000000, 0.000000000000000000 ) ) ;
#7526 = EDGE_CURVE ( 'NONE', #7516, #25306, #26498, .T. ) ;
#7527 = AXIS2_PLACEMENT_3D ( 'NONE', #21787, #18294, #5578 ) ;
#7528 = CARTESIAN_POINT ( 'NONE',  ( 17.99999999999999645, -103.4151313792875158, 61.85306461934377609 ) ) ;
#7529 = AXIS2_PLACEMENT_3D ( 'NONE', #9899, #17364, #13419 ) ;
#7530 = VECTOR ( 'NONE', #1605, 1000.000000000000000 ) ;
#7531 = EDGE_LOOP ( 'NONE', ( #41415, #27687, #7686, #2145 ) ) ;
#7533 = VERTEX_POINT ( 'NONE', #27493 ) ;
#7532 = FACE_OUTER_BOUND ( 'NONE', #14000, .T. ) ;
#7534 = EDGE_CURVE ( 'NONE', #20186, #24437, #6298, .T. ) ;
#7535 = CARTESIAN_POINT ( 'NONE',  ( -11.35616125661755937, 31.00000000000000355, -42.69191301634815261 ) ) ;
#7536 = CARTESIAN_POINT ( 'NONE',  ( -10.00000000000000000, 0.000000000000000000, 0.000000000000000000 ) ) ;
#7537 = CIRCLE ( 'NONE', #13826, 52.00000000000000000 ) ;
#7539 = ORIENTED_EDGE ( 'NONE', *, *, #15188, .T. ) ;
#7538 = CARTESIAN_POINT ( 'NONE',  ( 147.8500000000000227, 1.576728355889448963E-12, 10.00000000000000000 ) ) ;
#7540 = ORIENTED_EDGE ( 'NONE', *, *, #11703, .F. ) ;
#7541 = CARTESIAN_POINT ( 'NONE',  ( -10.00000000000000000, 0.000000000000000000, 0.000000000000000000 ) ) ;
#7542 = CARTESIAN_POINT ( 'NONE',  ( 3.791180027291366272, 40.00000000000000000, 59.39995347152935778 ) ) ;
#7543 = CARTESIAN_POINT ( 'NONE',  ( 17.99999999999999645, 117.6086855750634470, 26.24286718912143712 ) ) ;
#7544 = DIRECTION ( 'NONE',  ( 0.000000000000000000, 0.000000000000000000, 1.000000000000000000 ) ) ;
#7545 = ORIENTED_EDGE ( 'NONE', *, *, #10834, .F. ) ;
#7546 = CARTESIAN_POINT ( 'NONE',  ( -2.000000000000007550, -3.464101615137749945, 0.000000000000000000 ) ) ;
#7547 = EDGE_CURVE ( 'NONE', #36084, #23269, #25831, .T. ) ;
#7548 = ORIENTED_EDGE ( 'NONE', *, *, #25557, .T. ) ;
#7549 = EDGE_CURVE ( 'NONE', #2925, #21218, #40765, .T. ) ;
#7550 = CARTESIAN_POINT ( 'NONE',  ( 0.000000000000000000, 115.9750404417044081, -2.406240749597859718 ) ) ;
#7551 = CARTESIAN_POINT ( 'NONE',  ( 17.99999999999999645, -116.0452958106482981, 32.46506308663420270 ) ) ;
#7553 = EDGE_CURVE ( 'NONE', #8886, #22817, #34238, .T. ) ;
#7552 = CARTESIAN_POINT ( 'NONE',  ( -53.27196957865878346, 31.00000000000000711, 26.27224001321920355 ) ) ;
#7554 = AXIS2_PLACEMENT_3D ( 'NONE', #4126, #33816, #634 ) ;
#7555 = DIRECTION ( 'NONE',  ( -1.000000000000000000, -0.000000000000000000, -0.000000000000000000 ) ) ;
#7556 = ORIENTED_EDGE ( 'NONE', *, *, #21032, .T. ) ;
#7557 = CIRCLE ( 'NONE', #26359, 2.649999999999993694 ) ;
#7558 = DIRECTION ( 'NONE',  ( 1.000000000000000000, 0.000000000000000000, 0.000000000000000000 ) ) ;
#7559 = ORIENTED_EDGE ( 'NONE', *, *, #20501, .T. ) ;
#7560 = CARTESIAN_POINT ( 'NONE',  ( 7.411374251232441424, 40.00000000000000000, -21.84767871671174788 ) ) ;
#7561 = ORIENTED_EDGE ( 'NONE', *, *, #20810, .F. ) ;
#7562 = CARTESIAN_POINT ( 'NONE',  ( -10.00000000000000000, 0.000000000000000000, 0.000000000000000000 ) ) ;
#7563 = CARTESIAN_POINT ( 'NONE',  ( -9.000000000000005329, 0.000000000000000000, 0.000000000000000000 ) ) ;
#7564 = CARTESIAN_POINT ( 'NONE',  ( -69.31868535681203980, 31.00000000000000711, 18.45717643660088214 ) ) ;
#7565 = CARTESIAN_POINT ( 'NONE',  ( 72.60479858918233731, 39.99999999999999289, -24.53750584076950858 ) ) ;
#7566 = LINE ( 'NONE', #9967, #6949 ) ;
#7567 = EDGE_CURVE ( 'NONE', #16411, #23201, #33380, .T. ) ;
#7568 = VERTEX_POINT ( 'NONE', #33589 ) ;
#7569 = CARTESIAN_POINT ( 'NONE',  ( 18.00000000000000355, 44.75336757549779776, 14.30704879393622164 ) ) ;
#7570 = EDGE_LOOP ( 'NONE', ( #18173, #9826, #39455, #24551 ) ) ;
#7571 = SURFACE_STYLE_USAGE ( .BOTH. , #37457 ) ;
#7572 = CARTESIAN_POINT ( 'NONE',  ( 17.99999999999999645, -7.749090474611287860, -30.53094492177221397 ) ) ;
#7574 = ORIENTED_EDGE ( 'NONE', *, *, #36768, .F. ) ;
#7573 = CARTESIAN_POINT ( 'NONE',  ( 0.000000000000000000, -93.26762629039475883, 76.29967815892324268 ) ) ;
#7575 = DIRECTION ( 'NONE',  ( 0.000000000000000000, 0.5076658003388351270, 0.8615540813938089570 ) ) ;
#7576 = ORIENTED_EDGE ( 'NONE', *, *, #31830, .F. ) ;
#7577 = DIRECTION ( 'NONE',  ( -1.000000000000000000, -0.000000000000000000, 0.000000000000000000 ) ) ;
#7578 = EDGE_CURVE ( 'NONE', #7188, #43139, #14414, .T. ) ;
#7579 = CARTESIAN_POINT ( 'NONE',  ( 57.06996419936330511, 39.99999999999999289, 65.05326946697847745 ) ) ;
#7580 = DIRECTION ( 'NONE',  ( 0.000000000000000000, -0.9574220383620022368, -0.2886919473396315494 ) ) ;
#7581 = ORIENTED_EDGE ( 'NONE', *, *, #7101, .T. ) ;
#7582 = DIRECTION ( 'NONE',  ( -1.000000000000000000, -0.000000000000000000, 0.000000000000000000 ) ) ;
#7583 = EDGE_CURVE ( 'NONE', #38985, #6569, #22346, .T. ) ;
#7584 = AXIS2_PLACEMENT_3D ( 'NONE', #5219, #41656, #12801 ) ;
#7585 = FACE_OUTER_BOUND ( 'NONE', #15462, .T. ) ;
#7586 = AXIS2_PLACEMENT_3D ( 'NONE', #26533, #39805, #35891 ) ;
#7587 = VERTEX_POINT ( 'NONE', #23809 ) ;
#7588 = AXIS2_PLACEMENT_3D ( 'NONE', #22582, #15593, #28897 ) ;
#7589 = PRESENTATION_STYLE_ASSIGNMENT (( #37474 ) ) ;
#7590 = ORIENTED_EDGE ( 'NONE', *, *, #17042, .T. ) ;
#7591 = LINE ( 'NONE', #30522, #3783 ) ;
#7592 = ORIENTED_EDGE ( 'NONE', *, *, #29530, .T. ) ;
#7593 = CARTESIAN_POINT ( 'NONE',  ( 30.20675218207097501, 40.00000000000000000, 23.25504409023340813 ) ) ;
#7594 = CYLINDRICAL_SURFACE ( 'NONE', #30025, 59.00000000000000711 ) ;
#7595 = FACE_OUTER_BOUND ( 'NONE', #9933, .T. ) ;
#7596 = LINE ( 'NONE', #33999, #18577 ) ;
#7597 = ORIENTED_EDGE ( 'NONE', *, *, #40437, .T. ) ;
#7599 = CARTESIAN_POINT ( 'NONE',  ( -126.0000000000000284, 1.230603612181078346E-13, 1.999999999999952704 ) ) ;
#7598 = CARTESIAN_POINT ( 'NONE',  ( 17.99999999999999645, -23.21237537461820466, 109.7700237000591414 ) ) ;
#7600 = ORIENTED_EDGE ( 'NONE', *, *, #33271, .F. ) ;
#7601 = DIRECTION ( 'NONE',  ( -1.000000000000000000, 0.000000000000000000, 0.000000000000000000 ) ) ;
#7603 = ADVANCED_FACE ( 'NONE', ( #30561 ), #409, .F. ) ;
#7602 = CARTESIAN_POINT ( 'NONE',  ( 16.14498194198480618, 31.00000000000000355, 21.03343489346954698 ) ) ;
#7604 = ORIENTED_EDGE ( 'NONE', *, *, #16720, .F. ) ;
#7605 = DIRECTION ( 'NONE',  ( -1.000000000000000000, 0.000000000000000000, 0.000000000000000000 ) ) ;
#7606 = PRODUCT_RELATED_PRODUCT_CATEGORY ( 'part', '', ( #3607 ) ) ;
#7607 = CARTESIAN_POINT ( 'NONE',  ( 0.000000000000000000, 98.69720329641039314, -60.94966826379810243 ) ) ;
#7608 = DIRECTION ( 'NONE',  ( -1.000000000000000000, -0.000000000000000000, 0.000000000000000000 ) ) ;
#7609 = CARTESIAN_POINT ( 'NONE',  ( -8.856203846296160975, 31.00000000000000355, 67.27320953167645712 ) ) ;
#7610 = ORIENTED_EDGE ( 'NONE', *, *, #30321, .T. ) ;
#7611 = VECTOR ( 'NONE', #30163, 1000.000000000000000 ) ;
#7612 = CARTESIAN_POINT ( 'NONE',  ( 46.89194940766294906, 31.00000000000000355, 6.259973086888626526 ) ) ;
#7613 = CARTESIAN_POINT ( 'NONE',  ( -64.44063486737354651, 40.00000000000000711, -49.42892067282641477 ) ) ;
#7614 = VECTOR ( 'NONE', #27125, 1000.000000000000000 ) ;
#7615 = EDGE_CURVE ( 'NONE', #26682, #24778, #6979, .T. ) ;
#7616 = DIRECTION ( 'NONE',  ( -1.000000000000000000, -0.000000000000000000, -0.000000000000000000 ) ) ;
#7617 = CARTESIAN_POINT ( 'NONE',  ( 0.000000000000000000, 0.000000000000000000, 0.000000000000000000 ) ) ;
#7618 = FACE_OUTER_BOUND ( 'NONE', #22126, .T. ) ;
#7620 = ORIENTED_EDGE ( 'NONE', *, *, #10110, .F. ) ;
#7619 = FACE_OUTER_BOUND ( 'NONE', #43128, .T. ) ;
#7621 = CARTESIAN_POINT ( 'NONE',  ( 17.99999999999999645, -84.62908780824814414, -85.78116633471378805 ) ) ;
#7622 = LINE ( 'NONE', #17046, #16079 ) ;
#7623 = EDGE_CURVE ( 'NONE', #28961, #25672, #15381, .T. ) ;
#7624 = ORIENTED_EDGE ( 'NONE', *, *, #1679, .F. ) ;
#7625 = CARTESIAN_POINT ( 'NONE',  ( -44.11856065373272173, 40.00000000000000000, -25.46949057303769948 ) ) ;
#7626 = CARTESIAN_POINT ( 'NONE',  ( 17.99999999999999645, 98.39501399267960835, -53.91376164787712355 ) ) ;
#7627 = DIRECTION ( 'NONE',  ( -1.000000000000000000, 0.000000000000000000, 0.000000000000000000 ) ) ;
#7628 = ORIENTED_EDGE ( 'NONE', *, *, #12975, .T. ) ;
#7629 = EDGE_CURVE ( 'NONE', #5449, #3132, #20770, .T. ) ;
#7630 = CARTESIAN_POINT ( 'NONE',  ( 0.000000000000000000, 1.592040838891559450E-14, -130.0000000000000000 ) ) ;
#7631 = DIRECTION ( 'NONE',  ( 0.000000000000000000, 0.000000000000000000, -1.000000000000000000 ) ) ;
#7632 = ORIENTED_EDGE ( 'NONE', *, *, #14583, .T. ) ;
#7633 = DIRECTION ( 'NONE',  ( -1.000000000000000000, -0.000000000000000000, -0.000000000000000000 ) ) ;
#7634 = ORIENTED_EDGE ( 'NONE', *, *, #39351, .F. ) ;
#7635 = CYLINDRICAL_SURFACE ( 'NONE', #40637, 20.00000000000000711 ) ;
#7637 = EDGE_LOOP ( 'NONE', ( #42082, #31979, #29703, #28487 ) ) ;
#7636 = VECTOR ( 'NONE', #36336, 1000.000000000000000 ) ;
#7638 = FACE_OUTER_BOUND ( 'NONE', #36973, .T. ) ;
#7639 = CYLINDRICAL_SURFACE ( 'NONE', #32487, 11.00000000000000000 ) ;
#7640 = ORIENTED_EDGE ( 'NONE', *, *, #27370, .T. ) ;
#7641 = VECTOR ( 'NONE', #16189, 1000.000000000000000 ) ;
#7642 = DIRECTION ( 'NONE',  ( 0.000000000000000000, 0.000000000000000000, 1.000000000000000000 ) ) ;
#7643 = DIRECTION ( 'NONE',  ( -1.000000000000000000, 0.000000000000000000, -0.000000000000000000 ) ) ;
#7644 = EDGE_LOOP ( 'NONE', ( #25541, #31101, #16059, #2919 ) ) ;
#7645 = DIRECTION ( 'NONE',  ( -1.000000000000000000, -0.000000000000000000, 0.000000000000000000 ) ) ;
#7646 = CYLINDRICAL_SURFACE ( 'NONE', #27613, 10.99999999999999645 ) ;
#7647 = EDGE_CURVE ( 'NONE', #6443, #9628, #7622, .T. ) ;
#7648 = EDGE_CURVE ( 'NONE', #40120, #35216, #1062, .T. ) ;
#7649 = DIRECTION ( 'NONE',  ( -1.000000000000000000, -0.000000000000000000, -0.000000000000000000 ) ) ;
#7650 = EDGE_CURVE ( 'NONE', #22785, #6740, #20118, .T. ) ;
#7651 = EDGE_CURVE ( 'NONE', #22603, #21952, #28587, .T. ) ;
#7652 = EDGE_CURVE ( 'NONE', #25306, #21207, #15298, .T. ) ;
#7653 = CARTESIAN_POINT ( 'NONE',  ( 17.99999999999999645, 0.000000000000000000, 0.000000000000000000 ) ) ;
#7654 = ORIENTED_EDGE ( 'NONE', *, *, #16361, .F. ) ;
#7655 = CARTESIAN_POINT ( 'NONE',  ( -5.832187760079096936E-15, -12.99999999999999822, 0.000000000000000000 ) ) ;
#7656 = CARTESIAN_POINT ( 'NONE',  ( 0.000000000000000000, -31.11570115861491814, -4.898994019976963266 ) ) ;
#7657 = CARTESIAN_POINT ( 'NONE',  ( 34.28525303991722240, 31.00000000000000355, 9.176237600273646322 ) ) ;
#7658 = ORIENTED_EDGE ( 'NONE', *, *, #32723, .T. ) ;
#7660 = CARTESIAN_POINT ( 'NONE',  ( 0.000000000000000000, 46.21320724403648939, 10.97699764141968970 ) ) ;
#7659 = DIRECTION ( 'NONE',  ( -1.000000000000000000, 0.000000000000000000, 0.000000000000000000 ) ) ;
#7661 = FACE_OUTER_BOUND ( 'NONE', #5820, .T. ) ;
#7662 = VERTEX_POINT ( 'NONE', #1290 ) ;
#7663 = DIRECTION ( 'NONE',  ( -1.000000000000000000, 0.000000000000000000, 0.000000000000000000 ) ) ;
#7664 = CARTESIAN_POINT ( 'NONE',  ( 3.108867721649529958, 40.00000000000000000, 47.39583333474234905 ) ) ;
#7665 = CARTESIAN_POINT ( 'NONE',  ( -35.18788409414197815, 40.00000000000000000, -40.25400722681193599 ) ) ;
#7666 = AXIS2_PLACEMENT_3D ( 'NONE', #24675, #18797, #34673 ) ;
#7667 = CIRCLE ( 'NONE', #41803, 59.00000000000000000 ) ;
#7668 = CARTESIAN_POINT ( 'NONE',  ( 17.99999999999999645, -52.19040376560366923, -99.31985817764231683 ) ) ;
#7669 = CARTESIAN_POINT ( 'NONE',  ( 0.000000000000000000, -112.5220807139885864, 28.19186676675805003 ) ) ;
#7670 = AXIS2_PLACEMENT_3D ( 'NONE', #9190, #12275, #35381 ) ;
#7671 = VECTOR ( 'NONE', #38576, 1000.000000000000000 ) ;
#7672 = DIRECTION ( 'NONE',  ( 0.000000000000000000, 0.000000000000000000, 1.000000000000000000 ) ) ;
#7673 = DIRECTION ( 'NONE',  ( 0.000000000000000000, 0.000000000000000000, 1.000000000000000000 ) ) ;
#7674 = ORIENTED_EDGE ( 'NONE', *, *, #19958, .F. ) ;
#7675 = CARTESIAN_POINT ( 'NONE',  ( 16.14498194198480618, 40.00000000000000000, 21.03343489346954698 ) ) ;
#7676 = ORIENTED_EDGE ( 'NONE', *, *, #17827, .F. ) ;
#7677 = DIRECTION ( 'NONE',  ( 0.000000000000000000, 0.000000000000000000, 1.000000000000000000 ) ) ;
#7678 = DIRECTION ( 'NONE',  ( -1.000000000000000000, 0.000000000000000000, 0.000000000000000000 ) ) ;
#7679 = ORIENTED_EDGE ( 'NONE', *, *, #34743, .T. ) ;
#7680 = EDGE_CURVE ( 'NONE', #31449, #36459, #31619, .T. ) ;
#7681 = DIRECTION ( 'NONE',  ( -1.000000000000000000, -0.000000000000000000, -0.000000000000000000 ) ) ;
#7682 = LINE ( 'NONE', #27135, #23419 ) ;
#7683 = VERTEX_POINT ( 'NONE', #15071 ) ;
#7684 = FACE_OUTER_BOUND ( 'NONE', #14262, .T. ) ;
#7685 = VERTEX_POINT ( 'NONE', #14638 ) ;
#7686 = ORIENTED_EDGE ( 'NONE', *, *, #2305, .T. ) ;
#7688 = EDGE_LOOP ( 'NONE', ( #12648, #38296, #10764, #29972 ) ) ;
#7687 = CYLINDRICAL_SURFACE ( 'NONE', #32073, 59.00000000000000000 ) ;
#7690 = AXIS2_PLACEMENT_3D ( 'NONE', #18610, #22300, #15733 ) ;
#7689 = CARTESIAN_POINT ( 'NONE',  ( 4.991138515316659863, 31.00000000000000355, -74.59332054773635434 ) ) ;
#7691 = ORIENTED_EDGE ( 'NONE', *, *, #38715, .T. ) ;
#7692 = CARTESIAN_POINT ( 'NONE',  ( 1.798435537469519230E-14, -1.196353617197826191E-13, -44.99999999999999289 ) ) ;
#7693 = VECTOR ( 'NONE', #3165, 1000.000000000000000 ) ;
#7694 = ORIENTED_EDGE ( 'NONE', *, *, #14997, .F. ) ;
#7695 = CARTESIAN_POINT ( 'NONE',  ( 106.9999999999993321, -2.424707662641753068E-13, -40.00000000000000000 ) ) ;
#7696 = ORIENTED_EDGE ( 'NONE', *, *, #2078, .F. ) ;
#7697 = CARTESIAN_POINT ( 'NONE',  ( 22.98560153735141043, 40.00000000000000000, 86.26083236265425569 ) ) ;
#7698 = AXIS2_PLACEMENT_3D ( 'NONE', #40462, #752, #88 ) ;
#7699 = CIRCLE ( 'NONE', #2781, 59.00000000000000000 ) ;
#7700 = VECTOR ( 'NONE', #31221, 1000.000000000000000 ) ;
#7702 = DIRECTION ( 'NONE',  ( 0.000000000000000000, 0.000000000000000000, 1.000000000000000000 ) ) ;
#7701 = CARTESIAN_POINT ( 'NONE',  ( 0.000000000000000000, -64.69195966009822030, -96.28577441832322847 ) ) ;
#7703 = ADVANCED_FACE ( 'NONE', ( #24465 ), #35098, .T. ) ;
#7704 = EDGE_CURVE ( 'NONE', #38773, #13970, #28379, .T. ) ;
#7705 = AXIS2_PLACEMENT_3D ( 'NONE', #33339, #10864, #10642 ) ;
#7706 = LINE ( 'NONE', #10554, #42197 ) ;
#7707 = DIRECTION ( 'NONE',  ( 0.000000000000000000, 0.000000000000000000, 1.000000000000000000 ) ) ;
#7708 = ORIENTED_EDGE ( 'NONE', *, *, #39074, .T. ) ;
#7709 =( NAMED_UNIT ( * ) PLANE_ANGLE_UNIT ( ) SI_UNIT ( $, .RADIAN. ) );
#7710 = EDGE_CURVE ( 'NONE', #32276, #37957, #32075, .T. ) ;
#7711 = CARTESIAN_POINT ( 'NONE',  ( 17.99999999999999645, -11.49545354908914518, -29.80986809967271967 ) ) ;
#7712 = CARTESIAN_POINT ( 'NONE',  ( 17.99999999999999645, 0.000000000000000000, 0.000000000000000000 ) ) ;
#7713 = CARTESIAN_POINT ( 'NONE',  ( -70.72766149062127283, 31.00000000000000711, 54.26934393422349956 ) ) ;
#7714 = DIRECTION ( 'NONE',  ( -1.000000000000000000, -0.000000000000000000, -0.000000000000000000 ) ) ;
#7715 = VERTEX_POINT ( 'NONE', #41199 ) ;
#7716 = CARTESIAN_POINT ( 'NONE',  ( 3.798394181604433761, 40.00000000000000000, 29.10671710469611284 ) ) ;
#7717 = ORIENTED_EDGE ( 'NONE', *, *, #11186, .T. ) ;
#7718 = ADVANCED_FACE ( 'NONE', ( #31204 ), #41858, .F. ) ;
#7719 = EDGE_CURVE ( 'NONE', #9615, #30643, #34448, .T. ) ;
#7720 = AXIS2_PLACEMENT_3D ( 'NONE', #40748, #4315, #4098 ) ;
#7721 = ORIENTED_EDGE ( 'NONE', *, *, #6940, .F. ) ;
#7722 = DIRECTION ( 'NONE',  ( 0.000000000000000000, 0.000000000000000000, 1.000000000000000000 ) ) ;
#7723 = DIRECTION ( 'NONE',  ( -0.000000000000000000, -0.000000000000000000, -1.000000000000000000 ) ) ;
#7724 = DIRECTION ( 'NONE',  ( 1.000000000000000000, 0.000000000000000000, 0.000000000000000000 ) ) ;
#7725 = CARTESIAN_POINT ( 'NONE',  ( -91.96080130434573618, -35.35525454449571470, 14.45886780445633946 ) ) ;
#7726 = VECTOR ( 'NONE', #36292, 1000.000000000000000 ) ;
#7727 = ORIENTED_EDGE ( 'NONE', *, *, #19339, .F. ) ;
#7728 = DIRECTION ( 'NONE',  ( -0.000000000000000000, -0.000000000000000000, -1.000000000000000000 ) ) ;
#7729 = EDGE_LOOP ( 'NONE', ( #2433, #8027, #3018, #24779 ) ) ;
#7730 = DIRECTION ( 'NONE',  ( -1.000000000000000000, -0.000000000000000000, -0.000000000000000000 ) ) ;
#7731 = AXIS2_PLACEMENT_3D ( 'NONE', #19976, #10765, #37371 ) ;
#7732 = DIRECTION ( 'NONE',  ( -1.000000000000000000, 0.000000000000000000, 0.000000000000000000 ) ) ;
#7733 = AXIS2_PLACEMENT_3D ( 'NONE', #15413, #26280, #9464 ) ;
#7734 = CYLINDRICAL_SURFACE ( 'NONE', #17982, 20.00000000000000711 ) ;
#7735 = VECTOR ( 'NONE', #23277, 1000.000000000000000 ) ;
#7736 = CARTESIAN_POINT ( 'NONE',  ( 0.000000000000000000, 51.27532863109366446, 99.79535634195144667 ) ) ;
#7737 = ORIENTED_EDGE ( 'NONE', *, *, #10680, .T. ) ;
#7738 = EDGE_CURVE ( 'NONE', #25961, #41859, #10480, .T. ) ;
#7739 = ORIENTED_EDGE ( 'NONE', *, *, #17389, .F. ) ;
#7740 = FACE_OUTER_BOUND ( 'NONE', #13614, .T. ) ;
#7741 = DIRECTION ( 'NONE',  ( 1.000000000000000000, -1.373900992973642263E-15, -3.736327486719295592E-16 ) ) ;
#7742 = CARTESIAN_POINT ( 'NONE',  ( 17.99999999999999645, -30.78424799127072120, 6.672111855473074726 ) ) ;
#7743 = VECTOR ( 'NONE', #20514, 1000.000000000000000 ) ;
#7744 = ORIENTED_EDGE ( 'NONE', *, *, #2075, .F. ) ;
#7746 = VERTEX_POINT ( 'NONE', #38368 ) ;
#7745 = DIRECTION ( 'NONE',  ( -1.000000000000000000, 0.000000000000000000, 0.000000000000000000 ) ) ;
#7747 = CARTESIAN_POINT ( 'NONE',  ( 24.31498657912377226, 31.00000000000000355, 42.27453502171529465 ) ) ;
#7748 = DIRECTION ( 'NONE',  ( 0.000000000000000000, 0.000000000000000000, -1.000000000000000000 ) ) ;
#7749 = AXIS2_PLACEMENT_3D ( 'NONE', #9006, #42573, #12938 ) ;
#7751 = DIRECTION ( 'NONE',  ( 0.000000000000000000, -7.056502275159893199E-15, -1.000000000000000000 ) ) ;
#7750 = DIRECTION ( 'NONE',  ( 0.000000000000000000, 0.000000000000000000, -1.000000000000000000 ) ) ;
#7752 = ORIENTED_EDGE ( 'NONE', *, *, #34213, .T. ) ;
#7753 = CARTESIAN_POINT ( 'NONE',  ( -19.43072497041043079, 40.00000000000000000, 56.92208038676060511 ) ) ;
#7754 = LINE ( 'NONE', #17624, #29150 ) ;
#7755 = ADVANCED_FACE ( 'NONE', ( #11348 ), #41648, .F. ) ;
#7756 = DIRECTION ( 'NONE',  ( 1.000000000000000000, 0.000000000000000000, 0.000000000000000000 ) ) ;
#7757 = ORIENTED_EDGE ( 'NONE', *, *, #24547, .F. ) ;
#7758 = CARTESIAN_POINT ( 'NONE',  ( 17.99999999999999645, 51.27532863109366446, 99.79535634195144667 ) ) ;
#7759 = ORIENTED_EDGE ( 'NONE', *, *, #31886, .T. ) ;
#7760 = CIRCLE ( 'NONE', #35623, 116.0000000000000000 ) ;
#7761 = CARTESIAN_POINT ( 'NONE',  ( 8.919999999999994600, 0.000000000000000000, 0.000000000000000000 ) ) ;
#7762 = DIRECTION ( 'NONE',  ( 0.000000000000000000, 0.000000000000000000, 1.000000000000000000 ) ) ;
#7763 = CIRCLE ( 'NONE', #25225, 20.00000000000000711 ) ;
#7764 = CARTESIAN_POINT ( 'NONE',  ( 28.40420691229738281, 31.00000000000000355, 49.17333623205379922 ) ) ;
#7765 = DIRECTION ( 'NONE',  ( 0.000000000000000000, -0.9968120070307493474, -0.07978610555309324781 ) ) ;
#7766 = VERTEX_POINT ( 'NONE', #4792 ) ;
#7767 = EDGE_CURVE ( 'NONE', #41990, #11322, #34871, .T. ) ;
#7768 = CIRCLE ( 'NONE', #18944, 4.500000000000000888 ) ;
#7769 = EDGE_CURVE ( 'NONE', #25462, #20305, #12887, .T. ) ;
#7770 = DIRECTION ( 'NONE',  ( 1.000000000000000000, 0.000000000000000000, 0.000000000000000000 ) ) ;
#7771 = ORIENTED_EDGE ( 'NONE', *, *, #8265, .F. ) ;
#7772 = CARTESIAN_POINT ( 'NONE',  ( 8.528031178950213231, 40.00000000000000000, -31.86521141804621493 ) ) ;
#7773 = AXIS2_PLACEMENT_3D ( 'NONE', #9895, #12345, #26288 ) ;
#7774 = EDGE_CURVE ( 'NONE', #43001, #27783, #35317, .T. ) ;
#7775 = VERTEX_POINT ( 'NONE', #8283 ) ;
#7776 = FACE_OUTER_BOUND ( 'NONE', #35032, .T. ) ;
#7777 = CARTESIAN_POINT ( 'NONE',  ( 17.99999999999999645, 59.07817985939141181, -105.0250430397503294 ) ) ;
#7778 = CARTESIAN_POINT ( 'NONE',  ( -72.09351246574976813, 31.00000000000000711, -4.825959690424619808 ) ) ;
#7779 = CARTESIAN_POINT ( 'NONE',  ( 61.98103557012430542, 39.99999999999999289, 47.69015029125304039 ) ) ;
#7780 = DIRECTION ( 'NONE',  ( 0.000000000000000000, -0.5963673585385078635, 0.8027116379309587879 ) ) ;
#7781 = ORIENTED_EDGE ( 'NONE', *, *, #27248, .F. ) ;
#7782 = CARTESIAN_POINT ( 'NONE',  ( 18.00000000000000355, -47.00885577955406802, -6.806061952192774989 ) ) ;
#7783 = VERTEX_POINT ( 'NONE', #34888 ) ;
#7784 = CYLINDRICAL_SURFACE ( 'NONE', #11641, 59.00000000000000000 ) ;
#7785 = DIRECTION ( 'NONE',  ( 1.000000000000000000, -0.000000000000000000, 0.000000000000000000 ) ) ;
#7787 = ORIENTED_EDGE ( 'NONE', *, *, #40653, .T. ) ;
#7786 = LINE ( 'NONE', #21798, #6739 ) ;
#7788 = DIRECTION ( 'NONE',  ( 0.000000000000000000, 0.000000000000000000, 1.000000000000000000 ) ) ;
#7789 = EDGE_LOOP ( 'NONE', ( #12020, #43015, #25810, #30858 ) ) ;
#7790 = CARTESIAN_POINT ( 'NONE',  ( 0.000000000000000000, 96.25468616236661035, 72.49500943364525085 ) ) ;
#7791 = CARTESIAN_POINT ( 'NONE',  ( 94.89583333399441756, 39.99999999999999289, -6.217735451874103703 ) ) ;
#7792 = FACE_BOUND ( 'NONE', #25624, .T. ) ;
#7794 = EDGE_CURVE ( 'NONE', #40062, #6784, #32771, .T. ) ;
#7793 = CIRCLE ( 'NONE', #828, 120.5010000000000190 ) ;
#7795 = APPLICATION_CONTEXT ( 'automotive_design' ) ;
#7796 = CIRCLE ( 'NONE', #32185, 47.49900000000000233 ) ;
#7797 = ORIENTED_EDGE ( 'NONE', *, *, #4357, .T. ) ;
#7798 = CARTESIAN_POINT ( 'NONE',  ( 0.000000000000000000, 97.97378550988308632, -62.10585602713662468 ) ) ;
#7799 = CARTESIAN_POINT ( 'NONE',  ( 18.00000000000000355, 0.2227391519123156360, -46.98410307550729215 ) ) ;
#7800 = AXIS2_PLACEMENT_3D ( 'NONE', #18052, #31740, #24366 ) ;
#7801 = CARTESIAN_POINT ( 'NONE',  ( 18.00000000000000355, 46.19362259308835661, 8.585149169758654608 ) ) ;
#7802 = ORIENTED_EDGE ( 'NONE', *, *, #8418, .F. ) ;
#7803 = CYLINDRICAL_SURFACE ( 'NONE', #28171, 20.00000000000000355 ) ;
#7804 = ORIENTED_EDGE ( 'NONE', *, *, #39165, .F. ) ;
#7805 = CARTESIAN_POINT ( 'NONE',  ( 0.000000000000000000, 108.8684555192050425, -27.12806418649509865 ) ) ;
#7807 = CARTESIAN_POINT ( 'NONE',  ( -10.89792128226954482, 40.00000000000000000, -32.25956908328721795 ) ) ;
#7806 = AXIS2_PLACEMENT_3D ( 'NONE', #32551, #9843, #36440 ) ;
#7808 = LINE ( 'NONE', #34415, #25194 ) ;
#7809 = DIRECTION ( 'NONE',  ( -3.996523416598930318E-16, 2.658563593772947863E-15, 1.000000000000000000 ) ) ;
#7810 = CYLINDRICAL_SURFACE ( 'NONE', #32505, 20.00000000000000711 ) ;
#7811 = ORIENTED_EDGE ( 'NONE', *, *, #29679, .F. ) ;
#7813 = CARTESIAN_POINT ( 'NONE',  ( 17.99999999999999645, 64.69195966010022403, -96.28577441832183581 ) ) ;
#7812 = CARTESIAN_POINT ( 'NONE',  ( 9.000000000000001776, 29.86146780999950323, 112.0905559814579675 ) ) ;
#7814 = ADVANCED_FACE ( 'NONE', ( #5436 ), #18800, .T. ) ;
#7815 = ORIENTED_EDGE ( 'NONE', *, *, #29179, .F. ) ;
#7816 = CARTESIAN_POINT ( 'NONE',  ( 17.99999999999999645, -112.1702510623870666, 2.471285140322257323 ) ) ;
#7817 = CARTESIAN_POINT ( 'NONE',  ( -26.30698076681265363, 31.00000000000000355, 12.97770382244945253 ) ) ;
#7818 = ORIENTED_EDGE ( 'NONE', *, *, #12311, .T. ) ;
#7819 = DIRECTION ( 'NONE',  ( 0.000000000000000000, -0.9510565162951565288, 0.3090169943749383474 ) ) ;
#7820 = CARTESIAN_POINT ( 'NONE',  ( 18.00000000000000355, 47.00885577955412487, 6.806061952192453468 ) ) ;
#7821 = ITEM_DEFINED_TRANSFORMATION ( 'NONE', 'NONE', #42769,  #13552 ) ;
#7822 = EDGE_CURVE ( 'NONE', #39558, #6132, #10797, .T. ) ;
#7823 = CARTESIAN_POINT ( 'NONE',  ( 3.999999999999999112, -0.7890432684750902093, -0.04868663549882291247 ) ) ;
#7824 = AXIS2_PLACEMENT_3D ( 'NONE', #33782, #29898, #3655 ) ;
#7825 = CARTESIAN_POINT ( 'NONE',  ( -61.13902149641835138, 31.00000000000000355, -53.61851653479526902 ) ) ;
#7826 = VERTEX_POINT ( 'NONE', #9568 ) ;
#7827 = CARTESIAN_POINT ( 'NONE',  ( 5.928665350384932253, 31.00000000000000355, -44.40877992884582426 ) ) ;
#7828 = CONICAL_SURFACE ( 'NONE', #36369, 2.500000000000000888, 0.9599310885968785900 ) ;
#7829 = ADVANCED_FACE ( 'NONE', ( #35523 ), #33109, .T. ) ;
#7830 = CARTESIAN_POINT ( 'NONE',  ( -36.24314215638268877, 40.00000000000000000, -73.49571118816069770 ) ) ;
#7831 = AXIS2_PLACEMENT_3D ( 'NONE', #10950, #7207, #14221 ) ;
#7832 = DIRECTION ( 'NONE',  ( -1.000000000000000000, -0.000000000000000000, -0.000000000000000000 ) ) ;
#7833 = DIRECTION ( 'NONE',  ( 0.000000000000000000, 0.000000000000000000, 1.000000000000000000 ) ) ;
#7834 = DIRECTION ( 'NONE',  ( -3.009274222672345096E-17, -1.000000000000000000, 2.455023325076454960E-18 ) ) ;
#7836 = ORIENTED_EDGE ( 'NONE', *, *, #9323, .F. ) ;
#7835 = FACE_OUTER_BOUND ( 'NONE', #34167, .T. ) ;
#7837 = CARTESIAN_POINT ( 'NONE',  ( 18.00000000000000355, -46.19362259308839214, 8.585149169758333088 ) ) ;
#7838 = DIRECTION ( 'NONE',  ( -1.000000000000000000, 0.000000000000000000, 0.000000000000000000 ) ) ;
#7839 = EDGE_LOOP ( 'NONE', ( #38943, #13836, #25595, #19842 ) ) ;
#7840 = CARTESIAN_POINT ( 'NONE',  ( -67.35649507452052376, 40.00000000000000711, 18.04843207638801772 ) ) ;
#7841 = DIRECTION ( 'NONE',  ( 0.000000000000000000, 0.000000000000000000, 1.000000000000000000 ) ) ;
#7843 = EDGE_CURVE ( 'NONE', #26674, #39350, #15501, .T. ) ;
#7842 = DIRECTION ( 'NONE',  ( -0.2140725878556641315, -0.9768177553304295824, 0.000000000000000000 ) ) ;
#7844 = EDGE_LOOP ( 'NONE', ( #25517, #10385, #1077, #35013 ) ) ;
#7845 = EDGE_CURVE ( 'NONE', #34783, #19720, #18915, .T. ) ;
#7846 = DIRECTION ( 'NONE',  ( -1.000000000000000000, -0.000000000000000000, 0.000000000000000000 ) ) ;
#7847 = DIRECTION ( 'NONE',  ( 0.000000000000000000, 0.000000000000000000, 1.000000000000000000 ) ) ;
#7848 = ORIENTED_EDGE ( 'NONE', *, *, #23782, .F. ) ;
#7849 = LINE ( 'NONE', #3904, #35366 ) ;
#7850 = ORIENTED_EDGE ( 'NONE', *, *, #35770, .F. ) ;
#7851 = CIRCLE ( 'NONE', #23211, 58.99999999999999289 ) ;
#7852 = CARTESIAN_POINT ( 'NONE',  ( 17.99999999999999645, 63.24564713401792204, 102.5693868539697178 ) ) ;
#7853 = ORIENTED_EDGE ( 'NONE', *, *, #16627, .F. ) ;
#7854 = CYLINDRICAL_SURFACE ( 'NONE', #39724, 13.59999999999999964 ) ;
#7855 = CARTESIAN_POINT ( 'NONE',  ( -44.52253807734693680, 31.00000000000000355, 90.03212995789276363 ) ) ;
#7856 = VERTEX_POINT ( 'NONE', #16130 ) ;
#7857 = CIRCLE ( 'NONE', #39882, 47.49900000000000233 ) ;
#7858 = CARTESIAN_POINT ( 'NONE',  ( 17.99999999999999645, 83.49789599728902090, -86.88263557826680028 ) ) ;
#7859 = CARTESIAN_POINT ( 'NONE',  ( 18.00000000000000355, 30.93515269692114344, 36.04401931830261674 ) ) ;
#7860 = ORIENTED_EDGE ( 'NONE', *, *, #11291, .T. ) ;
#7861 = CARTESIAN_POINT ( 'NONE',  ( 18.00000000000000355, 0.000000000000000000, 0.000000000000000000 ) ) ;
#7862 = EDGE_CURVE ( 'NONE', #2989, #15836, #5641, .T. ) ;
#7863 = AXIS2_PLACEMENT_3D ( 'NONE', #3228, #389, #33573 ) ;
#7864 = DIRECTION ( 'NONE',  ( -1.000000000000000000, 0.000000000000000000, 0.000000000000000000 ) ) ;
#7865 = CARTESIAN_POINT ( 'NONE',  ( 17.99999999999999645, -83.58328028049608349, -80.43528614701409651 ) ) ;
#7866 = CYLINDRICAL_SURFACE ( 'NONE', #25154, 120.5010000000000190 ) ;
#7867 = VERTEX_POINT ( 'NONE', #39209 ) ;
#7868 = DIRECTION ( 'NONE',  ( -0.3475381258641427329, 1.166608493463239706E-16, 0.9376658525673413624 ) ) ;
#7869 = EDGE_CURVE ( 'NONE', #9771, #22661, #29012, .T. ) ;
#7870 = CARTESIAN_POINT ( 'NONE',  ( 0.000000000000000000, -30.03615769709704608, -42.44795908869020451 ) ) ;
#7871 = CARTESIAN_POINT ( 'NONE',  ( -45.59965607524345899, 31.00000000000000355, -22.47439267160796916 ) ) ;
#7872 = ORIENTED_EDGE ( 'NONE', *, *, #23023, .F. ) ;
#7874 = CARTESIAN_POINT ( 'NONE',  ( 0.000000000000000000, 0.000000000000000000, 0.000000000000000000 ) ) ;
#7873 = DIRECTION ( 'NONE',  ( -1.000000000000000000, -0.000000000000000000, -0.000000000000000000 ) ) ;
#7875 = EDGE_CURVE ( 'NONE', #42975, #29643, #20300, .T. ) ;
#7876 = FACE_OUTER_BOUND ( 'NONE', #34785, .T. ) ;
#7877 = ORIENTED_EDGE ( 'NONE', *, *, #5940, .F. ) ;
#7878 = SHAPE_REPRESENTATION ( 'needle roller bearing_nh_iso_ISO 3245 - 3022D - 20,SI,NC,20', ( #13552 ), #4416 ) ;
#7879 = EDGE_CURVE ( 'NONE', #14699, #41127, #6, .T. ) ;
#7880 = CARTESIAN_POINT ( 'NONE',  ( 9.000000000000001776, 43.55304910509406113, 28.41006711800000062 ) ) ;
#7881 = CARTESIAN_POINT ( 'NONE',  ( -3.108867721649295035, 40.00000000000000000, 47.60416666525765095 ) ) ;
#7882 = CARTESIAN_POINT ( 'NONE',  ( 50.14038141241296387, 40.00000000000000000, 29.06424286984033145 ) ) ;
#7883 = CYLINDRICAL_SURFACE ( 'NONE', #1162, 116.0000000000000000 ) ;
#7884 = CARTESIAN_POINT ( 'NONE',  ( 17.99999999999999645, 29.68570942776486987, -10.53307442156903662 ) ) ;
#7885 = CARTESIAN_POINT ( 'NONE',  ( 0.000000000000000000, 52.88069566989454273, 103.2454939717370905 ) ) ;
#7886 = DIRECTION ( 'NONE',  ( 0.000000000000000000, 0.000000000000000000, 1.000000000000000000 ) ) ;
#7887 =( GEOMETRIC_REPRESENTATION_CONTEXT ( 3 ) GLOBAL_UNCERTAINTY_ASSIGNED_CONTEXT ( ( #29032 ) ) GLOBAL_UNIT_ASSIGNED_CONTEXT ( ( #12352, #5985, #38498 ) ) REPRESENTATION_CONTEXT ( 'NONE', 'WORKASPACE' ) );
#7888 = VERTEX_POINT ( 'NONE', #5850 ) ;
#7889 = CARTESIAN_POINT ( 'NONE',  ( -27.97094176822542977, 40.00000000000000000, 9.504947828999611659 ) ) ;
#7890 = ORIENTED_EDGE ( 'NONE', *, *, #39115, .F. ) ;
#7891 = CARTESIAN_POINT ( 'NONE',  ( 18.00000000000000355, -8.053585752061598768, -46.81126742072031988 ) ) ;
#7892 = AXIS2_PLACEMENT_3D ( 'NONE', #38084, #4264, #14127 ) ;
#7893 = FACE_OUTER_BOUND ( 'NONE', #24021, .T. ) ;
#7894 = EDGE_CURVE ( 'NONE', #21438, #33305, #17530, .T. ) ;
#7895 = ORIENTED_EDGE ( 'NONE', *, *, #33455, .F. ) ;
#7896 = ADVANCED_FACE ( 'NONE', ( #22483, #25752 ), #9335, .T. ) ;
#7897 = PLANE ( 'NONE',  #40268 ) ;
#7898 = EDGE_CURVE ( 'NONE', #6403, #36912, #9129, .T. ) ;
#7899 = EDGE_CURVE ( 'NONE', #714, #2641, #28796, .T. ) ;
#7900 = EDGE_CURVE ( 'NONE', #30670, #23378, #25868, .T. ) ;
#7901 = DIRECTION ( 'NONE',  ( 0.000000000000000000, -0.9968120070307509017, 0.07978610555307326380 ) ) ;
#7902 = ORIENTED_EDGE ( 'NONE', *, *, #36421, .F. ) ;
#7903 = CARTESIAN_POINT ( 'NONE',  ( 0.000000000000000000, 111.7974656912330005, 9.465682155095883843 ) ) ;
#7904 = EDGE_LOOP ( 'NONE', ( #35000, #7624, #13097, #16086 ) ) ;
#7905 = ORIENTED_EDGE ( 'NONE', *, *, #6810, .T. ) ;
#7906 = CARTESIAN_POINT ( 'NONE',  ( -91.96080130434580724, -35.35525454449571470, 14.45886780445738218 ) ) ;
#7907 = CARTESIAN_POINT ( 'NONE',  ( -48.39074809477736494, 31.00000000000000355, -55.33250407651094349 ) ) ;
#7908 = AXIS2_PLACEMENT_3D ( 'NONE', #29094, #22149, #16213 ) ;
#7909 = EDGE_LOOP ( 'NONE', ( #26389, #30001, #8771, #2701 ) ) ;
#7910 = DIRECTION ( 'NONE',  ( 0.000000000000000000, 0.000000000000000000, -1.000000000000000000 ) ) ;
#7911 = CIRCLE ( 'NONE', #208, 116.0000000000000000 ) ;
#7912 = DIRECTION ( 'NONE',  ( 0.000000000000000000, -0.5963673585384915432, -0.8027116379309710004 ) ) ;
#7913 = EDGE_LOOP ( 'NONE', ( #41299, #30596, #33138, #853 ) ) ;
#7914 = DIRECTION ( 'NONE',  ( 0.000000000000000000, 0.000000000000000000, 1.000000000000000000 ) ) ;
#7915 = ORIENTED_EDGE ( 'NONE', *, *, #2030, .T. ) ;
#7916 = AXIS2_PLACEMENT_3D ( 'NONE', #42326, #32518, #12259 ) ;
#7917 = CARTESIAN_POINT ( 'NONE',  ( -80.50242771303932443, 40.00000000000000711, -46.62292012066232871 ) ) ;
#7919 = LINE ( 'NONE', #21281, #11685 ) ;
#7918 = LINE ( 'NONE', #25195, #20391 ) ;
#7920 = CARTESIAN_POINT ( 'NONE',  ( 18.00000000000000355, 0.000000000000000000, 0.000000000000000000 ) ) ;
#7921 = CARTESIAN_POINT ( 'NONE',  ( 0.000000000000000000, 11.41303419184972689, 111.6154788735836405 ) ) ;
#7922 = VERTEX_POINT ( 'NONE', #32688 ) ;
#7923 = ADVANCED_FACE ( 'NONE', ( #29431, #26156, #25539 ), #39431, .T. ) ;
#7924 = VECTOR ( 'NONE', #10119, 1000.000000000000000 ) ;
#7925 = ORIENTED_EDGE ( 'NONE', *, *, #39381, .T. ) ;
#7926 = DIRECTION ( 'NONE',  ( 0.000000000000000000, 0.000000000000000000, -1.000000000000000000 ) ) ;
#7927 = CARTESIAN_POINT ( 'NONE',  ( -78.83182461418512332, 31.00000000000000711, -45.51551753872077910 ) ) ;
#7928 = EDGE_CURVE ( 'NONE', #43048, #35650, #39049, .T. ) ;
#7929 = DIRECTION ( 'NONE',  ( 1.000000000000000000, 0.000000000000000000, 0.000000000000000000 ) ) ;
#7930 = ORIENTED_EDGE ( 'NONE', *, *, #30038, .F. ) ;
#7931 = CARTESIAN_POINT ( 'NONE',  ( -28.12618851199097492, 40.00000000000000000, 13.81902982503211064 ) ) ;
#7932 = ORIENTED_EDGE ( 'NONE', *, *, #19309, .T. ) ;
#7933 = ORIENTED_EDGE ( 'NONE', *, *, #23388, .T. ) ;
#7934 = CARTESIAN_POINT ( 'NONE',  ( 6.075999999999997847, 0.000000000000000000, 0.000000000000000000 ) ) ;
#7935 = DIRECTION ( 'NONE',  ( 0.000000000000000000, 0.000000000000000000, 1.000000000000000000 ) ) ;
#7936 = CIRCLE ( 'NONE', #39269, 58.99999999999998579 ) ;
#7937 = CARTESIAN_POINT ( 'NONE',  ( 18.00000000000000355, 32.00046193115198179, -34.40241257139653186 ) ) ;
#7938 = AXIS2_PLACEMENT_3D ( 'NONE', #31203, #15069, #14637 ) ;
#7939 = VERTEX_POINT ( 'NONE', #6486 ) ;
#7940 = CARTESIAN_POINT ( 'NONE',  ( 18.00000000000000355, 42.41764978026606769, 20.20639853260304619 ) ) ;
#7941 = ORIENTED_EDGE ( 'NONE', *, *, #19172, .T. ) ;
#7942 = CARTESIAN_POINT ( 'NONE',  ( -45.51113419504475388, -12.05525454449572109, 56.57887602028989704 ) ) ;
#7943 = DIRECTION ( 'NONE',  ( 0.000000000000000000, 0.000000000000000000, 1.000000000000000000 ) ) ;
#7944 = EDGE_CURVE ( 'NONE', #19546, #30887, #19843, .T. ) ;
#7945 = DIRECTION ( 'NONE',  ( 0.000000000000000000, 0.000000000000000000, 1.000000000000000000 ) ) ;
#7946 = EDGE_CURVE ( 'NONE', #29277, #21041, #40063, .T. ) ;
#7947 = EDGE_CURVE ( 'NONE', #29982, #27564, #6326, .T. ) ;
#7948 = CARTESIAN_POINT ( 'NONE',  ( 0.000000000000000000, 0.000000000000000000, 0.000000000000000000 ) ) ;
#7949 = ORIENTED_EDGE ( 'NONE', *, *, #23633, .F. ) ;
#7950 = VERTEX_POINT ( 'NONE', #795 ) ;
#7951 = CARTESIAN_POINT ( 'NONE',  ( -91.96080130434580724, -12.05525454449571043, 14.45886780445738218 ) ) ;
#7952 = DIRECTION ( 'NONE',  ( -1.000000000000000000, -0.000000000000000000, -0.000000000000000000 ) ) ;
#7953 = DIRECTION ( 'NONE',  ( 0.000000000000000000, 0.000000000000000000, -1.000000000000000000 ) ) ;
#7954 = ADVANCED_FACE ( 'NONE', ( #9980 ), #37241, .F. ) ;
#7955 = AXIS2_PLACEMENT_3D ( 'NONE', #19767, #33031, #3117 ) ;
#7956 = VERTEX_POINT ( 'NONE', #37029 ) ;
#7958 = VERTEX_POINT ( 'NONE', #7137 ) ;
#7957 = LINE ( 'NONE', #8597, #42418 ) ;
#7959 = CARTESIAN_POINT ( 'NONE',  ( 45.11287655886648906, 31.00000000000000355, -12.00022417491544324 ) ) ;
#7960 = DIRECTION ( 'NONE',  ( 0.000000000000000000, 0.1253332335643045359, -0.9921147013144778759 ) ) ;
#7961 = EDGE_CURVE ( 'NONE', #15394, #30264, #41867, .T. ) ;
#7963 = CARTESIAN_POINT ( 'NONE',  ( 42.80287614962790599, -35.35525454449572180, 69.29271901957253021 ) ) ;
#7962 = DIRECTION ( 'NONE',  ( -1.000000000000000000, -0.000000000000000000, -0.000000000000000000 ) ) ;
#7964 = AXIS2_PLACEMENT_3D ( 'NONE', #24929, #2353, #28396 ) ;
#7965 = ORIENTED_EDGE ( 'NONE', *, *, #361, .F. ) ;
#7966 = DIRECTION ( 'NONE',  ( 0.000000000000000000, 0.000000000000000000, 1.000000000000000000 ) ) ;
#7967 = CARTESIAN_POINT ( 'NONE',  ( -8.314562429032193336, 40.00000000000000000, -63.88718494337742015 ) ) ;
#7968 = AXIS2_PLACEMENT_3D ( 'NONE', #3359, #20004, #20219 ) ;
#7969 = CARTESIAN_POINT ( 'NONE',  ( 0.000000000000000000, 42.03146605346817921, -22.12489237027272893 ) ) ;
#7970 = CIRCLE ( 'NONE', #39990, 116.0000000000000000 ) ;
#7971 = CARTESIAN_POINT ( 'NONE',  ( 17.99999999999999645, -0.5156212287272186057, -112.1962860721878172 ) ) ;
#7972 = VERTEX_POINT ( 'NONE', #39855 ) ;
#7973 = DIRECTION ( 'NONE',  ( -1.000000000000000000, -0.000000000000000000, -0.000000000000000000 ) ) ;
#7974 = ORIENTED_EDGE ( 'NONE', *, *, #14856, .F. ) ;
#7975 = FILL_AREA_STYLE ('',( #6735 ) ) ;
#7976 = AXIS2_PLACEMENT_3D ( 'NONE', #28745, #9510, #35260 ) ;
#7977 = CYLINDRICAL_SURFACE ( 'NONE', #13481, 2.649999999999979039 ) ;
#7978 = DIRECTION ( 'NONE',  ( 0.000000000000000000, 0.000000000000000000, 1.000000000000000000 ) ) ;
#7979 = CARTESIAN_POINT ( 'NONE',  ( -46.07128526072433772, 31.00000000000000355, -40.40198152342698990 ) ) ;
#7980 = CARTESIAN_POINT ( 'NONE',  ( -10.00000000000000000, 0.000000000000000000, 0.000000000000000000 ) ) ;
#7981 = ORIENTED_EDGE ( 'NONE', *, *, #29534, .T. ) ;
#7982 = AXIS2_PLACEMENT_3D ( 'NONE', #2693, #16266, #30003 ) ;
#7983 = DIRECTION ( 'NONE',  ( 0.000000000000000000, 0.000000000000000000, -1.000000000000000000 ) ) ;
#7984 = ORIENTED_EDGE ( 'NONE', *, *, #39941, .T. ) ;
#7985 = CARTESIAN_POINT ( 'NONE',  ( -1.799870782497340782, 40.00000000000000000, 27.60416666422008802 ) ) ;
#7986 = EDGE_LOOP ( 'NONE', ( #36624, #28370, #41271, #20052 ) ) ;
#7987 = CYLINDRICAL_SURFACE ( 'NONE', #15209, 10.99999999999998934 ) ;
#7988 = DIRECTION ( 'NONE',  ( 0.000000000000000000, 0.5528000653611888637, 0.8333139190825179510 ) ) ;
#7989 = CARTESIAN_POINT ( 'NONE',  ( 11.20008397362390618, 31.00000000000000355, -84.14439686172904942 ) ) ;
#7990 = CARTESIAN_POINT ( 'NONE',  ( -10.92011822083620309, 40.00000000000000000, -83.75917815547794021 ) ) ;
#7991 = CARTESIAN_POINT ( 'NONE',  ( 0.000000000000000000, -31.94619804602776725, 16.59639811537345366 ) ) ;
#7992 = CIRCLE ( 'NONE', #32379, 20.00000000000000711 ) ;
#7993 = ORIENTED_EDGE ( 'NONE', *, *, #35383, .T. ) ;
#7994 = CARTESIAN_POINT ( 'NONE',  ( 0.000000000000000000, 120.4984140710909344, -0.7894348306988346886 ) ) ;
#7995 = VERTEX_POINT ( 'NONE', #33980 ) ;
#7996 = CARTESIAN_POINT ( 'NONE',  ( 0.000000000000000000, -31.48608500567869584, -0.9019157472707834966 ) ) ;
#7997 = AXIS2_PLACEMENT_3D ( 'NONE', #26039, #2229, #25640 ) ;
#7998 = DIRECTION ( 'NONE',  ( -0.000000000000000000, -0.000000000000000000, 1.000000000000000000 ) ) ;
#7999 = VECTOR ( 'NONE', #38507, 1000.000000000000000 ) ;
#8001 = VERTEX_POINT ( 'NONE', #40716 ) ;
#8000 = DIRECTION ( 'NONE',  ( -1.000000000000000000, 0.000000000000000000, 0.000000000000000000 ) ) ;
#8002 = ADVANCED_FACE ( 'NONE', ( #36586 ), #36815, .T. ) ;
#8003 = CARTESIAN_POINT ( 'NONE',  ( 0.000000000000000000, -57.40245293794732362, 96.40140491896615060 ) ) ;
#8004 = ORIENTED_EDGE ( 'NONE', *, *, #37912, .T. ) ;
#8005 = CARTESIAN_POINT ( 'NONE',  ( 1.411581201560190495E-15, 4.862606272033091592, -3.745885042887436622 ) ) ;
#8006 = CIRCLE ( 'NONE', #6585, 52.00000000000000000 ) ;
#8007 = CARTESIAN_POINT ( 'NONE',  ( 94.59594211465898184, 39.99999999999999289, 12.45590092308117569 ) ) ;
#8008 = DIRECTION ( 'NONE',  ( -0.9247238835424298475, -2.016449031586420221E-16, -0.3806385939525924744 ) ) ;
#8009 = ORIENTED_EDGE ( 'NONE', *, *, #6081, .T. ) ;
#8010 = DIRECTION ( 'NONE',  ( -1.000000000000000000, -0.000000000000000000, -0.000000000000000000 ) ) ;
#8011 = CARTESIAN_POINT ( 'NONE',  ( -105.9879088449591933, 17.11489954122026447, -0.3807199291576673361 ) ) ;
#8012 = ADVANCED_FACE ( 'NONE', ( #17225 ), #16578, .F. ) ;
#8013 = CIRCLE ( 'NONE', #15705, 59.00000000000001421 ) ;
#8015 = DIRECTION ( 'NONE',  ( 0.000000000000000000, -0.9213119778704166318, 0.3888241754733122724 ) ) ;
#8014 = DIRECTION ( 'NONE',  ( -1.000000000000000000, -0.000000000000000000, -0.000000000000000000 ) ) ;
#8016 = VERTEX_POINT ( 'NONE', #138 ) ;
#8017 = CYLINDRICAL_SURFACE ( 'NONE', #1697, 13.59999999999999964 ) ;
#8018 = ORIENTED_EDGE ( 'NONE', *, *, #32064, .T. ) ;
#8019 = CARTESIAN_POINT ( 'NONE',  ( 17.99999999999999645, 0.000000000000000000, 0.000000000000000000 ) ) ;
#8020 = CARTESIAN_POINT ( 'NONE',  ( -28.12618851199097492, 40.00000000000000000, 13.81902982503211064 ) ) ;
#8021 = CARTESIAN_POINT ( 'NONE',  ( 0.000000000000000000, -32.00046193115124282, -34.40241257139720688 ) ) ;
#8022 = ADVANCED_FACE ( 'NONE', ( #13500 ), #14152, .F. ) ;
#8023 = CARTESIAN_POINT ( 'NONE',  ( 17.99999999999999645, -31.80866420683992857, 16.59709355804118402 ) ) ;
#8024 = AXIS2_PLACEMENT_3D ( 'NONE', #10049, #6138, #6346 ) ;
#8025 = CARTESIAN_POINT ( 'NONE',  ( 17.99999999999999645, -6.486220790507708500, -112.0098273076987994 ) ) ;
#8027 = ORIENTED_EDGE ( 'NONE', *, *, #32960, .F. ) ;
#8026 = AXIS2_PLACEMENT_3D ( 'NONE', #22548, #15992, #36014 ) ;
#8029 = FACE_OUTER_BOUND ( 'NONE', #4233, .T. ) ;
#8028 = CARTESIAN_POINT ( 'NONE',  ( 17.99999999999999645, 0.000000000000000000, 0.000000000000000000 ) ) ;
#8030 = ORIENTED_EDGE ( 'NONE', *, *, #9227, .T. ) ;
#8031 = CIRCLE ( 'NONE', #11541, 116.0000000000000000 ) ;
#8032 = CARTESIAN_POINT ( 'NONE',  ( 0.000000000000000000, 24.22031524826126514, -109.5520369638034879 ) ) ;
#8033 = CARTESIAN_POINT ( 'NONE',  ( 17.99999999999999645, 31.48608500567870294, -0.9019157472705674472 ) ) ;
#8034 = CARTESIAN_POINT ( 'NONE',  ( -2.127120017302697619, 31.00000000000000355, -32.39583333539214038 ) ) ;
#8035 = ORIENTED_EDGE ( 'NONE', *, *, #37553, .T. ) ;
#8036 = CARTESIAN_POINT ( 'NONE',  ( 0.000000000000000000, 0.000000000000000000, 0.000000000000000000 ) ) ;
#8037 = AXIS2_PLACEMENT_3D ( 'NONE', #41744, #18041, #31512 ) ;
#8038 = CARTESIAN_POINT ( 'NONE',  ( 17.99999999999999645, -31.81777574834303124, -2.898764365605651427 ) ) ;
#8040 = AXIS2_PLACEMENT_3D ( 'NONE', #2666, #38689, #16030 ) ;
#8039 = CARTESIAN_POINT ( 'NONE',  ( 0.000000000000000000, 15.49408907645171674, 44.90087086784597403 ) ) ;
#8041 = CARTESIAN_POINT ( 'NONE',  ( 81.87674480462379734, 31.00000000000000000, -21.93767060400471891 ) ) ;
#8042 = ORIENTED_EDGE ( 'NONE', *, *, #28981, .F. ) ;
#8043 = CARTESIAN_POINT ( 'NONE',  ( -13.93478910046839125, 31.00000000000000355, -52.37520058406987999 ) ) ;
#8044 = CARTESIAN_POINT ( 'NONE',  ( -89.89583333403318477, 40.00000000000000711, 5.890486217120591839 ) ) ;
#8045 = EDGE_LOOP ( 'NONE', ( #42682, #18932, #21792, #5748 ) ) ;
#8046 = DIRECTION ( 'NONE',  ( 0.000000000000000000, 0.9980267284282713369, 0.06279051952931692659 ) ) ;
#8047 = DIRECTION ( 'NONE',  ( 0.000000000000000000, 0.000000000000000000, 1.000000000000000000 ) ) ;
#8048 = DIRECTION ( 'NONE',  ( 0.000000000000000000, 0.9213119778704139673, -0.3888241754733183231 ) ) ;
#8050 = ORIENTED_EDGE ( 'NONE', *, *, #4248, .T. ) ;
#8049 = DIRECTION ( 'NONE',  ( -1.000000000000000000, 0.000000000000000000, 0.000000000000000000 ) ) ;
#8051 = EDGE_CURVE ( 'NONE', #11670, #32336, #22394, .T. ) ;
#8052 = CARTESIAN_POINT ( 'NONE',  ( 0.000000000000000000, -114.6488492393081913, 37.09625815499973100 ) ) ;
#8053 = VECTOR ( 'NONE', #7643, 1000.000000000000000 ) ;
#8054 = DIRECTION ( 'NONE',  ( 0.000000000000000000, 0.000000000000000000, 1.000000000000000000 ) ) ;
#8055 = EDGE_CURVE ( 'NONE', #2747, #32585, #9110, .T. ) ;
#8056 = AXIS2_PLACEMENT_3D ( 'NONE', #24720, #27115, #37554 ) ;
#8057 = ORIENTED_EDGE ( 'NONE', *, *, #17258, .F. ) ;
#8058 = CARTESIAN_POINT ( 'NONE',  ( 20.30000058474805869, 40.00000000000000000, -59.80472289869057789 ) ) ;
#8059 = FACE_OUTER_BOUND ( 'NONE', #19741, .T. ) ;
#8060 = CIRCLE ( 'NONE', #38697, 13.60000000000000142 ) ;
#8061 = ORIENTED_EDGE ( 'NONE', *, *, #27032, .T. ) ;
#8062 = VECTOR ( 'NONE', #1210, 1000.000000000000000 ) ;
#8063 = CARTESIAN_POINT ( 'NONE',  ( -109.0695705685749317, 106.4195705685765603, 7.000000000000336620 ) ) ;
#8064 = DIRECTION ( 'NONE',  ( 0.000000000000000000, 0.000000000000000000, 1.000000000000000000 ) ) ;
#8065 = AXIS2_PLACEMENT_3D ( 'NONE', #23802, #37711, #24243 ) ;
#8066 = AXIS2_PLACEMENT_3D ( 'NONE', #18068, #27853, #23778 ) ;
#8067 = ORIENTED_EDGE ( 'NONE', *, *, #14413, .T. ) ;
#8068 = DIRECTION ( 'NONE',  ( 1.000000000000000000, 0.000000000000000000, 0.000000000000000000 ) ) ;
#8069 = ORIENTED_EDGE ( 'NONE', *, *, #27597, .F. ) ;
#8070 = EDGE_CURVE ( 'NONE', #37442, #25462, #37820, .T. ) ;
#8071 = AXIS2_PLACEMENT_3D ( 'NONE', #16136, #11628, #21900 ) ;
#8072 = DIRECTION ( 'NONE',  ( 1.000000000000000000, 0.000000000000000000, 0.000000000000000000 ) ) ;
#8073 = ORIENTED_EDGE ( 'NONE', *, *, #40077, .F. ) ;
#8074 = DIRECTION ( 'NONE',  ( 0.000000000000000000, 0.5877852522924685852, 0.8090169943749507819 ) ) ;
#8075 = CARTESIAN_POINT ( 'NONE',  ( -50.38378093998269946, 31.00000000000000711, 87.00968337440518496 ) ) ;
#8076 = EDGE_CURVE ( 'NONE', #36459, #18380, #3840, .T. ) ;
#8077 = ORIENTED_EDGE ( 'NONE', *, *, #42674, .F. ) ;
#8078 = DIRECTION ( 'NONE',  ( -1.000000000000000000, 0.000000000000000000, 0.000000000000000000 ) ) ;
#8079 = CYLINDRICAL_SURFACE ( 'NONE', #3849, 116.0000000000000000 ) ;
#8080 = VERTEX_POINT ( 'NONE', #13289 ) ;
#8081 = PLANE ( 'NONE',  #5024 ) ;
#8082 = DIRECTION ( 'NONE',  ( 0.000000000000000000, 0.9826841245925203028, 0.1852887240871181618 ) ) ;
#8083 = VERTEX_POINT ( 'NONE', #20280 ) ;
#8084 = DIRECTION ( 'NONE',  ( -0.000000000000000000, -0.000000000000000000, -1.000000000000000000 ) ) ;
#8085 = DIRECTION ( 'NONE',  ( -1.000000000000000000, 0.000000000000000000, 0.000000000000000000 ) ) ;
#8086 = CIRCLE ( 'NONE', #37322, 59.00000000000000711 ) ;
#8087 = VERTEX_POINT ( 'NONE', #30513 ) ;
#8088 = ADVANCED_FACE ( 'NONE', ( #585 ), #4231, .T. ) ;
#8089 = CIRCLE ( 'NONE', #19966, 116.0000000000000000 ) ;
#8090 = CARTESIAN_POINT ( 'NONE',  ( 106.4195705685763471, -106.4195705685744855, 10.00000000000000000 ) ) ;
#8091 = CARTESIAN_POINT ( 'NONE',  ( -38.53741714288415210, 31.00000000000000355, -33.79371401777069650 ) ) ;
#8092 = EDGE_CURVE ( 'NONE', #1587, #27890, #33489, .T. ) ;
#8093 = ORIENTED_EDGE ( 'NONE', *, *, #10290, .T. ) ;
#8094 = AXIS2_PLACEMENT_3D ( 'NONE', #11874, #11656, #24999 ) ;
#8096 = DIRECTION ( 'NONE',  ( 0.000000000000000000, -0.9996456111234522934, -0.02662052143778445915 ) ) ;
#8095 = DIRECTION ( 'NONE',  ( 0.000000000000000000, 0.000000000000000000, 1.000000000000000000 ) ) ;
#8097 = ADVANCED_FACE ( 'NONE', ( #11090 ), #38109, .F. ) ;
#8098 = FACE_OUTER_BOUND ( 'NONE', #42977, .T. ) ;
#8099 = ORIENTED_EDGE ( 'NONE', *, *, #35616, .T. ) ;
#8100 = CIRCLE ( 'NONE', #12291, 116.0000000000000000 ) ;
#8101 = AXIS2_PLACEMENT_3D ( 'NONE', #23837, #37101, #14219 ) ;
#8102 = CARTESIAN_POINT ( 'NONE',  ( 0.000000000000000000, -22.43957647427129842, -41.27978878573651400 ) ) ;
#8103 = CARTESIAN_POINT ( 'NONE',  ( -29.22812062908682051, 40.00000000000000000, 50.62729764625685647 ) ) ;
#8104 = CARTESIAN_POINT ( 'NONE',  ( -58.36801134196149832, 40.00000000000000711, 19.71467013091580256 ) ) ;
#8105 = CIRCLE ( 'NONE', #13699, 120.5010000000000332 ) ;
#8106 = CARTESIAN_POINT ( 'NONE',  ( 9.000000000000001776, 98.69720329641039314, -60.94966826379810243 ) ) ;
#8107 = DIRECTION ( 'NONE',  ( -1.000000000000000000, 0.000000000000000000, 0.000000000000000000 ) ) ;
#8108 = DIRECTION ( 'NONE',  ( -1.000000000000000000, 0.000000000000000000, -0.000000000000000000 ) ) ;
#8109 = CARTESIAN_POINT ( 'NONE',  ( -10.86393331615775892, 31.00000000000000355, -18.79923026442779843 ) ) ;
#8110 = EDGE_CURVE ( 'NONE', #33918, #17817, #21028, .T. ) ;
#8111 = VERTEX_POINT ( 'NONE', #34839 ) ;
#8112 = CARTESIAN_POINT ( 'NONE',  ( 34.98270738856093232, 40.00000000000000000, 4.602016392115340970 ) ) ;
#8113 = ORIENTED_EDGE ( 'NONE', *, *, #31886, .F. ) ;
#8114 = DIRECTION ( 'NONE',  ( -1.000000000000000000, 0.000000000000000000, 0.000000000000000000 ) ) ;
#8115 = CYLINDRICAL_SURFACE ( 'NONE', #8914, 16.00000000000023448 ) ;
#8116 = ORIENTED_EDGE ( 'NONE', *, *, #5624, .F. ) ;
#8117 = VECTOR ( 'NONE', #4866, 1000.000000000000000 ) ;
#8118 = CARTESIAN_POINT ( 'NONE',  ( -10.00000000000000178, 0.000000000000000000, 0.000000000000000000 ) ) ;
#8119 = DIRECTION ( 'NONE',  ( 1.000000000000000000, 0.000000000000000000, 0.000000000000000000 ) ) ;
#8120 = ORIENTED_EDGE ( 'NONE', *, *, #11107, .T. ) ;
#8121 = CARTESIAN_POINT ( 'NONE',  ( 17.99999999999999645, 27.24480646643629811, -15.80846360676556372 ) ) ;
#8122 = CIRCLE ( 'NONE', #12313, 47.49900000000000233 ) ;
#8123 = ORIENTED_EDGE ( 'NONE', *, *, #31324, .T. ) ;
#8124 = VECTOR ( 'NONE', #20246, 1000.000000000000000 ) ;
#8125 = CIRCLE ( 'NONE', #22092, 5.384454397937118664 ) ;
#8126 = EDGE_CURVE ( 'NONE', #20431, #1556, #42532, .T. ) ;
#8127 = ORIENTED_EDGE ( 'NONE', *, *, #31027, .T. ) ;
#8128 = AXIS2_PLACEMENT_3D ( 'NONE', #31021, #3715, #20166 ) ;
#8129 = CARTESIAN_POINT ( 'NONE',  ( -6.075999999999997847, 0.000000000000000000, 0.000000000000000000 ) ) ;
#8130 = CARTESIAN_POINT ( 'NONE',  ( -46.76215110878947456, 31.00000000000000355, 53.15211786535368788 ) ) ;
#8131 = EDGE_CURVE ( 'NONE', #12660, #14763, #40944, .T. ) ;
#8132 = ORIENTED_EDGE ( 'NONE', *, *, #30375, .F. ) ;
#8133 = CIRCLE ( 'NONE', #1140, 59.00000000000000000 ) ;
#8134 = EDGE_CURVE ( 'NONE', #8627, #2879, #23781, .T. ) ;
#8135 = CARTESIAN_POINT ( 'NONE',  ( 0.000000000000000000, 18.35539002514530793, -110.6858262410707994 ) ) ;
#8136 = ORIENTED_EDGE ( 'NONE', *, *, #42928, .F. ) ;
#8137 = FACE_OUTER_BOUND ( 'NONE', #2110, .T. ) ;
#8138 = AXIS2_PLACEMENT_3D ( 'NONE', #39870, #19646, #32912 ) ;
#8139 = VERTEX_POINT ( 'NONE', #30925 ) ;
#8140 = CARTESIAN_POINT ( 'NONE',  ( 97.09201668843398636, 39.99999999999999289, 6.474068422258194566 ) ) ;
#8141 = AXIS2_PLACEMENT_3D ( 'NONE', #37845, #21767, #25045 ) ;
#8142 = CARTESIAN_POINT ( 'NONE',  ( -3.169834189307652927, 31.00000000000000355, -24.13593742708953016 ) ) ;
#8144 = DIRECTION ( 'NONE',  ( -1.000000000000000000, 0.000000000000000000, -0.000000000000000000 ) ) ;
#8143 = DIRECTION ( 'NONE',  ( 0.000000000000000000, -0.9213119778704086382, -0.3888241754733307021 ) ) ;
#8145 = DIRECTION ( 'NONE',  ( -1.000000000000000000, 0.000000000000000000, 0.000000000000000000 ) ) ;
#8146 = FACE_OUTER_BOUND ( 'NONE', #40371, .T. ) ;
#8147 = ORIENTED_EDGE ( 'NONE', *, *, #22989, .T. ) ;
#8148 = SURFACE_STYLE_USAGE ( .BOTH. , #11433 ) ;
#8149 = DIRECTION ( 'NONE',  ( -1.000000000000000000, 0.000000000000000000, 0.000000000000000000 ) ) ;
#8150 = ORIENTED_EDGE ( 'NONE', *, *, #37855, .F. ) ;
#8151 = DIRECTION ( 'NONE',  ( 0.000000000000000000, 0.1590634960190723812, -0.9872683547213445543 ) ) ;
#8152 = CARTESIAN_POINT ( 'NONE',  ( 89.65113856817994531, 31.00000000000000000, -30.44896562292877462 ) ) ;
#8153 = EDGE_CURVE ( 'NONE', #26461, #32652, #4941, .T. ) ;
#8154 = CARTESIAN_POINT ( 'NONE',  ( 17.99999999999999645, 53.40478689619730090, 108.0204598100367548 ) ) ;
#8155 = AXIS2_PLACEMENT_3D ( 'NONE', #18097, #14796, #28098 ) ;
#8156 = ORIENTED_EDGE ( 'NONE', *, *, #8683, .F. ) ;
#8157 = PRODUCT_DEFINITION ( 'UNKNOWN', '', #36488, #32497 ) ;
#8158 = AXIS2_PLACEMENT_3D ( 'NONE', #34125, #34776, #27598 ) ;
#8159 = CARTESIAN_POINT ( 'NONE',  ( -15.23573235977941032, 40.00000000000000000, 26.30445775087293114 ) ) ;
#8160 = CIRCLE ( 'NONE', #40866, 116.0000000000000000 ) ;
#8161 = ORIENTED_EDGE ( 'NONE', *, *, #22771, .F. ) ;
#8162 = AXIS2_PLACEMENT_3D ( 'NONE', #29819, #25906, #6655 ) ;
#8163 = ORIENTED_EDGE ( 'NONE', *, *, #25337, .F. ) ;
#8164 = CARTESIAN_POINT ( 'NONE',  ( 18.00000000000000355, -47.00885577955416039, 6.806061952192135500 ) ) ;
#8165 = CARTESIAN_POINT ( 'NONE',  ( 11.90854556226686789, -34.05525454449573175, -74.83297477053821467 ) ) ;
#8166 = DIRECTION ( 'NONE',  ( 0.000000000000000000, 0.000000000000000000, -1.000000000000000000 ) ) ;
#8167 = VECTOR ( 'NONE', #24360, 1000.000000000000000 ) ;
#8168 = CARTESIAN_POINT ( 'NONE',  ( 17.99999999999999645, -96.25468616236614139, -72.49500943364587613 ) ) ;
#8169 = EDGE_CURVE ( 'NONE', #28304, #42969, #15254, .T. ) ;
#8170 = VECTOR ( 'NONE', #29084, 1000.000000000000000 ) ;
#8171 = ORIENTED_EDGE ( 'NONE', *, *, #40677, .T. ) ;
#8172 = DIRECTION ( 'NONE',  ( 1.000000000000000000, 0.000000000000000000, 0.000000000000000000 ) ) ;
#8173 = EDGE_LOOP ( 'NONE', ( #7676, #13776, #19033, #38901 ) ) ;
#8174 = LINE ( 'NONE', #21534, #21575 ) ;
#8175 = DIRECTION ( 'NONE',  ( -1.000000000000000000, -0.000000000000000000, -0.000000000000000000 ) ) ;
#8176 = CARTESIAN_POINT ( 'NONE',  ( -0.2142857142857142738, -10.49781318335647917, 0.000000000000000000 ) ) ;
#8177 = CARTESIAN_POINT ( 'NONE',  ( 0.000000000000000000, 5.919241748379588053, 31.39643714728458690 ) ) ;
#8178 = VERTEX_POINT ( 'NONE', #18309 ) ;
#8179 = ORIENTED_EDGE ( 'NONE', *, *, #36594, .T. ) ;
#8180 = DIRECTION ( 'NONE',  ( -1.000000000000000000, 0.000000000000000000, 0.000000000000000000 ) ) ;
#8181 = CARTESIAN_POINT ( 'NONE',  ( 18.00000000000000355, -27.79676263918213763, 37.88001506494759241 ) ) ;
#8182 = EDGE_CURVE ( 'NONE', #1507, #34733, #16112, .T. ) ;
#8183 = VERTEX_POINT ( 'NONE', #7790 ) ;
#8185 = EDGE_LOOP ( 'NONE', ( #21416, #7316, #16335, #467, #4660 ) ) ;
#8184 = DIRECTION ( 'NONE',  ( -0.000000000000000000, -0.000000000000000000, -1.000000000000000000 ) ) ;
#8186 = CARTESIAN_POINT ( 'NONE',  ( 30.22238470471967631, 31.00000000000000355, -34.33595424619392844 ) ) ;
#8187 = EDGE_CURVE ( 'NONE', #42630, #2738, #40450, .T. ) ;
#8188 = DIRECTION ( 'NONE',  ( 1.000000000000000000, 0.000000000000000000, 0.000000000000000000 ) ) ;
#8189 = AXIS2_PLACEMENT_3D ( 'NONE', #25480, #35470, #36112 ) ;
#8190 = AXIS2_PLACEMENT_3D ( 'NONE', #13383, #19722, #29518 ) ;
#8192 = LINE ( 'NONE', #22547, #31702 ) ;
#8191 = DIRECTION ( 'NONE',  ( -1.000000000000000000, 0.000000000000000000, -0.000000000000000000 ) ) ;
#8193 = VERTEX_POINT ( 'NONE', #37882 ) ;
#8194 = FACE_OUTER_BOUND ( 'NONE', #36119, .T. ) ;
#8195 = CIRCLE ( 'NONE', #4728, 13.59999999999999964 ) ;
#8196 = CARTESIAN_POINT ( 'NONE',  ( -16.51797447735934199, 40.00000000000000000, -62.05742538352703974 ) ) ;
#8197 = CIRCLE ( 'NONE', #8877, 59.00000000000000000 ) ;
#8198 = CIRCLE ( 'NONE', #34662, 20.00000000000000711 ) ;
#8199 = EDGE_CURVE ( 'NONE', #9794, #20914, #27250, .T. ) ;
#8200 = CIRCLE ( 'NONE', #20130, 47.49900000000000944 ) ;
#8201 = CARTESIAN_POINT ( 'NONE',  ( 17.99999999999999645, -5.456439917444183330, -112.0647122740742390 ) ) ;
#8202 = DIRECTION ( 'NONE',  ( 0.000000000000000000, 0.000000000000000000, 1.000000000000000000 ) ) ;
#8203 = ORIENTED_EDGE ( 'NONE', *, *, #23450, .F. ) ;
#8204 = CARTESIAN_POINT ( 'NONE',  ( 0.000000000000000000, -30.78424799127072120, 6.672111855473074726 ) ) ;
#8205 = ORIENTED_EDGE ( 'NONE', *, *, #20565, .T. ) ;
#8206 = LINE ( 'NONE', #14331, #30878 ) ;
#8207 = DIRECTION ( 'NONE',  ( 0.000000000000000000, 0.000000000000000000, 1.000000000000000000 ) ) ;
#8208 = CIRCLE ( 'NONE', #38155, 36.00000000000000000 ) ;
#8209 = EDGE_CURVE ( 'NONE', #11655, #16140, #8235, .T. ) ;
#8210 = CARTESIAN_POINT ( 'NONE',  ( -9.469526743414824921, 31.00000000000000355, -71.82433816204535049 ) ) ;
#8211 = EDGE_CURVE ( 'NONE', #1657, #29146, #14446, .T. ) ;
#8212 = CARTESIAN_POINT ( 'NONE',  ( 17.99999999999999645, 0.000000000000000000, 0.000000000000000000 ) ) ;
#8213 = EDGE_LOOP ( 'NONE', ( #8385, #11994, #34419, #42980 ) ) ;
#8214 = EDGE_CURVE ( 'NONE', #39261, #35327, #27674, .T. ) ;
#8215 = ADVANCED_FACE ( 'NONE', ( #31366 ), #14588, .F. ) ;
#8216 = CARTESIAN_POINT ( 'NONE',  ( 0.000000000000000000, 0.000000000000000000, 0.000000000000000000 ) ) ;
#8217 = ORIENTED_EDGE ( 'NONE', *, *, #42164, .F. ) ;
#8218 = FACE_OUTER_BOUND ( 'NONE', #27298, .T. ) ;
#8219 = DIRECTION ( 'NONE',  ( 0.000000000000000000, 0.000000000000000000, 1.000000000000000000 ) ) ;
#8220 = CIRCLE ( 'NONE', #13094, 20.00000000000001066 ) ;
#8221 = CARTESIAN_POINT ( 'NONE',  ( -40.35386350238496789, 31.00000000000000355, 69.65762217234957632 ) ) ;
#8222 = CARTESIAN_POINT ( 'NONE',  ( 39.23423008407738877, 40.00000000000000000, 79.83814995801118641 ) ) ;
#8223 = CARTESIAN_POINT ( 'NONE',  ( 103.7695705685741387, 106.4195705685767166, 9.999999999999998224 ) ) ;
#8224 = ORIENTED_EDGE ( 'NONE', *, *, #8397, .T. ) ;
#8225 = DIRECTION ( 'NONE',  ( -1.000000000000000000, 0.000000000000000000, 0.000000000000000000 ) ) ;
#8226 = ORIENTED_EDGE ( 'NONE', *, *, #10834, .T. ) ;
#8227 = VECTOR ( 'NONE', #7515, 1000.000000000000000 ) ;
#8228 = CARTESIAN_POINT ( 'NONE',  ( 0.000000000000000000, -120.4984140710909202, -0.7894348306996294973 ) ) ;
#8229 = DIRECTION ( 'NONE',  ( -1.000000000000000000, -0.000000000000000000, -0.000000000000000000 ) ) ;
#8230 = AXIS2_PLACEMENT_3D ( 'NONE', #37567, #21043, #18847 ) ;
#8232 = ORIENTED_EDGE ( 'NONE', *, *, #18023, .F. ) ;
#8231 = DIRECTION ( 'NONE',  ( -0.000000000000000000, -0.000000000000000000, 1.000000000000000000 ) ) ;
#8233 = DIRECTION ( 'NONE',  ( 0.000000000000000000, 0.3681245526846719240, 0.9297764858882537897 ) ) ;
#8234 = ORIENTED_EDGE ( 'NONE', *, *, #26069, .F. ) ;
#8235 = LINE ( 'NONE', #11750, #32805 ) ;
#8236 = CARTESIAN_POINT ( 'NONE',  ( 95.10416666600561086, 39.99999999999999289, 6.217735451873073416 ) ) ;
#8237 = DIRECTION ( 'NONE',  ( -2.249565377136137858E-32, 1.224646799147353207E-16, 1.000000000000000000 ) ) ;
#8238 = VERTEX_POINT ( 'NONE', #17876 ) ;
#8239 = CYLINDRICAL_SURFACE ( 'NONE', #17203, 47.49900000000000233 ) ;
#8240 = EDGE_CURVE ( 'NONE', #33247, #25006, #14800, .T. ) ;
#8241 = DIRECTION ( 'NONE',  ( -1.000000000000000000, 0.000000000000000000, 0.000000000000000000 ) ) ;
#8242 = AXIS2_PLACEMENT_3D ( 'NONE', #23889, #37376, #20198 ) ;
#8244 = DIRECTION ( 'NONE',  ( 1.000000000000000000, 0.000000000000000000, 0.000000000000000000 ) ) ;
#8243 = DIRECTION ( 'NONE',  ( 0.000000000000000000, 0.9968120070307504577, -0.07978610555307977248 ) ) ;
#8245 = VERTEX_POINT ( 'NONE', #41364 ) ;
#8246 = DIRECTION ( 'NONE',  ( 0.000000000000000000, 0.000000000000000000, 1.000000000000000000 ) ) ;
#8247 = ORIENTED_EDGE ( 'NONE', *, *, #8682, .F. ) ;
#8248 = CARTESIAN_POINT ( 'NONE',  ( 0.000000000000000000, 7.220349212960960550, -35.26849241522656087 ) ) ;
#8249 = CARTESIAN_POINT ( 'NONE',  ( -30.84436395684957333, 40.00000000000000000, -10.52363363425145337 ) ) ;
#8250 = CYLINDRICAL_SURFACE ( 'NONE', #6325, 13.60000000000000142 ) ;
#8251 = CIRCLE ( 'NONE', #27066, 116.0000000000000000 ) ;
#8252 = VECTOR ( 'NONE', #4121, 1000.000000000000000 ) ;
#8253 = CARTESIAN_POINT ( 'NONE',  ( 4.000000000000000000, 2.309401076758497151, -5.000000000000000000 ) ) ;
#8254 = DIRECTION ( 'NONE',  ( -1.000000000000000000, 0.000000000000000000, 0.000000000000000000 ) ) ;
#8255 = ORIENTED_EDGE ( 'NONE', *, *, #22136, .F. ) ;
#8256 = AXIS2_PLACEMENT_3D ( 'NONE', #32891, #2968, #6703 ) ;
#8257 = CARTESIAN_POINT ( 'NONE',  ( -10.00000000000000000, 0.000000000000000000, 0.000000000000000000 ) ) ;
#8258 = ORIENTED_EDGE ( 'NONE', *, *, #15006, .F. ) ;
#8259 = AXIS2_PLACEMENT_3D ( 'NONE', #41305, #11454, #16024 ) ;
#8260 = CYLINDRICAL_SURFACE ( 'NONE', #36394, 19.19999999999999574 ) ;
#8261 = CARTESIAN_POINT ( 'NONE',  ( 0.000000000000000000, -40.47821179127690527, -32.64221760512802462 ) ) ;
#8262 = CARTESIAN_POINT ( 'NONE',  ( -30.01493782828161017, 31.00000000000000355, -3.947526014606304035 ) ) ;
#8263 = ORIENTED_EDGE ( 'NONE', *, *, #35615, .T. ) ;
#8264 = CYLINDRICAL_SURFACE ( 'NONE', #32930, 23.00000000000000000 ) ;
#8265 = EDGE_CURVE ( 'NONE', #8333, #35102, #11979, .T. ) ;
#8266 = EDGE_CURVE ( 'NONE', #16946, #40970, #25707, .T. ) ;
#8267 = ITEM_DEFINED_TRANSFORMATION ( 'NONE', 'NONE', #19820,  #13552 ) ;
#8268 = EDGE_CURVE ( 'NONE', #18966, #16222, #22431, .T. ) ;
#8269 = CARTESIAN_POINT ( 'NONE',  ( 17.99999999999999645, -91.65951123222531294, 71.09524597798055368 ) ) ;
#8270 = CARTESIAN_POINT ( 'NONE',  ( 75.10416666583130052, 31.00000000000000000, 4.908738512847474311 ) ) ;
#8271 = ORIENTED_EDGE ( 'NONE', *, *, #9156, .F. ) ;
#8272 = CARTESIAN_POINT ( 'NONE',  ( -33.53193138075044999, 31.00000000000000355, 38.09769221459629307 ) ) ;
#8273 = CARTESIAN_POINT ( 'NONE',  ( -87.52616871875942195, 40.00000000000000711, -23.43677886868077209 ) ) ;
#8274 = ORIENTED_EDGE ( 'NONE', *, *, #4357, .F. ) ;
#8275 = CARTESIAN_POINT ( 'NONE',  ( 18.00000000000000355, 0.000000000000000000, 0.000000000000000000 ) ) ;
#8276 = EDGE_CURVE ( 'NONE', #1401, #3853, #42442, .T. ) ;
#8277 = FACE_OUTER_BOUND ( 'NONE', #40523, .T. ) ;
#8278 = DIRECTION ( 'NONE',  ( 1.000000000000000000, 0.000000000000000000, 0.000000000000000000 ) ) ;
#8279 = AXIS2_PLACEMENT_3D ( 'NONE', #10479, #16639, #39692 ) ;
#8281 = ORIENTED_EDGE ( 'NONE', *, *, #43094, .T. ) ;
#8280 = FACE_OUTER_BOUND ( 'NONE', #10413, .T. ) ;
#8282 = CARTESIAN_POINT ( 'NONE',  ( -10.00000000000000000, 0.000000000000000000, 0.000000000000000000 ) ) ;
#8283 = CARTESIAN_POINT ( 'NONE',  ( 17.99999999999999645, 8.827181066045881153, 120.1772519049559662 ) ) ;
#8284 = CIRCLE ( 'NONE', #31276, 130.0000000000013927 ) ;
#8285 = ORIENTED_EDGE ( 'NONE', *, *, #26316, .F. ) ;
#8286 = CARTESIAN_POINT ( 'NONE',  ( 42.05404839982585941, 40.00000000000000000, -47.95475229022623864 ) ) ;
#8287 = CARTESIAN_POINT ( 'NONE',  ( -10.00000000000000000, 0.000000000000000000, 0.000000000000000000 ) ) ;
#8288 = ORIENTED_EDGE ( 'NONE', *, *, #15660, .T. ) ;
#8289 = CARTESIAN_POINT ( 'NONE',  ( 17.99999999999999645, -59.07817985938929439, -105.0250430397515089 ) ) ;
#8290 = CARTESIAN_POINT ( 'NONE',  ( 17.99999999999999645, 5.919241748379588053, 31.39643714728458690 ) ) ;
#8291 = VERTEX_POINT ( 'NONE', #6231 ) ;
#8292 = CARTESIAN_POINT ( 'NONE',  ( 17.99999999999999645, 0.000000000000000000, 0.000000000000000000 ) ) ;
#8293 = ORIENTED_EDGE ( 'NONE', *, *, #8555, .T. ) ;
#8294 = DIRECTION ( 'NONE',  ( -1.000000000000000000, 0.000000000000000000, 0.000000000000000000 ) ) ;
#8295 = EDGE_LOOP ( 'NONE', ( #3872, #14424, #35773, #944 ) ) ;
#8296 = CARTESIAN_POINT ( 'NONE',  ( 17.99999999999999645, -75.72520367775034345, -82.78868281116056949 ) ) ;
#8297 = CARTESIAN_POINT ( 'NONE',  ( 0.000000000000000000, -0.6168405712484118508, -35.99471499692226928 ) ) ;
#8298 = DIRECTION ( 'NONE',  ( 0.000000000000000000, 0.000000000000000000, 1.000000000000000000 ) ) ;
#8299 = CARTESIAN_POINT ( 'NONE',  ( 0.000000000000000000, -21.55123232222555529, 118.5581519187671518 ) ) ;
#8300 = ORIENTED_EDGE ( 'NONE', *, *, #35134, .F. ) ;
#8301 = CYLINDRICAL_SURFACE ( 'NONE', #40535, 59.00000000000000000 ) ;
#8302 = CARTESIAN_POINT ( 'NONE',  ( 65.39325745242679488, -2.055254544495723756, 58.58409293616905700 ) ) ;
#8303 = CIRCLE ( 'NONE', #13901, 52.00000000000000000 ) ;
#8304 = ORIENTED_EDGE ( 'NONE', *, *, #28285, .T. ) ;
#8305 = AXIS2_PLACEMENT_3D ( 'NONE', #7358, #4071, #797 ) ;
#8306 = CARTESIAN_POINT ( 'NONE',  ( 17.99999999999999645, -79.94368240339484544, 90.16373242487880191 ) ) ;
#8307 = ADVANCED_FACE ( 'NONE', ( #36115, #22864, #25905, #35681, #19369, #42866, #38957, #15649, #19576, #12381 ), #5594, .T. ) ;
#8308 = DIRECTION ( 'NONE',  ( -1.000000000000000000, 0.000000000000000000, -0.000000000000000000 ) ) ;
#8309 = VECTOR ( 'NONE', #468, 1000.000000000000000 ) ;
#8310 = SHAPE_DEFINITION_REPRESENTATION ( #9548, #39082 ) ;
#8311 = DIRECTION ( 'NONE',  ( -1.000000000000000000, 0.000000000000000000, 0.000000000000000000 ) ) ;
#8312 = CARTESIAN_POINT ( 'NONE',  ( -21.36651465564686703, 31.00000000000000355, 43.35257367405362317 ) ) ;
#8313 = ORIENTED_EDGE ( 'NONE', *, *, #19639, .T. ) ;
#8315 = FACE_OUTER_BOUND ( 'NONE', #13898, .T. ) ;
#8314 = LINE ( 'NONE', #41023, #27497 ) ;
#8316 = ORIENTED_EDGE ( 'NONE', *, *, #41115, .F. ) ;
#8317 = EDGE_CURVE ( 'NONE', #6169, #14830, #6016, .T. ) ;
#8318 = CARTESIAN_POINT ( 'NONE',  ( 4.090615425948669781, 40.00000000000000000, -62.60416666561555132 ) ) ;
#8319 = CARTESIAN_POINT ( 'NONE',  ( 18.91139405008128804, 40.00000000000000000, 55.99505798892768382 ) ) ;
#8320 = EDGE_CURVE ( 'NONE', #17546, #37998, #17564, .T. ) ;
#8321 = DIRECTION ( 'NONE',  ( -1.000000000000000000, 0.000000000000000000, 0.000000000000000000 ) ) ;
#8322 = ADVANCED_FACE ( 'NONE', ( #12588 ), #5796, .F. ) ;
#8323 = DIRECTION ( 'NONE',  ( -1.000000000000000000, 0.000000000000000000, 0.000000000000000000 ) ) ;
#8324 = FACE_OUTER_BOUND ( 'NONE', #35954, .T. ) ;
#8325 = CARTESIAN_POINT ( 'NONE',  ( -7.088330391075835735, 31.00000000000000355, -20.85399598300688595 ) ) ;
#8326 = B_SPLINE_CURVE_WITH_KNOTS ( 'NONE', 3,
 ( #17686, #40323, #30955, #24448, #24007 ),
 .UNSPECIFIED., .F., .F.,
 ( 4, 1, 4 ),
 ( 0.000000000000000000, 0.002309401076758505790, 0.004618802153517011580 ),
 .UNSPECIFIED. ) ;
#8327 = EDGE_LOOP ( 'NONE', ( #20804, #26585, #13554, #42176 ) ) ;
#8328 = CARTESIAN_POINT ( 'NONE',  ( -30.01493782828161017, 40.00000000000000000, -3.947526014606304035 ) ) ;
#8329 = ORIENTED_EDGE ( 'NONE', *, *, #35389, .F. ) ;
#8330 = DIRECTION ( 'NONE',  ( 0.000000000000000000, 0.000000000000000000, 1.000000000000000000 ) ) ;
#8332 = DIRECTION ( 'NONE',  ( 0.000000000000000000, 0.000000000000000000, 1.000000000000000000 ) ) ;
#8331 = AXIS2_PLACEMENT_3D ( 'NONE', #13307, #2990, #29445 ) ;
#8333 = VERTEX_POINT ( 'NONE', #39596 ) ;
#8334 = CARTESIAN_POINT ( 'NONE',  ( 18.00000000000000355, 0.000000000000000000, 0.000000000000000000 ) ) ;
#8335 = CARTESIAN_POINT ( 'NONE',  ( -10.00000000000000178, 0.000000000000000000, -13.40000000000000036 ) ) ;
#8336 = ORIENTED_EDGE ( 'NONE', *, *, #35197, .F. ) ;
#8337 = CARTESIAN_POINT ( 'NONE',  ( 0.6666666666666689611, 4.233901974057261874, -3.300726591567082480 ) ) ;
#8338 = ORIENTED_EDGE ( 'NONE', *, *, #20951, .F. ) ;
#8339 = VECTOR ( 'NONE', #15547, 1000.000000000000000 ) ;
#8340 = EDGE_CURVE ( 'NONE', #7274, #39353, #32421, .T. ) ;
#8341 = ORIENTED_EDGE ( 'NONE', *, *, #28631, .T. ) ;
#8342 = CARTESIAN_POINT ( 'NONE',  ( 0.000000000000000000, -31.81777574834303124, 10.70123563439434733 ) ) ;
#8343 = CARTESIAN_POINT ( 'NONE',  ( -68.78002826185903018, 31.00000000000000711, -23.46745878763085358 ) ) ;
#8344 = VERTEX_POINT ( 'NONE', #18956 ) ;
#8345 = CARTESIAN_POINT ( 'NONE',  ( -12.69999999999999929, 0.000000000000000000, -13.40000000000000213 ) ) ;
#8346 = DIRECTION ( 'NONE',  ( -1.000000000000000000, -0.000000000000000000, 0.000000000000000000 ) ) ;
#8347 = ORIENTED_EDGE ( 'NONE', *, *, #18157, .T. ) ;
#8348 = CARTESIAN_POINT ( 'NONE',  ( 17.99999999999999645, 68.63002662989875091, -93.51962064069435598 ) ) ;
#8349 = ORIENTED_EDGE ( 'NONE', *, *, #30164, .T. ) ;
#8350 = CARTESIAN_POINT ( 'NONE',  ( 6.386360208629404234, 40.00000000000000000, 99.40013590833049761 ) ) ;
#8351 = CARTESIAN_POINT ( 'NONE',  ( 17.33436897218374639, 31.00000000000000355, 22.64673195036552755 ) ) ;
#8353 = CARTESIAN_POINT ( 'NONE',  ( 17.99999999999999645, -30.78424799127063238, -6.672111855473501940 ) ) ;
#8352 = DIRECTION ( 'NONE',  ( 1.000000000000000000, 0.000000000000000000, 0.000000000000000000 ) ) ;
#8354 = CARTESIAN_POINT ( 'NONE',  ( 0.000000000000000000, 0.000000000000000000, 0.000000000000000000 ) ) ;
#8355 = DIRECTION ( 'NONE',  ( -1.000000000000000000, 0.000000000000000000, 0.000000000000000000 ) ) ;
#8356 = EDGE_CURVE ( 'NONE', #26654, #31369, #35262, .T. ) ;
#8357 = ORIENTED_EDGE ( 'NONE', *, *, #6863, .T. ) ;
#8358 = CYLINDRICAL_SURFACE ( 'NONE', #12970, 120.5010000000000190 ) ;
#8359 = CIRCLE ( 'NONE', #38989, 59.00000000000000000 ) ;
#8360 = ORIENTED_EDGE ( 'NONE', *, *, #1893, .T. ) ;
#8361 = CARTESIAN_POINT ( 'NONE',  ( 0.000000000000000000, -88.56657216608570593, -68.87840567546012949 ) ) ;
#8362 = CIRCLE ( 'NONE', #38990, 59.00000000000000000 ) ;
#8363 = CARTESIAN_POINT ( 'NONE',  ( -99.14707074559267141, 31.00000000000000711, 13.06922382031732610 ) ) ;
#8364 = CIRCLE ( 'NONE', #28605, 120.5010000000000190 ) ;
#8365 = DIRECTION ( 'NONE',  ( 0.000000000000000000, 0.1837495178165707566, -0.9829730996839017854 ) ) ;
#8366 = VERTEX_POINT ( 'NONE', #15869 ) ;
#8367 = CARTESIAN_POINT ( 'NONE',  ( -3.925388345520635536, 40.00000000000000000, 29.51202942214662173 ) ) ;
#8368 = EDGE_CURVE ( 'NONE', #10198, #16946, #28696, .T. ) ;
#8369 = ORIENTED_EDGE ( 'NONE', *, *, #43064, .F. ) ;
#8370 = VERTEX_POINT ( 'NONE', #42645 ) ;
#8371 = DIRECTION ( 'NONE',  ( -1.000000000000000000, 0.000000000000000000, 0.000000000000000000 ) ) ;
#8372 = CARTESIAN_POINT ( 'NONE',  ( -24.74979319748359785, 5.944745455504278020, 2.972870684497277427 ) ) ;
#8373 = CARTESIAN_POINT ( 'NONE',  ( 0.000000000000000000, -100.8494052988175298, 65.95368414178875582 ) ) ;
#8374 = EDGE_CURVE ( 'NONE', #37517, #41239, #41167, .T. ) ;
#8375 = CARTESIAN_POINT ( 'NONE',  ( 17.99999999999999645, -112.5120133921104753, -43.14554256761131512 ) ) ;
#8376 = ORIENTED_EDGE ( 'NONE', *, *, #18839, .T. ) ;
#8377 = CARTESIAN_POINT ( 'NONE',  ( 18.00000000000000355, 0.000000000000000000, 0.000000000000000000 ) ) ;
#8378 = VERTEX_POINT ( 'NONE', #25484 ) ;
#8379 = CARTESIAN_POINT ( 'NONE',  ( 0.000000000000000000, -7.220349212960696761, 35.26849241522661771 ) ) ;
#8380 = DIRECTION ( 'NONE',  ( 1.000000000000000000, -1.058513553088275437E-16, 0.000000000000000000 ) ) ;
#8381 = VECTOR ( 'NONE', #35125, 1000.000000000000000 ) ;
#8382 = DIRECTION ( 'NONE',  ( 0.000000000000000000, 1.541976423090494844E-15, 1.000000000000000000 ) ) ;
#8383 = DIRECTION ( 'NONE',  ( -1.000000000000000000, -0.000000000000000000, -0.000000000000000000 ) ) ;
#8384 = VERTEX_POINT ( 'NONE', #22640 ) ;
#8385 = ORIENTED_EDGE ( 'NONE', *, *, #7064, .F. ) ;
#8386 = DIRECTION ( 'NONE',  ( -1.000000000000000000, -0.000000000000000000, -0.000000000000000000 ) ) ;
#8387 = DIRECTION ( 'NONE',  ( 0.000000000000000000, 0.9822872507286879440, 0.1873813145857285700 ) ) ;
#8389 = EDGE_CURVE ( 'NONE', #38794, #11221, #39791, .T. ) ;
#8388 = AXIS2_PLACEMENT_3D ( 'NONE', #24905, #28584, #21422 ) ;
#8390 = VERTEX_POINT ( 'NONE', #29590 ) ;
#8392 = ORIENTED_EDGE ( 'NONE', *, *, #6812, .T. ) ;
#8391 = CARTESIAN_POINT ( 'NONE',  ( 6.004904395537136175, 0.000000000000000000, 0.000000000000000000 ) ) ;
#8393 = AXIS2_PLACEMENT_3D ( 'NONE', #30238, #9936, #23285 ) ;
#8394 = CARTESIAN_POINT ( 'NONE',  ( 46.89968353241609833, 31.00000000000000355, -2.988513402017745513 ) ) ;
#8397 = EDGE_CURVE ( 'NONE', #35404, #40182, #23806, .T. ) ;
#8396 = ORIENTED_EDGE ( 'NONE', *, *, #29483, .T. ) ;
#8395 = CIRCLE ( 'NONE', #2783, 20.00000000000000355 ) ;
#8398 = DIRECTION ( 'NONE',  ( 0.000000000000000000, 0.000000000000000000, 1.000000000000000000 ) ) ;
#8400 = CARTESIAN_POINT ( 'NONE',  ( 0.000000000000000000, 35.54274411428055913, 115.1399337407607959 ) ) ;
#8399 = DIRECTION ( 'NONE',  ( 0.000000000000000000, 1.000000000000000000, 0.000000000000000000 ) ) ;
#8401 = ORIENTED_EDGE ( 'NONE', *, *, #5110, .T. ) ;
#8402 = CARTESIAN_POINT ( 'NONE',  ( 0.000000000000000000, 0.000000000000000000, 0.000000000000000000 ) ) ;
#8403 = CARTESIAN_POINT ( 'NONE',  ( -7.911223860816524400, 40.00000000000000000, 59.30865348673674475 ) ) ;
#8404 = DIRECTION ( 'NONE',  ( 0.000000000000000000, 0.000000000000000000, 1.000000000000000000 ) ) ;
#8405 = CARTESIAN_POINT ( 'NONE',  ( -10.00000000000000000, 0.000000000000000000, 0.000000000000000000 ) ) ;
#8406 = ORIENTED_EDGE ( 'NONE', *, *, #41186, .F. ) ;
#8407 = DIRECTION ( 'NONE',  ( 1.000000000000000000, 0.000000000000000000, 0.000000000000000000 ) ) ;
#8408 = EDGE_CURVE ( 'NONE', #31369, #18067, #23133, .T. ) ;
#8409 = ORIENTED_EDGE ( 'NONE', *, *, #25232, .F. ) ;
#8410 = DIRECTION ( 'NONE',  ( 0.000000000000000000, 0.8183027759081702435, -0.5747874102144052699 ) ) ;
#8411 = DIRECTION ( 'NONE',  ( 0.000000000000000000, 0.000000000000000000, 1.000000000000000000 ) ) ;
#8412 = CIRCLE ( 'NONE', #15397, 47.49900000000000233 ) ;
#8413 = CARTESIAN_POINT ( 'NONE',  ( -43.59452257625678584, 31.00000000000000355, -56.81327804312699925 ) ) ;
#8414 = DIRECTION ( 'NONE',  ( -1.000000000000000000, 0.000000000000000000, 0.000000000000000000 ) ) ;
#8415 = ORIENTED_EDGE ( 'NONE', *, *, #37583, .F. ) ;
#8416 = AXIS2_PLACEMENT_3D ( 'NONE', #318, #3807, #30253 ) ;
#8417 = FILL_AREA_STYLE ('',( #15230 ) ) ;
#8418 = EDGE_CURVE ( 'NONE', #35542, #7493, #3537, .T. ) ;
#8419 = VECTOR ( 'NONE', #26751, 1000.000000000000000 ) ;
#8420 = AXIS2_PLACEMENT_3D ( 'NONE', #30411, #486, #3096 ) ;
#8421 = ORIENTED_EDGE ( 'NONE', *, *, #8240, .F. ) ;
#8422 = DIRECTION ( 'NONE',  ( -1.000000000000000000, 0.000000000000000000, 0.000000000000000000 ) ) ;
#8423 = ADVANCED_FACE ( 'NONE', ( #17167 ), #6875, .T. ) ;
#8424 = CIRCLE ( 'NONE', #3, 16.00000000000023448 ) ;
#8425 = FACE_OUTER_BOUND ( 'NONE', #31387, .T. ) ;
#8426 = CARTESIAN_POINT ( 'NONE',  ( -41.82916961767931951, 31.00000000000000355, -72.66191475361131324 ) ) ;
#8427 = CARTESIAN_POINT ( 'NONE',  ( -50.81742119984753714, 40.00000000000000000, -66.42451308377114572 ) ) ;
#8428 = AXIS2_PLACEMENT_3D ( 'NONE', #34620, #1665, #1011 ) ;
#8429 = CARTESIAN_POINT ( 'NONE',  ( 18.00000000000000355, -29.60891106212762125, -37.14118181634796656 ) ) ;
#8430 = VERTEX_POINT ( 'NONE', #33493 ) ;
#8431 = CYLINDRICAL_SURFACE ( 'NONE', #42981, 116.0000000000000000 ) ;
#8432 = VERTEX_POINT ( 'NONE', #9927 ) ;
#8433 = CARTESIAN_POINT ( 'NONE',  ( 17.99999999999999645, 47.31079789947484926, 105.9135893174952656 ) ) ;
#8434 = CARTESIAN_POINT ( 'NONE',  ( 2.027755760259328333E-13, -150.5000000000013642, 9.999999999999586109 ) ) ;
#8436 = ORIENTED_EDGE ( 'NONE', *, *, #29956, .T. ) ;
#8435 = DIRECTION ( 'NONE',  ( -1.000000000000000000, -0.000000000000000000, -0.000000000000000000 ) ) ;
#8437 = VECTOR ( 'NONE', #13161, 1000.000000000000000 ) ;
#8438 = CARTESIAN_POINT ( 'NONE',  ( 0.000000000000000000, 0.000000000000000000, 0.000000000000000000 ) ) ;
#8439 = ORIENTED_EDGE ( 'NONE', *, *, #986, .F. ) ;
#8440 = DIRECTION ( 'NONE',  ( 1.000000000000000000, 0.000000000000000000, 0.000000000000000000 ) ) ;
#8441 = DIRECTION ( 'NONE',  ( 0.000000000000000000, 0.000000000000000000, 1.000000000000000000 ) ) ;
#8442 = ORIENTED_EDGE ( 'NONE', *, *, #10611, .F. ) ;
#8443 = EDGE_CURVE ( 'NONE', #17756, #38173, #26594, .T. ) ;
#8444 = CARTESIAN_POINT ( 'NONE',  ( 17.99999999999999645, -28.62203781743013664, 14.19692359621445199 ) ) ;
#8445 = EDGE_CURVE ( 'NONE', #1680, #42118, #30230, .T. ) ;
#8446 = DIRECTION ( 'NONE',  ( -1.000000000000000000, -0.000000000000000000, -0.000000000000000000 ) ) ;
#8447 = ADVANCED_FACE ( 'NONE', ( #3143 ), #40454, .F. ) ;
#8448 = EDGE_CURVE ( 'NONE', #39845, #31846, #9137, .T. ) ;
#8450 = DIRECTION ( 'NONE',  ( 1.000000000000000000, -0.000000000000000000, -0.000000000000000000 ) ) ;
#8449 = CARTESIAN_POINT ( 'NONE',  ( 9.000000000000001776, 6.854627147200274884, -115.7972974066012881 ) ) ;
#8451 = ORIENTED_EDGE ( 'NONE', *, *, #30150, .F. ) ;
#8452 = FACE_OUTER_BOUND ( 'NONE', #31586, .T. ) ;
#8454 = ORIENTED_EDGE ( 'NONE', *, *, #37718, .T. ) ;
#8453 = CIRCLE ( 'NONE', #17556, 51.99999999999999289 ) ;
#8455 = CARTESIAN_POINT ( 'NONE',  ( 104.9999999999993321, -2.293336392629658115E-13, -32.00000000000000000 ) ) ;
#8456 = CARTESIAN_POINT ( 'NONE',  ( 1.888402776346428613, 40.00000000000000000, 29.39821258742166776 ) ) ;
#8457 = CARTESIAN_POINT ( 'NONE',  ( 6.075999999999997847, 2.346238345499656945E-15, -19.11697999999999809 ) ) ;
#8458 = DIRECTION ( 'NONE',  ( 1.000000000000000000, 0.000000000000000000, 0.000000000000000000 ) ) ;
#8459 = CIRCLE ( 'NONE', #32835, 116.0000000000000000 ) ;
#8460 = DIRECTION ( 'NONE',  ( -1.000000000000000000, 0.000000000000000000, 0.000000000000000000 ) ) ;
#8461 = ORIENTED_EDGE ( 'NONE', *, *, #42063, .T. ) ;
#8462 = CARTESIAN_POINT ( 'NONE',  ( 0.000000000000000000, 0.000000000000000000, 0.000000000000000000 ) ) ;
#8463 = VERTEX_POINT ( 'NONE', #533 ) ;
#8464 = AXIS2_PLACEMENT_3D ( 'NONE', #21069, #706, #13415 ) ;
#8465 = CYLINDRICAL_SURFACE ( 'NONE', #20439, 59.00000000000000000 ) ;
#8466 = FACE_BOUND ( 'NONE', #34394, .T. ) ;
#8467 = CARTESIAN_POINT ( 'NONE',  ( -23.50435451693408950, 31.00000000000000355, 30.64856077952424940 ) ) ;
#8468 = EDGE_LOOP ( 'NONE', ( #29319, #34464, #6901, #4215 ) ) ;
#8469 = DIRECTION ( 'NONE',  ( -1.000000000000000000, 0.000000000000000000, 0.000000000000000000 ) ) ;
#8470 = DIRECTION ( 'NONE',  ( -1.000000000000000000, 0.000000000000000000, 0.000000000000000000 ) ) ;
#8471 = EDGE_CURVE ( 'NONE', #23588, #6470, #32129, .T. ) ;
#8472 = CARTESIAN_POINT ( 'NONE',  ( 60.46509673945340779, 31.00000000000000000, 46.37897171330492085 ) ) ;
#8473 = EDGE_CURVE ( 'NONE', #31578, #28014, #26964, .T. ) ;
#8474 = ORIENTED_EDGE ( 'NONE', *, *, #42095, .F. ) ;
#8475 = CARTESIAN_POINT ( 'NONE',  ( -25.29816761085220378, 31.00000000000000355, 43.63644233510515846 ) ) ;
#8476 = CARTESIAN_POINT ( 'NONE',  ( 11.43299787627070607, 40.00000000000000000, 86.72764684403134083 ) ) ;
#8477 = ORIENTED_EDGE ( 'NONE', *, *, #7399, .F. ) ;
#8478 = CIRCLE ( 'NONE', #33547, 58.99999999999999289 ) ;
#8479 = CARTESIAN_POINT ( 'NONE',  ( -4.175002511812151873, -2.208363329454905877, -3.469254087858246738 ) ) ;
#8480 = VECTOR ( 'NONE', #23292, 1000.000000000000000 ) ;
#8481 = CARTESIAN_POINT ( 'NONE',  ( 0.000000000000000000, 92.25992191227393846, 77.51514567967427638 ) ) ;
#8482 = CYLINDRICAL_SURFACE ( 'NONE', #23377, 51.99999999999999289 ) ;
#8483 = AXIS2_PLACEMENT_3D ( 'NONE', #42745, #3253, #15978 ) ;
#8485 = VERTEX_POINT ( 'NONE', #16518 ) ;
#8484 = CARTESIAN_POINT ( 'NONE',  ( 17.99999999999999645, 111.2721026680458749, 14.38025178762809908 ) ) ;
#8486 = DIRECTION ( 'NONE',  ( 0.000000000000000000, -0.05322217484216511946, -0.9985826956767627216 ) ) ;
#8487 = DIRECTION ( 'NONE',  ( 0.000000000000000000, -0.9618256431728219313, 0.2736629900720728981 ) ) ;
#8488 = ORIENTED_EDGE ( 'NONE', *, *, #32242, .F. ) ;
#8489 = CARTESIAN_POINT ( 'NONE',  ( 8.815036365794538753, 40.00000000000000000, 66.85656860134390911 ) ) ;
#8490 = FACE_OUTER_BOUND ( 'NONE', #6364, .T. ) ;
#8491 = AXIS2_PLACEMENT_3D ( 'NONE', #6997, #17075, #206 ) ;
#8492 = ORIENTED_EDGE ( 'NONE', *, *, #6127, .T. ) ;
#8493 = CARTESIAN_POINT ( 'NONE',  ( 0.000000000000000000, -80.74349901498459303, 77.90224541347254217 ) ) ;
#8494 = CYLINDRICAL_SURFACE ( 'NONE', #35425, 120.5010000000000190 ) ;
#8495 = EDGE_CURVE ( 'NONE', #8083, #2224, #18259, .T. ) ;
#8496 = EDGE_CURVE ( 'NONE', #10112, #36592, #33286, .T. ) ;
#8497 = CARTESIAN_POINT ( 'NONE',  ( 18.00000000000000355, -8.053585752062225822, 46.81126742072019908 ) ) ;
#8498 = EDGE_LOOP ( 'NONE', ( #40453, #22772, #10731, #33358 ) ) ;
#8499 = EDGE_CURVE ( 'NONE', #25660, #15814, #36529, .T. ) ;
#8500 = VERTEX_POINT ( 'NONE', #30666 ) ;
#8501 = CYLINDRICAL_SURFACE ( 'NONE', #965, 36.00000000000000000 ) ;
#8502 = ORIENTED_EDGE ( 'NONE', *, *, #411, .T. ) ;
#8503 = CARTESIAN_POINT ( 'NONE',  ( 0.000000000000000000, 105.3681574666269256, -38.54638589714782881 ) ) ;
#8504 = DIRECTION ( 'NONE',  ( 0.000000000000000000, 0.9996456111234526265, -0.02662052143777152158 ) ) ;
#8505 = DIRECTION ( 'NONE',  ( 0.000000000000000000, 0.000000000000000000, 1.000000000000000000 ) ) ;
#8506 = EDGE_CURVE ( 'NONE', #13412, #24013, #40480, .T. ) ;
#8507 = CARTESIAN_POINT ( 'NONE',  ( 0.000000000000000000, 0.000000000000000000, 0.000000000000000000 ) ) ;
#8508 = EDGE_LOOP ( 'NONE', ( #578, #38590, #33423, #40681 ) ) ;
#8509 = CYLINDRICAL_SURFACE ( 'NONE', #25280, 116.0000000000000000 ) ;
#8510 = AXIS2_PLACEMENT_3D ( 'NONE', #28175, #38395, #41880 ) ;
#8511 = CIRCLE ( 'NONE', #2900, 47.49900000000000233 ) ;
#8512 = AXIS2_PLACEMENT_3D ( 'NONE', #2862, #39102, #9663 ) ;
#8513 = CYLINDRICAL_SURFACE ( 'NONE', #8510, 47.49900000000000233 ) ;
#8514 = EDGE_CURVE ( 'NONE', #21952, #29194, #4973, .T. ) ;
#8515 = VERTEX_POINT ( 'NONE', #23919 ) ;
#8516 = DIRECTION ( 'NONE',  ( -1.000000000000000000, 0.000000000000000000, -0.000000000000000000 ) ) ;
#8517 = VECTOR ( 'NONE', #35103, 1000.000000000000000 ) ;
#8518 = DIRECTION ( 'NONE',  ( 1.000000000000000000, 0.000000000000000000, 0.000000000000000000 ) ) ;
#8519 = DIRECTION ( 'NONE',  ( -0.7071067811865413555, -6.123233995736766036E-17, 0.7071067811865536790 ) ) ;
#8520 = CARTESIAN_POINT ( 'NONE',  ( 17.99999999999999645, -31.80866420683992857, 16.59709355804118402 ) ) ;
#8521 = CARTESIAN_POINT ( 'NONE',  ( -47.94314659152439617, 31.00000000000000355, -16.27230485535717719 ) ) ;
#8522 = CIRCLE ( 'NONE', #17631, 59.00000000000001421 ) ;
#8523 = ORIENTED_EDGE ( 'NONE', *, *, #9746, .F. ) ;
#8525 = DIRECTION ( 'NONE',  ( 0.9470131699890049770, 1.701542661702850483E-16, 0.3211947320043963550 ) ) ;
#8524 = DIRECTION ( 'NONE',  ( 0.000000000000000000, 0.000000000000000000, 1.000000000000000000 ) ) ;
#8526 = ORIENTED_EDGE ( 'NONE', *, *, #8743, .F. ) ;
#8527 = CARTESIAN_POINT ( 'NONE',  ( -44.33513214241411760, 40.00000000000000000, 38.89722855811361768 ) ) ;
#8528 = DIRECTION ( 'NONE',  ( -1.000000000000000000, -0.000000000000000000, -0.000000000000000000 ) ) ;
#8529 = DIRECTION ( 'NONE',  ( -1.000000000000000000, 0.000000000000000000, 0.000000000000000000 ) ) ;
#8530 = DIRECTION ( 'NONE',  ( -1.000000000000000000, 0.000000000000000000, -0.000000000000000000 ) ) ;
#8531 = DIRECTION ( 'NONE',  ( 1.000000000000000000, -1.373900992973642066E-15, -3.854941057726257326E-16 ) ) ;
#8532 = AXIS2_PLACEMENT_3D ( 'NONE', #24440, #14390, #22032 ) ;
#8533 = EDGE_LOOP ( 'NONE', ( #21293, #11741, #40964, #39910 ) ) ;
#8534 = CARTESIAN_POINT ( 'NONE',  ( -10.31048697494744815, 40.00000000000000000, -30.34325702988586215 ) ) ;
#8535 = ORIENTED_EDGE ( 'NONE', *, *, #27025, .T. ) ;
#8536 = CARTESIAN_POINT ( 'NONE',  ( 0.000000000000000000, 16.77727049691110750, 27.19001440037552086 ) ) ;
#8537 = CARTESIAN_POINT ( 'NONE',  ( 2.500000000000000000, 2.357898499370431722, -2.818925648462311528E-15 ) ) ;
#8538 = VECTOR ( 'NONE', #17646, 1000.000000000000000 ) ;
#8539 = EDGE_LOOP ( 'NONE', ( #27289, #22347, #21596, #18498 ) ) ;
#8540 = DIRECTION ( 'NONE',  ( 0.000000000000000000, 0.4817536741017162116, -0.8763066800438631399 ) ) ;
#8541 = AXIS2_PLACEMENT_3D ( 'NONE', #1453, #8654, #11305 ) ;
#8542 = EDGE_CURVE ( 'NONE', #35135, #14587, #41894, .T. ) ;
#8543 = CYLINDRICAL_SURFACE ( 'NONE', #8071, 100.0000000000000000 ) ;
#8544 = EDGE_LOOP ( 'NONE', ( #11071, #4990, #41347, #14304 ) ) ;
#8545 = CARTESIAN_POINT ( 'NONE',  ( 1.747541505913279281, -3.837784562140273081, -3.503702292528912299 ) ) ;
#8546 = ORIENTED_EDGE ( 'NONE', *, *, #16994, .F. ) ;
#8547 = AXIS2_PLACEMENT_3D ( 'NONE', #11547, #31602, #41627 ) ;
#8548 = VERTEX_POINT ( 'NONE', #37186 ) ;
#8549 = CARTESIAN_POINT ( 'NONE',  ( 0.000000000000000000, -93.26762629039376407, -76.29967815892449323 ) ) ;
#8550 = CARTESIAN_POINT ( 'NONE',  ( -79.00001692110807028, 31.00000000000000711, 21.04436337235335230 ) ) ;
#8551 = ORIENTED_EDGE ( 'NONE', *, *, #788, .F. ) ;
#8552 = CARTESIAN_POINT ( 'NONE',  ( -4.211405944401398038, -2.460460786169389902, -3.751298493805494072 ) ) ;
#8553 = CARTESIAN_POINT ( 'NONE',  ( 18.00000000000000355, 26.17370628620655637, 39.63700417846172286 ) ) ;
#8554 = ORIENTED_EDGE ( 'NONE', *, *, #14856, .T. ) ;
#8555 = EDGE_CURVE ( 'NONE', #19787, #10716, #29372, .T. ) ;
#8556 = CARTESIAN_POINT ( 'NONE',  ( 17.99999999999999645, -0.04937522221101428577, -31.94951095880159286 ) ) ;
#8557 = CARTESIAN_POINT ( 'NONE',  ( -91.07534658258109062, 40.00000000000000711, 44.76935032130646874 ) ) ;
#8558 = CARTESIAN_POINT ( 'NONE',  ( -21.70016380022026681, 31.00000000000000355, -5.809120511592387182 ) ) ;
#8559 = EDGE_CURVE ( 'NONE', #25806, #20272, #14102, .T. ) ;
#8561 = CARTESIAN_POINT ( 'NONE',  ( 17.99999999999999645, 100.6739960869724655, -49.52796165323157851 ) ) ;
#8560 = CARTESIAN_POINT ( 'NONE',  ( 31.80287614962791665, -34.05525454449571754, 69.29271901957253021 ) ) ;
#8562 = EDGE_CURVE ( 'NONE', #37783, #40263, #23711, .T. ) ;
#8563 = DIRECTION ( 'NONE',  ( 0.000000000000000000, 0.000000000000000000, -1.000000000000000000 ) ) ;
#8564 = DIRECTION ( 'NONE',  ( 0.000000000000000000, 0.8443279255020161855, -0.5358267949789946583 ) ) ;
#8565 = ORIENTED_EDGE ( 'NONE', *, *, #34904, .F. ) ;
#8566 = VECTOR ( 'NONE', #33952, 1000.000000000000000 ) ;
#8567 = DIRECTION ( 'NONE',  ( 0.000000000000000000, -0.7705132427757949154, 0.6374239897486827511 ) ) ;
#8568 = ORIENTED_EDGE ( 'NONE', *, *, #19362, .F. ) ;
#8569 = DIRECTION ( 'NONE',  ( -1.000000000000000000, -0.000000000000000000, -0.000000000000000000 ) ) ;
#8570 = CARTESIAN_POINT ( 'NONE',  ( 70.70367055548476287, 31.00000000000000000, -62.02616482874480397 ) ) ;
#8571 = CARTESIAN_POINT ( 'NONE',  ( 17.99999999999999645, 17.33727698085173330, 110.8498592715974098 ) ) ;
#8572 = ORIENTED_EDGE ( 'NONE', *, *, #35770, .T. ) ;
#8573 = CARTESIAN_POINT ( 'NONE',  ( -26.91141215548883991, 40.00000000000000000, 30.57553017915055449 ) ) ;
#8574 = EDGE_CURVE ( 'NONE', #41039, #20422, #7768, .T. ) ;
#8575 = CIRCLE ( 'NONE', #20453, 59.00000000000000000 ) ;
#8576 = ORIENTED_EDGE ( 'NONE', *, *, #4895, .T. ) ;
#8577 = ORIENTED_EDGE ( 'NONE', *, *, #11974, .F. ) ;
#8578 = LINE ( 'NONE', #15386, #8775 ) ;
#8579 = CARTESIAN_POINT ( 'NONE',  ( 17.99999999999999645, 0.000000000000000000, 0.000000000000000000 ) ) ;
#8580 = DIRECTION ( 'NONE',  ( 0.000000000000000000, 0.000000000000000000, -1.000000000000000000 ) ) ;
#8581 = CARTESIAN_POINT ( 'NONE',  ( 0.000000000000000000, 51.19683565102443623, 9.104066087303637644 ) ) ;
#8582 = DIRECTION ( 'NONE',  ( 0.000000000000000000, 0.9407002666710341243, -0.3392388661180278930 ) ) ;
#8583 = ORIENTED_EDGE ( 'NONE', *, *, #13119, .F. ) ;
#8584 = DIRECTION ( 'NONE',  ( 0.000000000000000000, -0.9822872507286865007, -0.1873813145857356199 ) ) ;
#8585 = ORIENTED_EDGE ( 'NONE', *, *, #2222, .F. ) ;
#8586 = LINE ( 'NONE', #42801, #27103 ) ;
#8587 = FACE_OUTER_BOUND ( 'NONE', #36805, .T. ) ;
#8588 = CARTESIAN_POINT ( 'NONE',  ( 0.000000000000000000, 110.3490479609632615, -20.28201389785435182 ) ) ;
#8589 = CIRCLE ( 'NONE', #1643, 20.00000000000000711 ) ;
#8590 = DIRECTION ( 'NONE',  ( -1.000000000000000000, 0.000000000000000000, -0.000000000000000000 ) ) ;
#8591 = ORIENTED_EDGE ( 'NONE', *, *, #24856, .F. ) ;
#8592 = ORIENTED_EDGE ( 'NONE', *, *, #2958, .T. ) ;
#8593 = EDGE_CURVE ( 'NONE', #38227, #32590, #2845, .T. ) ;
#8594 = CARTESIAN_POINT ( 'NONE',  ( 0.000000000000000000, -14.84191762912334767, 27.78316904333121684 ) ) ;
#8595 = VECTOR ( 'NONE', #26201, 1000.000000000000000 ) ;
#8596 = ORIENTED_EDGE ( 'NONE', *, *, #25211, .F. ) ;
#8598 = ORIENTED_EDGE ( 'NONE', *, *, #3080, .F. ) ;
#8597 = CARTESIAN_POINT ( 'NONE',  ( 17.99999999999999645, 18.25486108452660972, -25.66996392254254644 ) ) ;
#8599 = CARTESIAN_POINT ( 'NONE',  ( 42.13926417418816328, 31.00000000000000355, -36.83769365847010846 ) ) ;
#8600 = ORIENTED_EDGE ( 'NONE', *, *, #9916, .F. ) ;
#8601 = DIRECTION ( 'NONE',  ( -3.009274222672345096E-17, -1.000000000000000000, 2.455023325076454960E-18 ) ) ;
#8602 = EDGE_CURVE ( 'NONE', #41947, #13537, #8459, .T. ) ;
#8603 = DIRECTION ( 'NONE',  ( -1.000000000000000000, -0.000000000000000000, 0.000000000000000000 ) ) ;
#8604 = VERTEX_POINT ( 'NONE', #4235 ) ;
#8606 = CARTESIAN_POINT ( 'NONE',  ( -4.660665814384791439, 40.00000000000000000, 69.59371722953135020 ) ) ;
#8605 = AXIS2_PLACEMENT_3D ( 'NONE', #25733, #2746, #25518 ) ;
#8607 = EDGE_CURVE ( 'NONE', #29204, #43139, #14059, .T. ) ;
#8608 = DIRECTION ( 'NONE',  ( 0.000000000000000000, 0.000000000000000000, 1.000000000000000000 ) ) ;
#8609 = CIRCLE ( 'NONE', #3998, 51.99999999999999289 ) ;
#8610 = ADVANCED_FACE ( 'NONE', ( #15197 ), #17607, .F. ) ;
#8611 = DIRECTION ( 'NONE',  ( 0.000000000000000000, -0.3140767120219556952, 0.9493976084683790617 ) ) ;
#8612 = ORIENTED_EDGE ( 'NONE', *, *, #7321, .T. ) ;
#8613 = DIRECTION ( 'NONE',  ( 0.000000000000000000, 0.3140767120219428166, 0.9493976084683832806 ) ) ;
#8614 = VECTOR ( 'NONE', #14049, 1000.000000000000000 ) ;
#8615 = ORIENTED_EDGE ( 'NONE', *, *, #17777, .F. ) ;
#8616 =( REPRESENTATION_RELATIONSHIP ('NONE','NONE', #330, #41895 ) REPRESENTATION_RELATIONSHIP_WITH_TRANSFORMATION ( #16826 )SHAPE_REPRESENTATION_RELATIONSHIP( ) );
#8617 = DIRECTION ( 'NONE',  ( 0.000000000000000000, 0.000000000000000000, 1.000000000000000000 ) ) ;
#8618 = DIRECTION ( 'NONE',  ( 3.009274222672345096E-17, 1.000000000000000000, -2.455023325076454960E-18 ) ) ;
#8619 = CIRCLE ( 'NONE', #33684, 116.0000000000000000 ) ;
#8620 = CARTESIAN_POINT ( 'NONE',  ( -69.34045338167970840, 31.00000000000000711, 9.142281554609933636 ) ) ;
#8621 = CYLINDRICAL_SURFACE ( 'NONE', #30918, 59.00000000000000000 ) ;
#8622 = VERTEX_POINT ( 'NONE', #18263 ) ;
#8623 = CIRCLE ( 'NONE', #40645, 2.500000000000000444 ) ;
#8624 = LINE ( 'NONE', #24609, #38636 ) ;
#8625 = VECTOR ( 'NONE', #42490, 1000.000000000000000 ) ;
#8626 = ADVANCED_FACE ( 'NONE', ( #14751 ), #31317, .F. ) ;
#8627 = VERTEX_POINT ( 'NONE', #4681 ) ;
#8628 = CARTESIAN_POINT ( 'NONE',  ( 17.99999999999999645, 0.000000000000000000, 0.000000000000000000 ) ) ;
#8629 = ADVANCED_FACE ( 'NONE', ( #40886 ), #27617, .T. ) ;
#8630 = DIRECTION ( 'NONE',  ( -1.000000000000000000, 0.000000000000000000, -0.000000000000000000 ) ) ;
#8631 = CARTESIAN_POINT ( 'NONE',  ( -78.26717753304431824, 31.00000000000000711, -26.69481836928899554 ) ) ;
#8632 = CARTESIAN_POINT ( 'NONE',  ( -45.36921519482122989, 40.00000000000000711, 78.33339762292068542 ) ) ;
#8633 = FACE_OUTER_BOUND ( 'NONE', #33017, .T. ) ;
#8634 = VECTOR ( 'NONE', #15954, 999.9999999999998863 ) ;
#8635 = ORIENTED_EDGE ( 'NONE', *, *, #22428, .T. ) ;
#8636 = DIRECTION ( 'NONE',  ( 0.000000000000000000, 0.000000000000000000, 1.000000000000000000 ) ) ;
#8637 = ORIENTED_EDGE ( 'NONE', *, *, #18227, .F. ) ;
#8638 = CIRCLE ( 'NONE', #17718, 120.5010000000000190 ) ;
#8639 = DIRECTION ( 'NONE',  ( 0.000000000000000000, -1.599473849036242511E-14, -1.000000000000000000 ) ) ;
#8640 = EDGE_CURVE ( 'NONE', #31678, #6403, #18290, .T. ) ;
#8641 = DIRECTION ( 'NONE',  ( 0.000000000000000000, 0.000000000000000000, -1.000000000000000000 ) ) ;
#8643 = ORIENTED_EDGE ( 'NONE', *, *, #9591, .F. ) ;
#8642 = DIRECTION ( 'NONE',  ( 0.000000000000000000, 0.000000000000000000, 1.000000000000000000 ) ) ;
#8644 = CARTESIAN_POINT ( 'NONE',  ( 9.000000000000000000, 0.6168405712491942250, -35.99471499692226217 ) ) ;
#8645 = ORIENTED_EDGE ( 'NONE', *, *, #2767, .F. ) ;
#8646 = CARTESIAN_POINT ( 'NONE',  ( -10.00000000000000000, 0.000000000000000000, 0.000000000000000000 ) ) ;
#8647 = CIRCLE ( 'NONE', #4457, 59.00000000000000711 ) ;
#8648 = EDGE_CURVE ( 'NONE', #18183, #26358, #26620, .T. ) ;
#8649 = DIRECTION ( 'NONE',  ( -1.000000000000000000, 0.000000000000000000, -0.000000000000000000 ) ) ;
#8650 = DIRECTION ( 'NONE',  ( 0.000000000000000000, 0.000000000000000000, 1.000000000000000000 ) ) ;
#8651 = AXIS2_PLACEMENT_3D ( 'NONE', #19563, #35874, #26097 ) ;
#8652 = ORIENTED_EDGE ( 'NONE', *, *, #34873, .F. ) ;
#8653 = CARTESIAN_POINT ( 'NONE',  ( -1.587008504153756938, 31.00000000000000355, -24.39691638390477380 ) ) ;
#8654 = DIRECTION ( 'NONE',  ( -1.000000000000000000, -0.000000000000000000, -0.000000000000000000 ) ) ;
#8655 = AXIS2_PLACEMENT_3D ( 'NONE', #29625, #13061, #26361 ) ;
#8656 = EDGE_CURVE ( 'NONE', #10648, #300, #21088, .T. ) ;
#8658 = DIRECTION ( 'NONE',  ( 3.996523416598930318E-16, -2.658563593772947863E-15, -1.000000000000000000 ) ) ;
#8657 = DIRECTION ( 'NONE',  ( 0.000000000000000000, 0.000000000000000000, 1.000000000000000000 ) ) ;
#8659 = AXIS2_PLACEMENT_3D ( 'NONE', #12795, #39161, #26107 ) ;
#8660 = EDGE_LOOP ( 'NONE', ( #33670, #37022, #26076, #245 ) ) ;
#8661 = DIRECTION ( 'NONE',  ( 0.000000000000000000, 0.000000000000000000, 1.000000000000000000 ) ) ;
#8662 = ORIENTED_EDGE ( 'NONE', *, *, #39803, .F. ) ;
#8663 = DIRECTION ( 'NONE',  ( -3.009274222672345096E-17, -1.000000000000000000, 2.455023325076454960E-18 ) ) ;
#8664 = CARTESIAN_POINT ( 'NONE',  ( -30.82418422902937039, 40.00000000000000000, 26.94311707097686792 ) ) ;
#8665 = DIRECTION ( 'NONE',  ( 1.000000000000000000, 0.000000000000000000, 0.000000000000000000 ) ) ;
#8666 = EDGE_CURVE ( 'NONE', #35643, #1340, #33552, .T. ) ;
#8667 = CARTESIAN_POINT ( 'NONE',  ( -10.00000000000000000, 0.000000000000000000, 0.000000000000000000 ) ) ;
#8668 = CARTESIAN_POINT ( 'NONE',  ( 17.99999999999999645, 0.000000000000000000, 0.000000000000000000 ) ) ;
#8669 = ORIENTED_EDGE ( 'NONE', *, *, #30083, .F. ) ;
#8670 = CARTESIAN_POINT ( 'NONE',  ( 0.000000000000000000, 78.18175027177548486, -85.69488855492920720 ) ) ;
#8671 = ORIENTED_EDGE ( 'NONE', *, *, #6347, .T. ) ;
#8672 = VECTOR ( 'NONE', #8524, 1000.000000000000000 ) ;
#8673 = CARTESIAN_POINT ( 'NONE',  ( 17.99999999999999645, 0.000000000000000000, 0.000000000000000000 ) ) ;
#8674 = CARTESIAN_POINT ( 'NONE',  ( 0.3000000000000028200, -14.69693845669907084, -1.199999999999999956 ) ) ;
#8675 = CARTESIAN_POINT ( 'NONE',  ( 33.47591237148697729, 31.00000000000000355, -8.973542178613062248 ) ) ;
#8676 = ORIENTED_EDGE ( 'NONE', *, *, #25735, .F. ) ;
#8677 = CYLINDRICAL_SURFACE ( 'NONE', #8605, 15.99999999999998579 ) ;
#8678 = VECTOR ( 'NONE', #17888, 1000.000000000000000 ) ;
#8679 = AXIS2_PLACEMENT_3D ( 'NONE', #29666, #42940, #26395 ) ;
#8680 = DIRECTION ( 'NONE',  ( 0.000000000000000000, 0.000000000000000000, 1.000000000000000000 ) ) ;
#8681 = CARTESIAN_POINT ( 'NONE',  ( -72.56464488860213180, 31.00000000000000711, -35.76892886290303863 ) ) ;
#8682 = EDGE_CURVE ( 'NONE', #18274, #10688, #19667, .T. ) ;
#8683 = EDGE_CURVE ( 'NONE', #32974, #9752, #20888, .T. ) ;
#8684 = ORIENTED_EDGE ( 'NONE', *, *, #7212, .F. ) ;
#8685 = CARTESIAN_POINT ( 'NONE',  ( -47.35250803175854628, 31.00000000000000355, -23.44639516808300073 ) ) ;
#8686 = ADVANCED_FACE ( 'NONE', ( #7740 ), #1182, .T. ) ;
#8687 = EDGE_CURVE ( 'NONE', #19812, #37957, #1614, .T. ) ;
#8688 = AXIS2_PLACEMENT_3D ( 'NONE', #23528, #36794, #6900 ) ;
#8689 = CARTESIAN_POINT ( 'NONE',  ( 12.12865573427490062, 40.00000000000000000, -92.11205733446308841 ) ) ;
#8690 = CIRCLE ( 'NONE', #4504, 10.99999999999999822 ) ;
#8691 = EDGE_LOOP ( 'NONE', ( #21194, #10462, #7293, #6050 ) ) ;
#8692 = DIRECTION ( 'NONE',  ( 1.000000000000000000, 0.000000000000000000, 0.000000000000000000 ) ) ;
#8693 = CYLINDRICAL_SURFACE ( 'NONE', #25029, 116.0000000000000000 ) ;
#8694 = DIRECTION ( 'NONE',  ( 0.000000000000000000, 0.5963673585385025344, -0.8027116379309628957 ) ) ;
#8696 = ORIENTED_EDGE ( 'NONE', *, *, #10733, .F. ) ;
#8695 = DIRECTION ( 'NONE',  ( 0.000000000000000000, 0.000000000000000000, 1.000000000000000000 ) ) ;
#8697 = FACE_OUTER_BOUND ( 'NONE', #38538, .T. ) ;
#8698 = CARTESIAN_POINT ( 'NONE',  ( 2.649999999999768541, 150.5000000000013642, 10.00000000000041567 ) ) ;
#8699 = AXIS2_PLACEMENT_3D ( 'NONE', #42623, #39570, #9903 ) ;
#8700 = VERTEX_POINT ( 'NONE', #41314 ) ;
#8701 = CARTESIAN_POINT ( 'NONE',  ( -69.89583333424914713, 40.00000000000000711, 4.581489278091138040 ) ) ;
#8702 = LINE ( 'NONE', #11801, #10361 ) ;
#8703 = VERTEX_POINT ( 'NONE', #11690 ) ;
#8704 = DIRECTION ( 'NONE',  ( 0.000000000000000000, 0.2631025642275152121, 0.9647678688145175929 ) ) ;
#8705 = DIRECTION ( 'NONE',  ( -1.000000000000000000, -0.000000000000000000, 0.000000000000000000 ) ) ;
#8706 = AXIS2_PLACEMENT_3D ( 'NONE', #7198, #24487, #41218 ) ;
#8707 = DIRECTION ( 'NONE',  ( 0.000000000000000000, 0.000000000000000000, 1.000000000000000000 ) ) ;
#8708 = EDGE_LOOP ( 'NONE', ( #24426, #39673, #892, #1313 ) ) ;
#8709 = AXIS2_PLACEMENT_3D ( 'NONE', #11642, #23508, #5068 ) ;
#8710 = ADVANCED_FACE ( 'NONE', ( #1398 ), #24799, .F. ) ;
#8711 = EDGE_LOOP ( 'NONE', ( #37111, #40231, #37215, #21577 ) ) ;
#8712 = CARTESIAN_POINT ( 'NONE',  ( -10.00000000000000000, 0.000000000000000000, 0.000000000000000000 ) ) ;
#8713 = VERTEX_POINT ( 'NONE', #34792 ) ;
#8714 = AXIS2_PLACEMENT_3D ( 'NONE', #580, #23544, #7348 ) ;
#8715 = DIRECTION ( 'NONE',  ( -1.000000000000000000, -0.000000000000000000, -0.000000000000000000 ) ) ;
#8716 = DIRECTION ( 'NONE',  ( 1.000000000000000000, 0.000000000000000000, 0.000000000000000000 ) ) ;
#8717 = EDGE_CURVE ( 'NONE', #9333, #16003, #15497, .T. ) ;
#8718 = CIRCLE ( 'NONE', #24107, 116.0000000000000000 ) ;
#8719 = DIRECTION ( 'NONE',  ( -1.000000000000000000, 0.000000000000000000, -0.000000000000000000 ) ) ;
#8720 = CARTESIAN_POINT ( 'NONE',  ( 0.000000000000000000, 115.0622509503834578, -14.72000021165029082 ) ) ;
#8721 = ORIENTED_EDGE ( 'NONE', *, *, #40675, .T. ) ;
#8722 = CARTESIAN_POINT ( 'NONE',  ( 18.00000000000000355, 27.79676263918187118, 37.88001506494779846 ) ) ;
#8724 = VERTEX_POINT ( 'NONE', #19900 ) ;
#8723 = AXIS2_PLACEMENT_3D ( 'NONE', #22805, #26269, #3728 ) ;
#8725 = FACE_OUTER_BOUND ( 'NONE', #25213, .T. ) ;
#8726 = EDGE_LOOP ( 'NONE', ( #27054, #14687 ) ) ;
#8727 = DIRECTION ( 'NONE',  ( 0.000000000000000000, 0.4132121857683791477, -0.9106347728549126774 ) ) ;
#8728 = DIRECTION ( 'NONE',  ( -1.000000000000000000, 0.000000000000000000, -0.000000000000000000 ) ) ;
#8729 = APPLICATION_PROTOCOL_DEFINITION ( 'draft international standard', 'automotive_design', 1998, #40067 ) ;
#8730 = DIRECTION ( 'NONE',  ( 0.000000000000000000, 0.000000000000000000, -1.000000000000000000 ) ) ;
#8731 = CARTESIAN_POINT ( 'NONE',  ( 12.21457428495364006, 31.00000000000000355, 45.57612047952555656 ) ) ;
#8732 = ORIENTED_EDGE ( 'NONE', *, *, #42266, .F. ) ;
#8733 = CARTESIAN_POINT ( 'NONE',  ( 0.000000000000000000, 0.000000000000000000, 0.000000000000000000 ) ) ;
#8734 = EDGE_CURVE ( 'NONE', #5484, #27946, #16637, .T. ) ;
#8735 = EDGE_CURVE ( 'NONE', #16446, #1738, #9876, .T. ) ;
#8737 = EDGE_LOOP ( 'NONE', ( #22044, #6398, #5795, #18832 ) ) ;
#8736 = CIRCLE ( 'NONE', #40760, 20.00000000000000711 ) ;
#8738 = ADVANCED_FACE ( 'NONE', ( #25801 ), #36422, .T. ) ;
#8739 = EDGE_CURVE ( 'NONE', #28542, #16567, #5001, .T. ) ;
#8740 = CIRCLE ( 'NONE', #1057, 13.59999999999999787 ) ;
#8741 = CARTESIAN_POINT ( 'NONE',  ( -59.89583333444493718, 40.00000000000000711, 3.926990808566372060 ) ) ;
#8742 = AXIS2_PLACEMENT_3D ( 'NONE', #23850, #17975, #31245 ) ;
#8743 = EDGE_CURVE ( 'NONE', #19682, #8854, #23840, .T. ) ;
#8744 = CIRCLE ( 'NONE', #29661, 13.59999999999999964 ) ;
#8745 = DIRECTION ( 'NONE',  ( 1.000000000000000000, 0.000000000000000000, 0.000000000000000000 ) ) ;
#8746 = AXIS2_PLACEMENT_3D ( 'NONE', #12823, #15899, #107 ) ;
#8747 = CARTESIAN_POINT ( 'NONE',  ( 17.99999999999999645, -12.43843445475394027, 111.5058645182329116 ) ) ;
#8748 = AXIS2_PLACEMENT_3D ( 'NONE', #23366, #20114, #28682 ) ;
#8749 = EDGE_CURVE ( 'NONE', #36535, #16214, #13343, .T. ) ;
#8750 = DIRECTION ( 'NONE',  ( 0.000000000000000000, 0.7164567402983115230, 0.6976315211349884970 ) ) ;
#8751 = DIRECTION ( 'NONE',  ( 1.000000000000000000, 0.000000000000000000, -0.000000000000000000 ) ) ;
#8752 = AXIS2_PLACEMENT_3D ( 'NONE', #5333, #28697, #41963 ) ;
#8753 = ORIENTED_EDGE ( 'NONE', *, *, #6450, .F. ) ;
#8754 = CARTESIAN_POINT ( 'NONE',  ( 34.28525303991722240, 40.00000000000000000, 9.176237600273646322 ) ) ;
#8755 = ORIENTED_EDGE ( 'NONE', *, *, #27028, .F. ) ;
#8756 = CARTESIAN_POINT ( 'NONE',  ( -1.600000000000000089, -12.75000000000000000, 0.000000000000000000 ) ) ;
#8757 = DIRECTION ( 'NONE',  ( 1.000000000000000000, 0.000000000000000000, 0.000000000000000000 ) ) ;
#8758 = ORIENTED_EDGE ( 'NONE', *, *, #22540, .T. ) ;
#8759 = CYLINDRICAL_SURFACE ( 'NONE', #25688, 20.00000000000000711 ) ;
#8760 = ORIENTED_EDGE ( 'NONE', *, *, #32430, .T. ) ;
#8761 = CARTESIAN_POINT ( 'NONE',  ( 17.99999999999999645, 29.36437154452156761, -116.8684075565133043 ) ) ;
#8762 = ORIENTED_EDGE ( 'NONE', *, *, #8187, .T. ) ;
#8763 = ORIENTED_EDGE ( 'NONE', *, *, #38033, .T. ) ;
#8764 = LINE ( 'NONE', #28645, #7641 ) ;
#8765 = CARTESIAN_POINT ( 'NONE',  ( 27.50146173783093317, 31.00000000000000355, -80.63904244945182143 ) ) ;
#8766 = ORIENTED_EDGE ( 'NONE', *, *, #39699, .T. ) ;
#8767 = LINE ( 'NONE', #22336, #18257 ) ;
#8768 = VECTOR ( 'NONE', #2893, 1000.000000000000000 ) ;
#8770 = CARTESIAN_POINT ( 'NONE',  ( 17.99999999999999645, -110.1579703617964725, -21.29539948940357164 ) ) ;
#8769 = AXIS2_PLACEMENT_3D ( 'NONE', #40735, #20953, #4088 ) ;
#8771 = ORIENTED_EDGE ( 'NONE', *, *, #3851, .T. ) ;
#8772 = AXIS2_PLACEMENT_3D ( 'NONE', #7563, #21353, #24403 ) ;
#8773 = CARTESIAN_POINT ( 'NONE',  ( -58.65872368235312706, -2.055254544495720648, -38.66963954070958209 ) ) ;
#8774 = CARTESIAN_POINT ( 'NONE',  ( -76.05825820879898913, 40.00000000000000711, 66.55365856249082412 ) ) ;
#8775 = VECTOR ( 'NONE', #8799, 1000.000000000000000 ) ;
#8776 = CARTESIAN_POINT ( 'NONE',  ( -9.709369018688816411, 31.00000000000000355, 28.47525938324675820 ) ) ;
#8777 = CIRCLE ( 'NONE', #4596, 120.5010000000000190 ) ;
#8779 = CARTESIAN_POINT ( 'NONE',  ( 18.00000000000000355, 0.2227391519116599106, 46.98410307550730636 ) ) ;
#8778 = DIRECTION ( 'NONE',  ( -1.000000000000000000, 0.000000000000000000, -0.000000000000000000 ) ) ;
#8780 = CIRCLE ( 'NONE', #26234, 36.00000000000000000 ) ;
#8781 = VECTOR ( 'NONE', #26442, 1000.000000000000000 ) ;
#8782 = DIRECTION ( 'NONE',  ( 0.000000000000000000, 0.1837495178165637066, 0.9829730996839030066 ) ) ;
#8783 = CARTESIAN_POINT ( 'NONE',  ( 0.000000000000000000, 7.749090474611513457, 30.53094492177216068 ) ) ;
#8784 = ORIENTED_EDGE ( 'NONE', *, *, #29913, .F. ) ;
#8785 = VECTOR ( 'NONE', #9343, 1000.000000000000000 ) ;
#8786 =( NAMED_UNIT ( * ) PLANE_ANGLE_UNIT ( ) SI_UNIT ( $, .RADIAN. ) );
#8787 = ORIENTED_EDGE ( 'NONE', *, *, #11673, .T. ) ;
#8788 = LINE ( 'NONE', #21724, #28935 ) ;
#8789 = CARTESIAN_POINT ( 'NONE',  ( 57.05379307149791401, 31.00000000000000000, -74.37948018729004218 ) ) ;
#8790 = CARTESIAN_POINT ( 'NONE',  ( 0.000000000000000000, 0.000000000000000000, 0.000000000000000000 ) ) ;
#8791 = ORIENTED_EDGE ( 'NONE', *, *, #10999, .T. ) ;
#8792 = EDGE_CURVE ( 'NONE', #40190, #38713, #28012, .T. ) ;
#8793 = EDGE_CURVE ( 'NONE', #37085, #21443, #2617, .T. ) ;
#8794 = CARTESIAN_POINT ( 'NONE',  ( 24.21999397792122366, 40.00000000000000000, 8.216913396989165008 ) ) ;
#8795 = CARTESIAN_POINT ( 'NONE',  ( -24.93870012979089168, 40.00000000000000000, -21.94074674037796058 ) ) ;
#8796 = EDGE_CURVE ( 'NONE', #38324, #36435, #4292, .T. ) ;
#8797 = ORIENTED_EDGE ( 'NONE', *, *, #6474, .F. ) ;
#8798 = ORIENTED_EDGE ( 'NONE', *, *, #6450, .T. ) ;
#8799 = DIRECTION ( 'NONE',  ( -1.000000000000000000, -0.000000000000000000, -0.000000000000000000 ) ) ;
#8800 = CARTESIAN_POINT ( 'NONE',  ( -10.00000000000000000, 0.000000000000000000, 0.000000000000000000 ) ) ;
#8801 = CARTESIAN_POINT ( 'NONE',  ( 0.2500000000000002220, 0.000000000000000000, 0.000000000000000000 ) ) ;
#8802 = LINE ( 'NONE', #35418, #39298 ) ;
#8803 = CIRCLE ( 'NONE', #31114, 59.00000000000000711 ) ;
#8804 = EDGE_CURVE ( 'NONE', #27530, #40464, #12003, .T. ) ;
#8805 = CONICAL_SURFACE ( 'NONE', #37358, 5.560781378645573980, 1.221730476396046816 ) ;
#8806 = CYLINDRICAL_SURFACE ( 'NONE', #23714, 120.5010000000000190 ) ;
#8807 = VERTEX_POINT ( 'NONE', #26211 ) ;
#8808 = DIRECTION ( 'NONE',  ( 0.000000000000000000, 0.000000000000000000, 1.000000000000000000 ) ) ;
#8809 = EDGE_LOOP ( 'NONE', ( #25606, #615, #43086, #38960 ) ) ;
#8810 = LINE ( 'NONE', #35825, #35431 ) ;
#8811 = CARTESIAN_POINT ( 'NONE',  ( -10.00000000000000000, 0.000000000000000000, 0.000000000000000000 ) ) ;
#8812 = CIRCLE ( 'NONE', #37360, 59.00000000000000711 ) ;
#8813 = EDGE_CURVE ( 'NONE', #631, #22812, #39116, .T. ) ;
#8814 = CIRCLE ( 'NONE', #31816, 120.5010000000000332 ) ;
#8815 = CARTESIAN_POINT ( 'NONE',  ( 17.99999999999999645, 115.9750404417044081, -2.406240749597859718 ) ) ;
#8816 = FACE_OUTER_BOUND ( 'NONE', #38739, .T. ) ;
#8817 = ORIENTED_EDGE ( 'NONE', *, *, #27096, .T. ) ;
#8818 = ORIENTED_EDGE ( 'NONE', *, *, #18157, .F. ) ;
#8819 = CARTESIAN_POINT ( 'NONE',  ( 17.99999999999999645, -30.01658535635337444, 108.1077105353196970 ) ) ;
#8820 = AXIS2_PLACEMENT_3D ( 'NONE', #15657, #12592, #19379 ) ;
#8821 = VERTEX_POINT ( 'NONE', #19257 ) ;
#8823 = VERTEX_POINT ( 'NONE', #42540 ) ;
#8822 = FACE_OUTER_BOUND ( 'NONE', #32539, .T. ) ;
#8824 = CARTESIAN_POINT ( 'NONE',  ( 29.31577600746836154, 31.00000000000000355, 50.95836110721448620 ) ) ;
#8825 = ORIENTED_EDGE ( 'NONE', *, *, #30741, .T. ) ;
#8826 = CYLINDRICAL_SURFACE ( 'NONE', #16108, 31.49899999999999878 ) ;
#8827 = CIRCLE ( 'NONE', #3218, 0.08402000000000062196 ) ;
#8828 = ADVANCED_FACE ( 'NONE', ( #12690 ), #19473, .F. ) ;
#8829 = DIRECTION ( 'NONE',  ( 0.000000000000000000, 0.000000000000000000, 1.000000000000000000 ) ) ;
#8830 = ORIENTED_EDGE ( 'NONE', *, *, #24249, .T. ) ;
#8831 = CARTESIAN_POINT ( 'NONE',  ( 4.991138515316659863, 40.00000000000000000, -74.59332054773635434 ) ) ;
#8832 = VECTOR ( 'NONE', #37668, 1000.000000000000000 ) ;
#8834 = CARTESIAN_POINT ( 'NONE',  ( 0.000000000000000000, -24.72041153920759271, 40.55929306992679528 ) ) ;
#8833 = DIRECTION ( 'NONE',  ( -1.000000000000000000, -0.000000000000000000, -0.000000000000000000 ) ) ;
#8835 = LINE ( 'NONE', #12347, #19238 ) ;
#8836 = EDGE_LOOP ( 'NONE', ( #7431, #6903, #10664, #39928 ) ) ;
#8837 = LINE ( 'NONE', #25673, #32824 ) ;
#8838 = CIRCLE ( 'NONE', #24932, 12.55910585664918422 ) ;
#8839 = EDGE_LOOP ( 'NONE', ( #40459, #2721, #35422, #10366 ) ) ;
#8840 = VECTOR ( 'NONE', #2807, 1000.000000000000000 ) ;
#8841 = DIRECTION ( 'NONE',  ( -1.000000000000000000, -0.000000000000000000, -0.000000000000000000 ) ) ;
#8842 = DIRECTION ( 'NONE',  ( 0.000000000000000000, 0.000000000000000000, -1.000000000000000000 ) ) ;
#8843 = AXIS2_PLACEMENT_3D ( 'NONE', #23076, #12798, #13024 ) ;
#8844 = CARTESIAN_POINT ( 'NONE',  ( 64.78932475141161262, 31.00000000000000000, 8.528958657501300777 ) ) ;
#8846 = CARTESIAN_POINT ( 'NONE',  ( 17.99999999999999645, -59.47573314508800735, 99.59235496188593117 ) ) ;
#8845 = DIRECTION ( 'NONE',  ( 1.000000000000000000, 0.000000000000000000, 0.000000000000000000 ) ) ;
#8848 = ORIENTED_EDGE ( 'NONE', *, *, #8666, .F. ) ;
#8847 = COLOUR_RGB ( '', 0.72549020, 0.75294118, 0.79215686) ;
#8849 = EDGE_CURVE ( 'NONE', #4662, #10112, #20354, .T. ) ;
#8850 = EDGE_CURVE ( 'NONE', #21953, #6529, #6387, .T. ) ;
#8852 = CIRCLE ( 'NONE', #3240, 2.649999999999987477 ) ;
#8851 = DIRECTION ( 'NONE',  ( -1.000000000000000000, -0.000000000000000000, 0.000000000000000000 ) ) ;
#8853 = AXIS2_PLACEMENT_3D ( 'NONE', #38926, #39335, #22400 ) ;
#8854 = VERTEX_POINT ( 'NONE', #35998 ) ;
#8855 = CARTESIAN_POINT ( 'NONE',  ( 17.99999999999999645, 46.83041522348636931, -101.9567785075596618 ) ) ;
#8856 = CARTESIAN_POINT ( 'NONE',  ( 18.00000000000000355, -42.60732521687558005, -19.80331771201703006 ) ) ;
#8857 = CARTESIAN_POINT ( 'NONE',  ( -88.68107738130200346, 31.00000000000000711, 23.63280646692842524 ) ) ;
#8858 = CARTESIAN_POINT ( 'NONE',  ( 64.90225467577229779, 39.99999999999999289, 74.17428024387139374 ) ) ;
#8859 = EDGE_CURVE ( 'NONE', #41335, #15839, #22744, .T. ) ;
#8860 = DIRECTION ( 'NONE',  ( -1.000000000000000000, 0.000000000000000000, 0.000000000000000000 ) ) ;
#8861 = EDGE_CURVE ( 'NONE', #27302, #33525, #9622, .T. ) ;
#8862 = VERTEX_POINT ( 'NONE', #22968 ) ;
#8863 = CYLINDRICAL_SURFACE ( 'NONE', #13788, 116.0000000000000000 ) ;
#8864 = EDGE_LOOP ( 'NONE', ( #33847, #19282, #19456, #13647 ) ) ;
#8865 = PLANE ( 'NONE',  #10210 ) ;
#8866 = EDGE_CURVE ( 'NONE', #1655, #11213, #7072, .T. ) ;
#8867 = CIRCLE ( 'NONE', #40894, 116.0000000000000000 ) ;
#8869 = ORIENTED_EDGE ( 'NONE', *, *, #31908, .T. ) ;
#8868 = CARTESIAN_POINT ( 'NONE',  ( 8.999999999999998224, 106.6051926090971023, 45.73109345704855855 ) ) ;
#8870 = DIRECTION ( 'NONE',  ( 1.000000000000000000, 0.000000000000000000, 0.000000000000000000 ) ) ;
#8871 = ORIENTED_EDGE ( 'NONE', *, *, #37193, .T. ) ;
#8872 = CARTESIAN_POINT ( 'NONE',  ( 8.999999999999998224, 0.000000000000000000, 0.000000000000000000 ) ) ;
#8873 = AXIS2_PLACEMENT_3D ( 'NONE', #19246, #42322, #25788 ) ;
#8874 = CARTESIAN_POINT ( 'NONE',  ( 0.000000000000000000, 41.20225022064669673, -23.63323037071358357 ) ) ;
#8875 = CIRCLE ( 'NONE', #15873, 59.00000000000000000 ) ;
#8876 = CARTESIAN_POINT ( 'NONE',  ( 0.000000000000000000, 0.000000000000000000, 0.000000000000000000 ) ) ;
#8877 = AXIS2_PLACEMENT_3D ( 'NONE', #2282, #35468, #9068 ) ;
#8878 = AXIS2_PLACEMENT_3D ( 'NONE', #20889, #7525, #27618 ) ;
#8879 = ORIENTED_EDGE ( 'NONE', *, *, #36479, .F. ) ;
#8880 = CARTESIAN_POINT ( 'NONE',  ( 22.27703560431448793, 31.00000000000000355, 17.12883495622356023 ) ) ;
#8881 = FACE_OUTER_BOUND ( 'NONE', #29516, .T. ) ;
#8882 = CIRCLE ( 'NONE', #33263, 59.00000000000000000 ) ;
#8883 = AXIS2_PLACEMENT_3D ( 'NONE', #1102, #34070, #18186 ) ;
#8884 = EDGE_CURVE ( 'NONE', #8807, #38409, #16168, .T. ) ;
#8886 = VERTEX_POINT ( 'NONE', #23818 ) ;
#8885 = FACE_OUTER_BOUND ( 'NONE', #35224, .T. ) ;
#8887 = ORIENTED_EDGE ( 'NONE', *, *, #37368, .T. ) ;
#8888 = CARTESIAN_POINT ( 'NONE',  ( 9.000000000000001776, -63.55543939553702160, -97.03971415477388973 ) ) ;
#8889 = EDGE_CURVE ( 'NONE', #2710, #42617, #16849, .T. ) ;
#8890 = CARTESIAN_POINT ( 'NONE',  ( 17.99999999999999645, -30.74337109795213863, -8.695908345466433431 ) ) ;
#8891 = CARTESIAN_POINT ( 'NONE',  ( -41.89947471387619515, 40.00000000000000000, 2.670153906482984230 ) ) ;
#8892 = CYLINDRICAL_SURFACE ( 'NONE', #29242, 59.00000000000001421 ) ;
#8893 = EDGE_CURVE ( 'NONE', #36084, #16529, #17592, .T. ) ;
#8894 = CARTESIAN_POINT ( 'NONE',  ( 0.000000000000000000, -8.053585752061598768, -46.81126742072031988 ) ) ;
#8895 = CARTESIAN_POINT ( 'NONE',  ( 2.500000000000000000, 0.000000000000000000, 0.000000000000000000 ) ) ;
#8896 = ORIENTED_EDGE ( 'NONE', *, *, #36085, .T. ) ;
#8897 = CARTESIAN_POINT ( 'NONE',  ( 18.00000000000000355, 0.000000000000000000, 0.000000000000000000 ) ) ;
#8898 = ORIENTED_EDGE ( 'NONE', *, *, #26928, .F. ) ;
#8899 = CARTESIAN_POINT ( 'NONE',  ( 0.000000000000000000, -31.17727234463771424, 111.7317219465818852 ) ) ;
#8900 = CYLINDRICAL_SURFACE ( 'NONE', #4531, 59.00000000000000000 ) ;
#8901 = CARTESIAN_POINT ( 'NONE',  ( 29.64712525329720449, 31.00000000000000355, -17.12831674356021239 ) ) ;
#8902 = ORIENTED_EDGE ( 'NONE', *, *, #28716, .F. ) ;
#8903 = CARTESIAN_POINT ( 'NONE',  ( -99.91857577502598531, 31.00000000000000355, -1.280628618496984616 ) ) ;
#8904 = VERTEX_POINT ( 'NONE', #24475 ) ;
#8905 = VECTOR ( 'NONE', #17273, 1000.000000000000000 ) ;
#8906 = EDGE_CURVE ( 'NONE', #714, #5010, #14091, .T. ) ;
#8907 = AXIS2_PLACEMENT_3D ( 'NONE', #20697, #37443, #27655 ) ;
#8908 = CARTESIAN_POINT ( 'NONE',  ( 17.99999999999999645, 119.0898412705476943, -18.38751498043618682 ) ) ;
#8909 = CARTESIAN_POINT ( 'NONE',  ( 85.10416666585589951, 31.00000000000000000, 5.563236982362346872 ) ) ;
#8910 = VECTOR ( 'NONE', #26877, 1000.000000000000000 ) ;
#8911 = CIRCLE ( 'NONE', #15244, 47.49900000000000233 ) ;
#8912 = CYLINDRICAL_SURFACE ( 'NONE', #17853, 1.000000000000000666 ) ;
#8913 = VERTEX_POINT ( 'NONE', #24261 ) ;
#8915 = CARTESIAN_POINT ( 'NONE',  ( 54.55067978551168295, 31.00000000000000355, 18.62288743479739139 ) ) ;
#8914 = AXIS2_PLACEMENT_3D ( 'NONE', #11624, #28207, #17760 ) ;
#8916 = CARTESIAN_POINT ( 'NONE',  ( 74.70319961851696178, 39.99999999999999289, -57.31929289364909152 ) ) ;
#8917 = EDGE_CURVE ( 'NONE', #14512, #5171, #41922, .T. ) ;
#8918 = VERTEX_POINT ( 'NONE', #7417 ) ;
#8919 = PLANE ( 'NONE',  #35283 ) ;
#8920 = AXIS2_PLACEMENT_3D ( 'NONE', #8667, #2306, #18770 ) ;
#8921 = FACE_OUTER_BOUND ( 'NONE', #36499, .T. ) ;
#8922 = DIRECTION ( 'NONE',  ( 0.000000000000000000, 0.000000000000000000, -1.000000000000000000 ) ) ;
#8924 = ORIENTED_EDGE ( 'NONE', *, *, #32091, .F. ) ;
#8923 = DIRECTION ( 'NONE',  ( -1.000000000000000000, -0.000000000000000000, -0.000000000000000000 ) ) ;
#8925 = ADVANCED_FACE ( 'NONE', ( #17286 ), #30982, .T. ) ;
#8926 = FACE_OUTER_BOUND ( 'NONE', #17684, .T. ) ;
#8927 = DIRECTION ( 'NONE',  ( 1.000000000000000000, 0.000000000000000000, 0.000000000000000000 ) ) ;
#8928 = ORIENTED_EDGE ( 'NONE', *, *, #878, .F. ) ;
#8929 = CARTESIAN_POINT ( 'NONE',  ( -61.47519263390311295, 40.00000000000000711, -35.49250405581909007 ) ) ;
#8930 = FACE_OUTER_BOUND ( 'NONE', #25854, .T. ) ;
#8931 = ORIENTED_EDGE ( 'NONE', *, *, #37193, .F. ) ;
#8932 = AXIS2_PLACEMENT_3D ( 'NONE', #5901, #11849, #25174 ) ;
#8933 = LINE ( 'NONE', #32060, #8517 ) ;
#8934 = EDGE_LOOP ( 'NONE', ( #30293, #11117, #41429, #14201 ) ) ;
#8935 = AXIS2_PLACEMENT_3D ( 'NONE', #16331, #22686, #39848 ) ;
#8936 = AXIS2_PLACEMENT_3D ( 'NONE', #38728, #14785, #28085 ) ;
#8937 = VERTEX_POINT ( 'NONE', #7630 ) ;
#8938 = LINE ( 'NONE', #25761, #40668 ) ;
#8940 = ORIENTED_EDGE ( 'NONE', *, *, #42636, .F. ) ;
#8939 = ADVANCED_FACE ( 'NONE', ( #20994 ), #7828, .F. ) ;
#8941 = AXIS2_PLACEMENT_3D ( 'NONE', #30182, #36477, #33232 ) ;
#8942 = FACE_OUTER_BOUND ( 'NONE', #5937, .T. ) ;
#8943 = DIRECTION ( 'NONE',  ( 0.000000000000000000, -0.6783118362696222148, 0.7347741508630615259 ) ) ;
#8944 = EDGE_CURVE ( 'NONE', #1122, #31468, #14421, .T. ) ;
#8945 = CARTESIAN_POINT ( 'NONE',  ( 17.99999999999999645, -68.63002662989681824, -93.51962064069581970 ) ) ;
#8946 = CARTESIAN_POINT ( 'NONE',  ( 0.000000000000000000, -119.7318547011700502, -13.59315897125848238 ) ) ;
#8947 = ORIENTED_EDGE ( 'NONE', *, *, #5829, .T. ) ;
#8948 = DIRECTION ( 'NONE',  ( 0.000000000000000000, -0.3612416661871603596, 0.9324722294043529258 ) ) ;
#8949 = EDGE_LOOP ( 'NONE', ( #7447, #6847, #42498, #30414, #33820 ) ) ;
#8950 = CARTESIAN_POINT ( 'NONE',  ( 8.999999999999998224, 42.87700105098606684, 107.7847984684006377 ) ) ;
#8951 = ORIENTED_EDGE ( 'NONE', *, *, #39652, .F. ) ;
#8952 = DIRECTION ( 'NONE',  ( 0.000000000000000000, 0.000000000000000000, -1.000000000000000000 ) ) ;
#8953 = DIRECTION ( 'NONE',  ( 1.000000000000000000, 0.000000000000000000, 0.000000000000000000 ) ) ;
#8954 = DIRECTION ( 'NONE',  ( -4.329780281177489232E-17, 1.000000000000000000, -4.329780281177443626E-17 ) ) ;
#8955 = EDGE_CURVE ( 'NONE', #25103, #28038, #9195, .T. ) ;
#8956 = CARTESIAN_POINT ( 'NONE',  ( -10.00000000000000000, 0.000000000000000000, 0.000000000000000000 ) ) ;
#8957 = CARTESIAN_POINT ( 'NONE',  ( 38.75409931461306456, 31.00000000000000355, -50.52625141960567134 ) ) ;
#8958 = ORIENTED_EDGE ( 'NONE', *, *, #7648, .F. ) ;
#8959 = CARTESIAN_POINT ( 'NONE',  ( 0.000000000000000000, 30.78424799127067502, 6.672111855473287001 ) ) ;
#8960 = CIRCLE ( 'NONE', #9672, 19.19999999999999574 ) ;
#8961 = ORIENTED_EDGE ( 'NONE', *, *, #21888, .F. ) ;
#8962 = AXIS2_PLACEMENT_3D ( 'NONE', #13084, #35945, #23333 ) ;
#8963 = CARTESIAN_POINT ( 'NONE',  ( -37.49462465745612860, 40.00000000000000000, -48.86220178749748300 ) ) ;
#8964 = AXIS2_PLACEMENT_3D ( 'NONE', #3517, #17106, #679 ) ;
#8965 = EDGE_CURVE ( 'NONE', #2475, #25511, #3594, .T. ) ;
#8966 = CARTESIAN_POINT ( 'NONE',  ( 0.000000000000000000, 29.36437154452156761, -116.8684075565133043 ) ) ;
#8967 = FACE_OUTER_BOUND ( 'NONE', #23309, .T. ) ;
#8968 = EDGE_CURVE ( 'NONE', #2829, #34305, #33815, .T. ) ;
#8969 = CARTESIAN_POINT ( 'NONE',  ( -6.999999999999999112, 4.546351088565595293E-15, 0.000000000000000000 ) ) ;
#8970 = DIRECTION ( 'NONE',  ( 0.000000000000000000, 0.000000000000000000, 1.000000000000000000 ) ) ;
#8971 = VERTEX_POINT ( 'NONE', #30130 ) ;
#8972 = CARTESIAN_POINT ( 'NONE',  ( 18.38119342899891961, 40.00000000000000000, 31.81670425098764099 ) ) ;
#8973 = ORIENTED_EDGE ( 'NONE', *, *, #36026, .T. ) ;
#8974 = CARTESIAN_POINT ( 'NONE',  ( -75.96080130434582145, -12.05525454449572109, 14.45886780445738218 ) ) ;
#8975 = DIRECTION ( 'NONE',  ( -1.000000000000000000, -0.000000000000000000, -0.000000000000000000 ) ) ;
#8976 = ORIENTED_EDGE ( 'NONE', *, *, #32064, .F. ) ;
#8977 = CARTESIAN_POINT ( 'NONE',  ( 18.00000000000000355, -11.46872990052349550, -45.56340405422456286 ) ) ;
#8978 = ORIENTED_EDGE ( 'NONE', *, *, #12353, .T. ) ;
#8979 = CARTESIAN_POINT ( 'NONE',  ( 17.99999999999999645, -97.97378550988183576, -62.10585602713859288 ) ) ;
#8980 = VERTEX_POINT ( 'NONE', #187 ) ;
#8981 = ORIENTED_EDGE ( 'NONE', *, *, #43083, .T. ) ;
#8982 = CARTESIAN_POINT ( 'NONE',  ( 18.00000000000000355, 2.123073309835184386, 47.45152853935334747 ) ) ;
#8983 = ADVANCED_FACE ( 'NONE', ( #7186 ), #13555, .F. ) ;
#8984 = CARTESIAN_POINT ( 'NONE',  ( -49.21613380539480431, 31.00000000000000355, 63.96793098899347996 ) ) ;
#8985 = ORIENTED_EDGE ( 'NONE', *, *, #17797, .T. ) ;
#8986 = DIRECTION ( 'NONE',  ( 1.000000000000000000, 0.000000000000000000, 0.000000000000000000 ) ) ;
#8988 = EDGE_CURVE ( 'NONE', #5335, #25212, #37068, .T. ) ;
#8987 = CIRCLE ( 'NONE', #33369, 15.08402000000000065 ) ;
#8989 = AXIS2_PLACEMENT_3D ( 'NONE', #15256, #28329, #22435 ) ;
#8990 = ADVANCED_FACE ( 'NONE', ( #10261 ), #13778, .F. ) ;
#8991 = ADVANCED_FACE ( 'NONE', ( #20335 ), #27500, .F. ) ;
#8992 = CARTESIAN_POINT ( 'NONE',  ( 18.00000000000000355, 0.000000000000000000, 0.000000000000000000 ) ) ;
#8993 = CIRCLE ( 'NONE', #16692, 139.5000000000000000 ) ;
#8994 = ORIENTED_EDGE ( 'NONE', *, *, #9326, .T. ) ;
#8995 = DIRECTION ( 'NONE',  ( 0.000000000000000000, -0.5264321628773447337, -0.8502171357296209875 ) ) ;
#8996 = CARTESIAN_POINT ( 'NONE',  ( 17.99999999999999645, 2.007101075700415738, -31.43498920425966858 ) ) ;
#8997 = CARTESIAN_POINT ( 'NONE',  ( -96.33078216555149709, 40.00000000000000711, 32.58251675340183340 ) ) ;
#8999 = DIRECTION ( 'NONE',  ( 1.000000000000000000, 0.000000000000000000, 0.000000000000000000 ) ) ;
#8998 = FACE_BOUND ( 'NONE', #32392, .T. ) ;
#9000 = DIRECTION ( 'NONE',  ( 0.000000000000000000, -0.9510565162951500895, -0.3090169943749582204 ) ) ;
#9001 = CARTESIAN_POINT ( 'NONE',  ( 0.000000000000000000, 0.000000000000000000, 0.000000000000000000 ) ) ;
#9002 = ORIENTED_EDGE ( 'NONE', *, *, #24578, .T. ) ;
#9003 = CARTESIAN_POINT ( 'NONE',  ( 17.99999999999999645, 45.89132998248050654, 102.3829004574631512 ) ) ;
#9004 = VERTEX_POINT ( 'NONE', #37083 ) ;
#9005 = CARTESIAN_POINT ( 'NONE',  ( 17.99999999999999645, 0.000000000000000000, 0.000000000000000000 ) ) ;
#9006 = CARTESIAN_POINT ( 'NONE',  ( 17.99999999999999645, -72.00556975657760006, 86.04342158279364128 ) ) ;
#9007 = ORIENTED_EDGE ( 'NONE', *, *, #21166, .F. ) ;
#9008 = CARTESIAN_POINT ( 'NONE',  ( 20.45440555730427690, 40.00000000000000000, -26.67302265141799467 ) ) ;
#9009 = CARTESIAN_POINT ( 'NONE',  ( -20.27214883179920690, 40.00000000000000000, 34.96734655410256210 ) ) ;
#9010 = ORIENTED_EDGE ( 'NONE', *, *, #6756, .T. ) ;
#9011 = ORIENTED_EDGE ( 'NONE', *, *, #31609, .F. ) ;
#9012 = CARTESIAN_POINT ( 'NONE',  ( 18.00000000000000355, -41.20225022064620646, -23.63323037071445043 ) ) ;
#9013 = DIRECTION ( 'NONE',  ( -1.000000000000000000, -0.000000000000000000, 0.000000000000000000 ) ) ;
#9014 = EDGE_CURVE ( 'NONE', #32794, #35367, #4125, .T. ) ;
#9015 = VECTOR ( 'NONE', #15144, 1000.000000000000000 ) ;
#9016 = CARTESIAN_POINT ( 'NONE',  ( 0.000000000000000000, -41.60679253225688967, -108.2814610871950265 ) ) ;
#9017 = CARTESIAN_POINT ( 'NONE',  ( 1.598609366639573350E-14, -1.063425437509180407E-13, -40.00000000000000000 ) ) ;
#9018 = DIRECTION ( 'NONE',  ( -1.000000000000000000, 0.000000000000000000, 0.000000000000000000 ) ) ;
#9019 = ORIENTED_EDGE ( 'NONE', *, *, #20810, .T. ) ;
#9020 = CARTESIAN_POINT ( 'NONE',  ( 17.99999999999999645, 0.000000000000000000, 0.000000000000000000 ) ) ;
#9021 = VERTEX_POINT ( 'NONE', #40345 ) ;
#9022 = DIRECTION ( 'NONE',  ( 1.000000000000000000, 0.000000000000000000, 0.000000000000000000 ) ) ;
#9023 = PLANE ( 'NONE',  #6101 ) ;
#9024 = CARTESIAN_POINT ( 'NONE',  ( 17.99999999999999645, -119.0898412705473532, -18.38751498043852806 ) ) ;
#9025 = CYLINDRICAL_SURFACE ( 'NONE', #37987, 20.00000000000001066 ) ;
#9026 = SHAPE_REPRESENTATION ( 'housing right', ( #13552 ), #31631 ) ;
#9027 = VERTEX_POINT ( 'NONE', #40774 ) ;
#9028 = CARTESIAN_POINT ( 'NONE',  ( -60.10374203099167545, 40.00000000000000711, 78.35501831527777483 ) ) ;
#9029 = ORIENTED_EDGE ( 'NONE', *, *, #7774, .F. ) ;
#9030 = DIRECTION ( 'NONE',  ( 0.000000000000000000, 0.000000000000000000, 1.000000000000000000 ) ) ;
#9031 = EDGE_LOOP ( 'NONE', ( #7708, #33134, #31158, #602 ) ) ;
#9033 = ORIENTED_EDGE ( 'NONE', *, *, #23835, .T. ) ;
#9032 = DIRECTION ( 'NONE',  ( -1.000000000000000000, 0.000000000000000000, -0.000000000000000000 ) ) ;
#9034 = CARTESIAN_POINT ( 'NONE',  ( 25.95756378415329024, 31.00000000000000355, 52.86556711865710412 ) ) ;
#9035 = EDGE_LOOP ( 'NONE', ( #8293, #8349 ) ) ;
#9036 = CARTESIAN_POINT ( 'NONE',  ( 17.99999999999999645, 0.000000000000000000, 0.000000000000000000 ) ) ;
#9037 = EDGE_CURVE ( 'NONE', #22117, #28268, #8933, .T. ) ;
#9038 = EDGE_CURVE ( 'NONE', #3997, #15479, #5011, .T. ) ;
#9039 = FACE_BOUND ( 'NONE', #21670, .T. ) ;
#9040 = EDGE_CURVE ( 'NONE', #18339, #26486, #20383, .T. ) ;
#9041 = ORIENTED_EDGE ( 'NONE', *, *, #33568, .F. ) ;
#9042 = CARTESIAN_POINT ( 'NONE',  ( 68.60033760563641181, 39.99999999999999289, -33.70054013428169526 ) ) ;
#9043 = CIRCLE ( 'NONE', #41775, 13.59999999999999964 ) ;
#9044 = AXIS2_PLACEMENT_3D ( 'NONE', #23960, #575, #40700 ) ;
#9045 = VECTOR ( 'NONE', #37091, 1000.000000000000000 ) ;
#9047 = DIRECTION ( 'NONE',  ( -3.009274222672345096E-17, -1.000000000000000000, 2.455023325076455345E-18 ) ) ;
#9046 = CARTESIAN_POINT ( 'NONE',  ( 0.000000000000000000, -97.97378550988183576, -62.10585602713859288 ) ) ;
#9048 = CARTESIAN_POINT ( 'NONE',  ( 0.000000000000000000, 52.19040376560434424, 99.31985817764196156 ) ) ;
#9049 = VERTEX_POINT ( 'NONE', #22283 ) ;
#9050 = LINE ( 'NONE', #5567, #36302 ) ;
#9051 = VERTEX_POINT ( 'NONE', #35324 ) ;
#9052 = SURFACE_STYLE_USAGE ( .BOTH. , #2690 ) ;
#9053 = CARTESIAN_POINT ( 'NONE',  ( 17.99999999999999645, 35.78484819117633720, 110.3423972910434117 ) ) ;
#9054 = CARTESIAN_POINT ( 'NONE',  ( 18.00000000000000355, 17.08890430202814059, -43.76671000081927332 ) ) ;
#9055 = EDGE_CURVE ( 'NONE', #30408, #19972, #2228, .T. ) ;
#9056 = CARTESIAN_POINT ( 'NONE',  ( 43.85342918759069164, 31.00000000000000355, 49.98553323097543455 ) ) ;
#9058 = CARTESIAN_POINT ( 'NONE',  ( -4.211140560182196957, -2.431303136016552013, -3.745885042887436178 ) ) ;
#9057 = DIRECTION ( 'NONE',  ( -1.000000000000000000, 0.000000000000000000, -0.000000000000000000 ) ) ;
#9059 = ORIENTED_EDGE ( 'NONE', *, *, #19150, .T. ) ;
#9060 = DIRECTION ( 'NONE',  ( -1.000000000000000000, 0.000000000000000000, -0.000000000000000000 ) ) ;
#9061 = EDGE_LOOP ( 'NONE', ( #35833, #29009, #17004, #27873 ) ) ;
#9062 = CARTESIAN_POINT ( 'NONE',  ( 18.00000000000000355, 32.00046193115148441, 34.40241257139697950 ) ) ;
#9063 = DIRECTION ( 'NONE',  ( -1.058513553088275437E-16, -1.000000000000000000, 8.813324511995299047E-17 ) ) ;
#9064 = CARTESIAN_POINT ( 'NONE',  ( 31.77777543000702565, 31.00000000000000355, 93.95825142778512884 ) ) ;
#9065 = CARTESIAN_POINT ( 'NONE',  ( 96.17895579825814423, 39.99999999999999289, -12.55124642863780338 ) ) ;
#9066 = CARTESIAN_POINT ( 'NONE',  ( 17.99999999999999645, -107.2885202478262698, -54.86040852957422942 ) ) ;
#9067 = ORIENTED_EDGE ( 'NONE', *, *, #40856, .T. ) ;
#9068 = DIRECTION ( 'NONE',  ( 0.000000000000000000, -0.4610925014493325591, 0.8873520750565681015 ) ) ;
#9069 = ORIENTED_EDGE ( 'NONE', *, *, #12046, .T. ) ;
#9070 = CARTESIAN_POINT ( 'NONE',  ( 17.99999999999999645, 29.86146780999950323, 112.0905559814579675 ) ) ;
#9071 = CIRCLE ( 'NONE', #39723, 116.0000000000000000 ) ;
#9072 = AXIS2_PLACEMENT_3D ( 'NONE', #29235, #42504, #32272 ) ;
#9074 = ORIENTED_EDGE ( 'NONE', *, *, #7402, .T. ) ;
#9073 = FACE_BOUND ( 'NONE', #43129, .T. ) ;
#9075 = VECTOR ( 'NONE', #12007, 1000.000000000000000 ) ;
#9076 = CARTESIAN_POINT ( 'NONE',  ( 2.649999999999769873, 150.5000000000013642, 7.000000000000418332 ) ) ;
#9077 = ORIENTED_EDGE ( 'NONE', *, *, #26231, .T. ) ;
#9078 = DIRECTION ( 'NONE',  ( -1.000000000000000000, 0.000000000000000000, 0.000000000000000000 ) ) ;
#9079 = DIRECTION ( 'NONE',  ( 0.000000000000000000, 0.8951632913550634507, -0.4457383557765359217 ) ) ;
#9080 = CARTESIAN_POINT ( 'NONE',  ( -6.599999999999994316, 4.619827469794975478E-15, 0.000000000000000000 ) ) ;
#9081 = ORIENTED_EDGE ( 'NONE', *, *, #35297, .T. ) ;
#9082 = DIRECTION ( 'NONE',  ( 0.000000000000000000, 0.000000000000000000, 1.000000000000000000 ) ) ;
#9083 = DIRECTION ( 'NONE',  ( 0.000000000000000000, 0.000000000000000000, -1.000000000000000000 ) ) ;
#9084 = EDGE_CURVE ( 'NONE', #20639, #14493, #15507, .T. ) ;
#9086 = VERTEX_POINT ( 'NONE', #31856 ) ;
#9085 = CARTESIAN_POINT ( 'NONE',  ( 0.000000000000000000, 0.000000000000000000, 0.000000000000000000 ) ) ;
#9087 = ORIENTED_EDGE ( 'NONE', *, *, #31018, .F. ) ;
#9088 = CARTESIAN_POINT ( 'NONE',  ( 129.9999999999992042, 8.206338904687194424E-13, 369.6955262170047263 ) ) ;
#9089 = LINE ( 'NONE', #22445, #11302 ) ;
#9090 = CARTESIAN_POINT ( 'NONE',  ( 46.89968353242633015, 40.00000000000000000, -2.988513402017745069 ) ) ;
#9091 = CARTESIAN_POINT ( 'NONE',  ( 17.99999999999999645, -98.39501399267994941, 53.91376164787647696 ) ) ;
#9092 = CIRCLE ( 'NONE', #29322, 12.55910585664918422 ) ;
#9093 = ADVANCED_FACE ( 'NONE', ( #34682 ), #28155, .F. ) ;
#9094 = CYLINDRICAL_SURFACE ( 'NONE', #12399, 120.5010000000000190 ) ;
#9095 = FACE_OUTER_BOUND ( 'NONE', #14861, .T. ) ;
#9096 = AXIS2_PLACEMENT_3D ( 'NONE', #8897, #22250, #18977 ) ;
#9097 = EDGE_LOOP ( 'NONE', ( #39863, #5050, #912, #40998 ) ) ;
#9098 = CARTESIAN_POINT ( 'NONE',  ( 26.80287614962791309, -14.05525454449571754, 69.29271901957253021 ) ) ;
#9099 = EDGE_CURVE ( 'NONE', #25078, #40994, #28594, .T. ) ;
#9100 = ORIENTED_EDGE ( 'NONE', *, *, #18220, .T. ) ;
#9101 = AXIS2_PLACEMENT_3D ( 'NONE', #22236, #35273, #18964 ) ;
#9102 = CARTESIAN_POINT ( 'NONE',  ( 17.99999999999999645, -101.1249659627852679, -48.60055280209521555 ) ) ;
#9103 = DIRECTION ( 'NONE',  ( -1.000000000000000000, 0.000000000000000000, 0.000000000000000000 ) ) ;
#9104 = AXIS2_PLACEMENT_3D ( 'NONE', #39326, #18709, #32171 ) ;
#9105 = EDGE_CURVE ( 'NONE', #36755, #33779, #32893, .T. ) ;
#9107 = CARTESIAN_POINT ( 'NONE',  ( 26.99674208481366833, 31.00000000000000355, -20.71990538090019029 ) ) ;
#9106 = AXIS2_PLACEMENT_3D ( 'NONE', #16353, #23564, #36832 ) ;
#9108 = ORIENTED_EDGE ( 'NONE', *, *, #2021, .F. ) ;
#9109 = EDGE_LOOP ( 'NONE', ( #18219, #24718, #2225, #22599 ) ) ;
#9110 = CIRCLE ( 'NONE', #14025, 47.49900000000000233 ) ;
#9111 = EDGE_CURVE ( 'NONE', #25035, #27234, #33581, .T. ) ;
#9112 = DIRECTION ( 'NONE',  ( 0.000000000000000000, 0.000000000000000000, 1.000000000000000000 ) ) ;
#9113 = CARTESIAN_POINT ( 'NONE',  ( -60.37409795221152109, 31.00000000000000711, -68.82020352599361956 ) ) ;
#9114 = DIRECTION ( 'NONE',  ( 0.000000000000000000, 0.8747630845319591675, 0.4845508703326539823 ) ) ;
#9115 = VERTEX_POINT ( 'NONE', #38582 ) ;
#9116 = CARTESIAN_POINT ( 'NONE',  ( 64.03668805592332092, 31.00000000000000000, 21.85318084035846198 ) ) ;
#9117 = CARTESIAN_POINT ( 'NONE',  ( 28.99662776679782539, 40.00000000000000000, -58.58186007941694129 ) ) ;
#9118 = CARTESIAN_POINT ( 'NONE',  ( -96.39699453480135105, 40.00000000000000711, 25.82690913164849889 ) ) ;
#9119 = EDGE_CURVE ( 'NONE', #23378, #42608, #9909, .T. ) ;
#9120 = VERTEX_POINT ( 'NONE', #38805 ) ;
#9121 = EDGE_CURVE ( 'NONE', #13471, #17450, #34896, .T. ) ;
#9122 = CYLINDRICAL_SURFACE ( 'NONE', #1104, 31.49899999999999878 ) ;
#9123 = FACE_OUTER_BOUND ( 'NONE', #33513, .T. ) ;
#9124 = LINE ( 'NONE', #25747, #10813 ) ;
#9126 = EDGE_LOOP ( 'NONE', ( #17712, #39071, #13862, #7163 ) ) ;
#9125 = CARTESIAN_POINT ( 'NONE',  ( 17.99999999999999645, 84.09610293794069946, 74.27057253243037849 ) ) ;
#9127 = DIRECTION ( 'NONE',  ( -3.996523416598930318E-16, 2.658563593772947863E-15, 1.000000000000000000 ) ) ;
#9128 = CIRCLE ( 'NONE', #28650, 36.00000000000000000 ) ;
#9129 = LINE ( 'NONE', #35723, #24477 ) ;
#9130 = ORIENTED_EDGE ( 'NONE', *, *, #40938, .T. ) ;
#9131 = CARTESIAN_POINT ( 'NONE',  ( -20.19574676229028043, 40.00000000000000000, 75.42596061005518493 ) ) ;
#9132 = LINE ( 'NONE', #15708, #23630 ) ;
#9133 = VECTOR ( 'NONE', #29136, 1000.000000000000000 ) ;
#9134 = AXIS2_PLACEMENT_3D ( 'NONE', #34519, #24095, #28011 ) ;
#9135 = ORIENTED_EDGE ( 'NONE', *, *, #36701, .F. ) ;
#9136 = DIRECTION ( 'NONE',  ( -3.009274222672345096E-17, -1.000000000000000000, 2.455023325076454960E-18 ) ) ;
#9137 = CIRCLE ( 'NONE', #33523, 59.00000000000000000 ) ;
#9138 = EDGE_LOOP ( 'NONE', ( #26067, #2140, #9267, #4132, #36040 ) ) ;
#9139 = EDGE_CURVE ( 'NONE', #3463, #18148, #12703, .T. ) ;
#9140 = ORIENTED_EDGE ( 'NONE', *, *, #31412, .F. ) ;
#9141 = FACE_OUTER_BOUND ( 'NONE', #42367, .T. ) ;
#9142 = ORIENTED_EDGE ( 'NONE', *, *, #38506, .T. ) ;
#9143 = AXIS2_PLACEMENT_3D ( 'NONE', #2788, #12871, #22502 ) ;
#9144 = DIRECTION ( 'NONE',  ( 1.000000000000000000, 0.000000000000000000, 0.000000000000000000 ) ) ;
#9145 = DIRECTION ( 'NONE',  ( 0.000000000000000000, 0.000000000000000000, 1.000000000000000000 ) ) ;
#9146 = DIRECTION ( 'NONE',  ( 1.000000000000000000, 0.000000000000000000, 0.000000000000000000 ) ) ;
#9147 = CARTESIAN_POINT ( 'NONE',  ( 0.000000000000000000, 29.86146780999950323, 112.0905559814579675 ) ) ;
#9148 = ORIENTED_EDGE ( 'NONE', *, *, #26266, .T. ) ;
#9149 = CARTESIAN_POINT ( 'NONE',  ( 17.99999999999999645, -51.98489025774375705, 108.7109110710159854 ) ) ;
#9150 = EDGE_CURVE ( 'NONE', #2165, #18762, #16198, .T. ) ;
#9151 = ORIENTED_EDGE ( 'NONE', *, *, #12158, .F. ) ;
#9152 = AXIS2_PLACEMENT_3D ( 'NONE', #14458, #27765, #21026 ) ;
#9153 = CARTESIAN_POINT ( 'NONE',  ( 17.99999999999999645, 79.94368240339547071, -90.16373242487824768 ) ) ;
#9154 = VERTEX_POINT ( 'NONE', #8063 ) ;
#9155 = CARTESIAN_POINT ( 'NONE',  ( 17.99999999999999645, 112.1427988504407551, 3.502162136923788083 ) ) ;
#9156 = EDGE_CURVE ( 'NONE', #2894, #35102, #32219, .T. ) ;
#9157 = CYLINDRICAL_SURFACE ( 'NONE', #37642, 47.49900000000000233 ) ;
#9158 = CONTEXT_DEPENDENT_SHAPE_REPRESENTATION ( #12274, #13771 ) ;
#9159 = LINE ( 'NONE', #16373, #27450 ) ;
#9160 = CARTESIAN_POINT ( 'NONE',  ( -30.90996028308246224, 31.00000000000000355, -53.51249422725337013 ) ) ;
#9161 = AXIS2_PLACEMENT_3D ( 'NONE', #15361, #24331, #17779 ) ;
#9162 = ORIENTED_EDGE ( 'NONE', *, *, #2182, .F. ) ;
#9163 = DIRECTION ( 'NONE',  ( -1.000000000000000000, 0.000000000000000000, 0.000000000000000000 ) ) ;
#9164 = AXIS2_PLACEMENT_3D ( 'NONE', #30683, #10825, #93 ) ;
#9165 = ORIENTED_EDGE ( 'NONE', *, *, #26503, .T. ) ;
#9166 = CARTESIAN_POINT ( 'NONE',  ( 12.49611804805956261, 31.00000000000000355, 37.00809541493615029 ) ) ;
#9167 = AXIS2_PLACEMENT_3D ( 'NONE', #33169, #16183, #9824 ) ;
#9168 = CARTESIAN_POINT ( 'NONE',  ( -53.60515337853228601, 40.00000000000000000, -47.01024902908782366 ) ) ;
#9169 = EDGE_CURVE ( 'NONE', #12063, #990, #1297, .T. ) ;
#9170 = AXIS2_PLACEMENT_3D ( 'NONE', #24435, #11320, #23998 ) ;
#9171 = CARTESIAN_POINT ( 'NONE',  ( 17.99999999999999645, 0.000000000000000000, 0.000000000000000000 ) ) ;
#9172 = CARTESIAN_POINT ( 'NONE',  ( 17.99999999999999645, 100.8494052988171035, 65.95368414178945216 ) ) ;
#9173 = EDGE_CURVE ( 'NONE', #23341, #3516, #24917, .T. ) ;
#9174 = CYLINDRICAL_SURFACE ( 'NONE', #24679, 59.00000000000000000 ) ;
#9175 = CARTESIAN_POINT ( 'NONE',  ( 0.000000000000000000, 150.5000000000000284, 10.00000000000000000 ) ) ;
#9176 = PRODUCT_DEFINITION_SHAPE ( 'NONE', 'NONE',  #43198 ) ;
#9177 = ORIENTED_EDGE ( 'NONE', *, *, #38033, .F. ) ;
#9178 = CARTESIAN_POINT ( 'NONE',  ( 19.15075862373047144, 40.00000000000000000, -38.85840887180553693 ) ) ;
#9179 = DIRECTION ( 'NONE',  ( -1.000000000000000000, -0.000000000000000000, -0.000000000000000000 ) ) ;
#9180 = LINE ( 'NONE', #25996, #15247 ) ;
#9181 = VERTEX_POINT ( 'NONE', #38169 ) ;
#9182 = DIRECTION ( 'NONE',  ( -1.000000000000000000, 0.000000000000000000, -0.000000000000000000 ) ) ;
#9183 = CARTESIAN_POINT ( 'NONE',  ( 17.99999999999999645, -29.02167576844178853, 108.3790330702168774 ) ) ;
#9184 = ORIENTED_EDGE ( 'NONE', *, *, #38804, .T. ) ;
#9185 = DIRECTION ( 'NONE',  ( 1.000000000000000000, 0.000000000000000000, 0.000000000000000000 ) ) ;
#9186 = ORIENTED_EDGE ( 'NONE', *, *, #36883, .T. ) ;
#9187 = ADVANCED_FACE ( 'NONE', ( #24686 ), #31627, .T. ) ;
#9188 = VECTOR ( 'NONE', #14217, 1000.000000000000000 ) ;
#9189 = EDGE_LOOP ( 'NONE', ( #7159, #41675, #9033, #42236 ) ) ;
#9190 = CARTESIAN_POINT ( 'NONE',  ( 17.99999999999999645, -16.86122981692037825, 27.13802899033285954 ) ) ;
#9191 = CIRCLE ( 'NONE', #16165, 58.99999999999998579 ) ;
#9192 = CARTESIAN_POINT ( 'NONE',  ( 69.92891852055319646, 31.00000000000000000, 53.79372986807582180 ) ) ;
#9193 = ORIENTED_EDGE ( 'NONE', *, *, #22735, .F. ) ;
#9194 = CARTESIAN_POINT ( 'NONE',  ( 18.00000000000000355, 0.000000000000000000, 0.000000000000000000 ) ) ;
#9195 = CIRCLE ( 'NONE', #35659, 20.00000000000000711 ) ;
#9196 = DIRECTION ( 'NONE',  ( -1.000000000000000000, 0.000000000000000000, 0.000000000000000000 ) ) ;
#9197 = CARTESIAN_POINT ( 'NONE',  ( 17.99999999999999645, 28.62203781743003717, -14.19692359621465094 ) ) ;
#9198 = ORIENTED_EDGE ( 'NONE', *, *, #40467, .T. ) ;
#9199 = CYLINDRICAL_SURFACE ( 'NONE', #3558, 58.99999999999999289 ) ;
#9200 = ADVANCED_FACE ( 'NONE', ( #41865 ), #22063, .T. ) ;
#9201 = DIRECTION ( 'NONE',  ( -1.058513553088275437E-16, -1.000000000000000000, 8.813324511995299047E-17 ) ) ;
#9202 = AXIS2_PLACEMENT_3D ( 'NONE', #31494, #24992, #35169 ) ;
#9203 = DIRECTION ( 'NONE',  ( 0.000000000000000000, 0.000000000000000000, 1.000000000000000000 ) ) ;
#9204 = EDGE_CURVE ( 'NONE', #27281, #12154, #41232, .T. ) ;
#9206 = LINE ( 'NONE', #35794, #15113 ) ;
#9205 = CARTESIAN_POINT ( 'NONE',  ( 0.000000000000000000, 0.7408941433508176022, -1.199999999999999956 ) ) ;
#9207 = CARTESIAN_POINT ( 'NONE',  ( 17.99999999999999645, 120.4984140710909344, -0.7894348306988416830 ) ) ;
#9208 = ORIENTED_EDGE ( 'NONE', *, *, #16817, .T. ) ;
#9209 = CARTESIAN_POINT ( 'NONE',  ( 17.42035916340572399, 31.00000000000000355, 19.85006075799527991 ) ) ;
#9210 = EDGE_LOOP ( 'NONE', ( #25750, #28064, #21092, #17412 ) ) ;
#9211 = DIRECTION ( 'NONE',  ( 0.000000000000000000, 0.000000000000000000, 1.000000000000000000 ) ) ;
#9212 = FACE_OUTER_BOUND ( 'NONE', #26209, .T. ) ;
#9213 = VERTEX_POINT ( 'NONE', #35528 ) ;
#9214 = CARTESIAN_POINT ( 'NONE',  ( -31.00354902519490352, 40.00000000000000000, -27.18544651223506392 ) ) ;
#9215 = CARTESIAN_POINT ( 'NONE',  ( 34.63398384099732397, 40.00000000000000000, -11.69655689657770559 ) ) ;
#9216 = ORIENTED_EDGE ( 'NONE', *, *, #32072, .T. ) ;
#9217 = VECTOR ( 'NONE', #24307, 1000.000000000000000 ) ;
#9218 = EDGE_CURVE ( 'NONE', #13944, #7683, #42497, .T. ) ;
#9219 = ORIENTED_EDGE ( 'NONE', *, *, #20013, .T. ) ;
#9220 = CARTESIAN_POINT ( 'NONE',  ( 0.000000000000000000, -8.827181066046705382, 120.1772519049559378 ) ) ;
#9221 = DIRECTION ( 'NONE',  ( -1.000000000000000000, 0.000000000000000000, 0.000000000000000000 ) ) ;
#9222 = EDGE_CURVE ( 'NONE', #18461, #39703, #5030, .T. ) ;
#9223 = FACE_OUTER_BOUND ( 'NONE', #27021, .T. ) ;
#9224 = EDGE_CURVE ( 'NONE', #12270, #5471, #2573, .T. ) ;
#9225 = ADVANCED_FACE ( 'NONE', ( #16137 ), #22698, .T. ) ;
#9227 = EDGE_CURVE ( 'NONE', #30882, #16679, #35949, .T. ) ;
#9226 = CIRCLE ( 'NONE', #34330, 4.500000000000002665 ) ;
#9228 = DIRECTION ( 'NONE',  ( 1.000000000000000000, 0.000000000000000000, 0.000000000000000000 ) ) ;
#9229 = CARTESIAN_POINT ( 'NONE',  ( 9.000000000000000000, 7.220349212960450735, 35.26849241522667455 ) ) ;
#9230 = DIRECTION ( 'NONE',  ( 0.000000000000000000, 0.7980172272802407152, -0.6026346363792548511 ) ) ;
#9231 = ORIENTED_EDGE ( 'NONE', *, *, #35388, .T. ) ;
#9232 = LINE ( 'NONE', #35823, #33320 ) ;
#9233 = ORIENTED_EDGE ( 'NONE', *, *, #3209, .T. ) ;
#9234 = CARTESIAN_POINT ( 'NONE',  ( 67.80287614962797704, -2.055254544495724645, 69.29271901957280022 ) ) ;
#9235 = CIRCLE ( 'NONE', #39178, 58.99999999999999289 ) ;
#9236 = DIRECTION ( 'NONE',  ( -1.000000000000000000, -0.000000000000000000, -0.000000000000000000 ) ) ;
#9237 = CARTESIAN_POINT ( 'NONE',  ( 8.999999999999998224, 107.1354928292869744, 44.47455650398100602 ) ) ;
#9238 = DIRECTION ( 'NONE',  ( 0.000000000000000000, 0.000000000000000000, 1.000000000000000000 ) ) ;
#9239 = ORIENTED_EDGE ( 'NONE', *, *, #31235, .F. ) ;
#9240 = CARTESIAN_POINT ( 'NONE',  ( 58.84426737335365232, 40.00000000000000000, 76.69096868241209108 ) ) ;
#9241 = EDGE_LOOP ( 'NONE', ( #27594, #42677, #27418, #8161 ) ) ;
#9242 = FACE_OUTER_BOUND ( 'NONE', #8839, .T. ) ;
#9243 = ORIENTED_EDGE ( 'NONE', *, *, #18518, .T. ) ;
#9245 = ORIENTED_EDGE ( 'NONE', *, *, #29055, .F. ) ;
#9244 = CARTESIAN_POINT ( 'NONE',  ( -16.80298683001097260, 17.11489954122026447, 2.367532924972517439 ) ) ;
#9246 = CARTESIAN_POINT ( 'NONE',  ( -3.469229457552013507, 31.00000000000000355, -54.39987425099493379 ) ) ;
#9247 = EDGE_LOOP ( 'NONE', ( #11230, #16589, #20794, #223 ) ) ;
#9248 = CARTESIAN_POINT ( 'NONE',  ( 18.00000000000000355, 0.000000000000000000, 0.000000000000000000 ) ) ;
#9249 = DIRECTION ( 'NONE',  ( -1.000000000000000000, -0.000000000000000000, -0.000000000000000000 ) ) ;
#9250 = ADVANCED_FACE ( 'NONE', ( #19211 ), #16586, .T. ) ;
#9251 = EDGE_LOOP ( 'NONE', ( #22422, #10094, #39979, #5222 ) ) ;
#9252 = CARTESIAN_POINT ( 'NONE',  ( -46.76215110880508519, 40.00000000000000000, 53.15211786533807725 ) ) ;
#9253 = EDGE_CURVE ( 'NONE', #19733, #255, #29427, .T. ) ;
#9255 = DIRECTION ( 'NONE',  ( -1.000000000000000000, 0.000000000000000000, 0.000000000000000000 ) ) ;
#9254 = CYLINDRICAL_SURFACE ( 'NONE', #37725, 20.00000000000000711 ) ;
#9256 = AXIS2_PLACEMENT_3D ( 'NONE', #32854, #38963, #3151 ) ;
#9257 = CARTESIAN_POINT ( 'NONE',  ( 17.99999999999999645, -116.0452958106478434, -32.46506308663576590 ) ) ;
#9258 = ORIENTED_EDGE ( 'NONE', *, *, #19237, .T. ) ;
#9259 = CYLINDRICAL_SURFACE ( 'NONE', #14048, 59.00000000000000000 ) ;
#9260 = ORIENTED_EDGE ( 'NONE', *, *, #41455, .F. ) ;
#9261 = AXIS2_PLACEMENT_3D ( 'NONE', #39031, #29457, #22508 ) ;
#9262 = CYLINDRICAL_SURFACE ( 'NONE', #2309, 20.00000000000000711 ) ;
#9263 = DIRECTION ( 'NONE',  ( -0.2604563316218754254, -1.023593278765030694E-15, -0.9654856287475623855 ) ) ;
#9264 = CARTESIAN_POINT ( 'NONE',  ( -47.90394619311608437, 31.00000000000000355, 62.45286580340285099 ) ) ;
#9266 = LINE ( 'NONE', #25885, #28361 ) ;
#9265 = CARTESIAN_POINT ( 'NONE',  ( -91.96080130434580724, -34.05525454449571043, 14.45886780445738218 ) ) ;
#9267 = ORIENTED_EDGE ( 'NONE', *, *, #41442, .T. ) ;
#9268 = FACE_OUTER_BOUND ( 'NONE', #29947, .T. ) ;
#9269 = VERTEX_POINT ( 'NONE', #32695 ) ;
#9270 = DIRECTION ( 'NONE',  ( -0.000000000000000000, -0.000000000000000000, 1.000000000000000000 ) ) ;
#9271 = DIRECTION ( 'NONE',  ( -1.000000000000000000, 0.000000000000000000, -0.000000000000000000 ) ) ;
#9272 = EDGE_CURVE ( 'NONE', #37517, #39291, #36171, .T. ) ;
#9273 = CARTESIAN_POINT ( 'NONE',  ( -6.638544827991894159, 31.00000000000000355, 99.59190654106262741 ) ) ;
#9274 = CARTESIAN_POINT ( 'NONE',  ( 58.37089435906660384, 39.99999999999999289, -75.89027429297954086 ) ) ;
#9275 = EDGE_CURVE ( 'NONE', #11938, #39753, #16899, .T. ) ;
#9276 = EDGE_CURVE ( 'NONE', #17401, #40745, #39146, .T. ) ;
#9277 = CARTESIAN_POINT ( 'NONE',  ( 17.99999999999999645, 96.25468616236661035, 72.49500943364525085 ) ) ;
#9278 = EDGE_CURVE ( 'NONE', #10268, #631, #7857, .T. ) ;
#9279 = CIRCLE ( 'NONE', #181, 14.99999999999999822 ) ;
#9280 = ORIENTED_EDGE ( 'NONE', *, *, #19762, .F. ) ;
#9281 = DIRECTION ( 'NONE',  ( 0.000000000000000000, 0.000000000000000000, 1.000000000000000000 ) ) ;
#9282 = ORIENTED_EDGE ( 'NONE', *, *, #1788, .F. ) ;
#9283 = FACE_OUTER_BOUND ( 'NONE', #23562, .T. ) ;
#9284 = CARTESIAN_POINT ( 'NONE',  ( 0.000000000000000000, -23.79363200506935172, -27.01597816121672224 ) ) ;
#9285 = EDGE_CURVE ( 'NONE', #967, #21211, #41262, .T. ) ;
#9286 = CARTESIAN_POINT ( 'NONE',  ( 17.99999999999999645, -111.7974656912330715, 9.465682155095141326 ) ) ;
#9287 = ORIENTED_EDGE ( 'NONE', *, *, #24012, .T. ) ;
#9288 = DIRECTION ( 'NONE',  ( 0.000000000000000000, 0.7865515558026396903, 0.6175246149461955936 ) ) ;
#9289 = DIRECTION ( 'NONE',  ( -1.000000000000000000, -0.000000000000000000, 0.000000000000000000 ) ) ;
#9290 = DIRECTION ( 'NONE',  ( 1.000000000000000000, -0.000000000000000000, 0.000000000000000000 ) ) ;
#9291 = AXIS2_PLACEMENT_3D ( 'NONE', #2120, #12412, #41837 ) ;
#9292 = ORIENTED_EDGE ( 'NONE', *, *, #52, .F. ) ;
#9293 = CARTESIAN_POINT ( 'NONE',  ( 17.99999999999999645, -41.60679253225836760, 108.2814610871944581 ) ) ;
#9294 = CYLINDRICAL_SURFACE ( 'NONE', #35561, 47.49900000000000233 ) ;
#9295 = VECTOR ( 'NONE', #40781, 1000.000000000000000 ) ;
#9297 = VERTEX_POINT ( 'NONE', #15711 ) ;
#9296 = CARTESIAN_POINT ( 'NONE',  ( 18.00000000000000355, -20.99948489194393275, -42.60488980472802467 ) ) ;
#9298 = ORIENTED_EDGE ( 'NONE', *, *, #20565, .F. ) ;
#9299 = DIRECTION ( 'NONE',  ( 0.000000000000000000, 0.000000000000000000, 1.000000000000000000 ) ) ;
#9300 = FACE_OUTER_BOUND ( 'NONE', #28185, .T. ) ;
#9301 = CARTESIAN_POINT ( 'NONE',  ( 10.06970066534629815, 40.00000000000000000, 37.84957806120350199 ) ) ;
#9302 = CARTESIAN_POINT ( 'NONE',  ( 17.99999999999999645, 5.456439917444967591, 112.0647122740742105 ) ) ;
#9303 = AXIS2_PLACEMENT_3D ( 'NONE', #37598, #41074, #1810 ) ;
#9304 = DIRECTION ( 'NONE',  ( 0.000000000000000000, 0.000000000000000000, 1.000000000000000000 ) ) ;
#9305 = VECTOR ( 'NONE', #41020, 1000.000000000000000 ) ;
#9306 = CARTESIAN_POINT ( 'NONE',  ( 1.999999999999998224, -3.464101615137772594, -3.142992957459239012 ) ) ;
#9307 = ORIENTED_EDGE ( 'NONE', *, *, #17115, .T. ) ;
#9308 = LINE ( 'NONE', #22662, #23769 ) ;
#9309 = ORIENTED_EDGE ( 'NONE', *, *, #15526, .T. ) ;
#9310 = CIRCLE ( 'NONE', #212, 13.59999999999999787 ) ;
#9311 = CARTESIAN_POINT ( 'NONE',  ( 0.000000000000000000, 39.78933988720149273, -24.98727647984960498 ) ) ;
#9312 = FACE_OUTER_BOUND ( 'NONE', #19651, .T. ) ;
#9313 = CARTESIAN_POINT ( 'NONE',  ( 22.22924588317381023, 31.00000000000000355, -25.35314793696836588 ) ) ;
#9314 = DIRECTION ( 'NONE',  ( -1.000000000000000000, -0.000000000000000000, 0.000000000000000000 ) ) ;
#9315 = VERTEX_POINT ( 'NONE', #39439 ) ;
#9316 = FACE_OUTER_BOUND ( 'NONE', #25481, .T. ) ;
#9317 = CARTESIAN_POINT ( 'NONE',  ( 81.71702119589899382, 31.00000000000000000, -47.19735719316410183 ) ) ;
#9318 = AXIS2_PLACEMENT_3D ( 'NONE', #7980, #4041, #11067 ) ;
#9319 = DIRECTION ( 'NONE',  ( -1.000000000000000000, 0.000000000000000000, 0.000000000000000000 ) ) ;
#9320 = ORIENTED_EDGE ( 'NONE', *, *, #15309, .T. ) ;
#9321 = CARTESIAN_POINT ( 'NONE',  ( -45.90931453311223720, 31.00000000000000355, 40.13788153756826915 ) ) ;
#9322 = CARTESIAN_POINT ( 'NONE',  ( -50.06114249711410480, 40.00000000000000000, -38.53249520213266521 ) ) ;
#9323 = EDGE_CURVE ( 'NONE', #37475, #5117, #132, .T. ) ;
#9324 = CARTESIAN_POINT ( 'NONE',  ( 18.00000000000000355, 0.000000000000000000, 0.000000000000000000 ) ) ;
#9325 = AXIS2_PLACEMENT_3D ( 'NONE', #19856, #42707, #19642 ) ;
#9326 = EDGE_CURVE ( 'NONE', #19393, #30398, #39215, .T. ) ;
#9327 = ORIENTED_EDGE ( 'NONE', *, *, #42887, .F. ) ;
#9328 = FILL_AREA_STYLE ('',( #36365 ) ) ;
#9329 = CIRCLE ( 'NONE', #35778, 13.60000000000000497 ) ;
#9330 = DIRECTION ( 'NONE',  ( -1.000000000000000000, -0.000000000000000000, 0.000000000000000000 ) ) ;
#9331 = FACE_BOUND ( 'NONE', #35580, .T. ) ;
#9333 = VERTEX_POINT ( 'NONE', #9344 ) ;
#9332 = CYLINDRICAL_SURFACE ( 'NONE', #23472, 13.59999999999999964 ) ;
#9334 = CYLINDRICAL_SURFACE ( 'NONE', #10754, 116.0000000000000000 ) ;
#9335 = PLANE ( 'NONE',  #18231 ) ;
#9336 = EDGE_CURVE ( 'NONE', #41904, #17494, #32925, .T. ) ;
#9337 = AXIS2_PLACEMENT_3D ( 'NONE', #24677, #28148, #37514 ) ;
#9338 = VERTEX_POINT ( 'NONE', #9780 ) ;
#9339 = CARTESIAN_POINT ( 'NONE',  ( 4.745113895470035814, 40.00000000000000000, -72.60416666572081112 ) ) ;
#9340 = DIRECTION ( 'NONE',  ( 0.000000000000000000, 1.423061292157245201E-14, -1.000000000000000000 ) ) ;
#9341 = ORIENTED_EDGE ( 'NONE', *, *, #33562, .T. ) ;
#9342 = EDGE_CURVE ( 'NONE', #11045, #16762, #14839, .T. ) ;
#9343 = DIRECTION ( 'NONE',  ( -1.000000000000000000, 0.000000000000000000, 0.000000000000000000 ) ) ;
#9344 = CARTESIAN_POINT ( 'NONE',  ( 0.000000000000000000, 18.53613841426789222, 48.58406706613909876 ) ) ;
#9345 = ORIENTED_EDGE ( 'NONE', *, *, #1926, .T. ) ;
#9346 = AXIS2_PLACEMENT_3D ( 'NONE', #40580, #40799, #27311 ) ;
#9347 = VERTEX_POINT ( 'NONE', #30932 ) ;
#9348 = CARTESIAN_POINT ( 'NONE',  ( -22.00000000000000000, 31.00000000000000355, 0.000000000000000000 ) ) ;
#9349 = CIRCLE ( 'NONE', #12155, 120.5010000000000190 ) ;
#9350 = ORIENTED_EDGE ( 'NONE', *, *, #2174, .T. ) ;
#9351 = CARTESIAN_POINT ( 'NONE',  ( 0.000000000000000000, 120.2856157092986678, 7.201503623197233139 ) ) ;
#9352 = DIRECTION ( 'NONE',  ( 3.996523416598930318E-16, -2.658563593772947863E-15, -1.000000000000000000 ) ) ;
#9353 = DIRECTION ( 'NONE',  ( -1.000000000000000000, -0.000000000000000000, -0.000000000000000000 ) ) ;
#9354 = DIRECTION ( 'NONE',  ( 1.000000000000000000, 0.000000000000000000, 0.000000000000000000 ) ) ;
#9356 = ORIENTED_EDGE ( 'NONE', *, *, #17580, .F. ) ;
#9355 = AXIS2_PLACEMENT_3D ( 'NONE', #38969, #3155, #13251 ) ;
#9357 = CARTESIAN_POINT ( 'NONE',  ( 0.000000000000000000, -103.5682682299991342, 43.14958040911493242 ) ) ;
#9358 = VECTOR ( 'NONE', #22941, 1000.000000000000000 ) ;
#9359 = ORIENTED_EDGE ( 'NONE', *, *, #31108, .F. ) ;
#9360 = CIRCLE ( 'NONE', #33057, 52.00000000000000000 ) ;
#9361 = CARTESIAN_POINT ( 'NONE',  ( 0.000000000000000000, 0.000000000000000000, 0.000000000000000000 ) ) ;
#9362 = ORIENTED_EDGE ( 'NONE', *, *, #18344, .F. ) ;
#9363 = CARTESIAN_POINT ( 'NONE',  ( 2.500000000000000000, -1.768423874527825568, -1.020999999999998575 ) ) ;
#9364 = CIRCLE ( 'NONE', #273, 25.00000000000000000 ) ;
#9365 = CYLINDRICAL_SURFACE ( 'NONE', #14703, 51.99999999999999289 ) ;
#9367 = CIRCLE ( 'NONE', #2372, 120.5010000000000332 ) ;
#9366 = CARTESIAN_POINT ( 'NONE',  ( 4.101954839143059139, -2.368264730582948285, -3.681130640444269631 ) ) ;
#9368 = CARTESIAN_POINT ( 'NONE',  ( 37.24516168167158270, 31.00000000000000355, 42.45166511289891531 ) ) ;
#9369 = DIRECTION ( 'NONE',  ( -1.058513553088275437E-16, -1.000000000000000000, 8.813324511995299047E-17 ) ) ;
#9370 = EDGE_LOOP ( 'NONE', ( #2755, #30348, #4749, #32743 ) ) ;
#9371 = CARTESIAN_POINT ( 'NONE',  ( 17.75583184595726749, 31.00000000000000355, -30.63479189996604646 ) ) ;
#9372 = EDGE_CURVE ( 'NONE', #11416, #640, #12060, .T. ) ;
#9373 = CARTESIAN_POINT ( 'NONE',  ( 23.52215716829092074, 40.00000000000000000, -69.29398394448777765 ) ) ;
#9374 = ADVANCED_FACE ( 'NONE', ( #33763 ), #13728, .F. ) ;
#9375 = AXIS2_PLACEMENT_3D ( 'NONE', #37161, #13423, #3551 ) ;
#9376 = DIRECTION ( 'NONE',  ( -1.000000000000000000, 0.000000000000000000, 0.000000000000000000 ) ) ;
#9377 = DIRECTION ( 'NONE',  ( 1.000000000000000000, -0.000000000000000000, 0.000000000000000000 ) ) ;
#9378 = DIRECTION ( 'NONE',  ( 0.000000000000000000, 0.000000000000000000, 1.000000000000000000 ) ) ;
#9379 = VECTOR ( 'NONE', #2939, 1000.000000000000000 ) ;
#9380 = CARTESIAN_POINT ( 'NONE',  ( -109.0695705685756138, 106.4195705685752529, 9.999999999999998224 ) ) ;
#9381 = ADVANCED_FACE ( 'NONE', ( #26801 ), #4291, .T. ) ;
#9382 = VECTOR ( 'NONE', #24432, 1000.000000000000000 ) ;
#9383 = ORIENTED_EDGE ( 'NONE', *, *, #16817, .F. ) ;
#9384 = CARTESIAN_POINT ( 'NONE',  ( 34.94781834021004840, 40.00000000000000000, -26.81980329959834108 ) ) ;
#9385 = DIRECTION ( 'NONE',  ( 0.000000000000000000, 0.000000000000000000, 1.000000000000000000 ) ) ;
#9386 = DIRECTION ( 'NONE',  ( 1.000000000000000000, -0.000000000000000000, -0.000000000000000000 ) ) ;
#9387 = AXIS2_PLACEMENT_3D ( 'NONE', #15291, #29003, #5432 ) ;
#9388 = ORIENTED_EDGE ( 'NONE', *, *, #2206, .F. ) ;
#9389 = ADVANCED_FACE ( 'NONE', ( #7585 ), #3845, .F. ) ;
#9390 = CARTESIAN_POINT ( 'NONE',  ( 0.000000000000000000, 0.000000000000000000, 0.000000000000000000 ) ) ;
#9391 = CARTESIAN_POINT ( 'NONE',  ( 8.999999999999998224, 86.84764344322962870, 76.89919913989776035 ) ) ;
#9392 = AXIS2_PLACEMENT_3D ( 'NONE', #2700, #8851, #42839 ) ;
#9393 = EDGE_LOOP ( 'NONE', ( #30445, #19614, #2336, #7981 ) ) ;
#9394 = CARTESIAN_POINT ( 'NONE',  ( 9.000000000000001776, 49.65209126885784485, -15.44894276735497662 ) ) ;
#9395 = ORIENTED_EDGE ( 'NONE', *, *, #8574, .T. ) ;
#9396 = AXIS2_PLACEMENT_3D ( 'NONE', #7948, #24576, #27388 ) ;
#9397 = ORIENTED_EDGE ( 'NONE', *, *, #22251, .T. ) ;
#9398 = FACE_OUTER_BOUND ( 'NONE', #42070, .T. ) ;
#9399 = CARTESIAN_POINT ( 'NONE',  ( 76.36627019853398224, 31.00000000000000000, -58.43797548692494814 ) ) ;
#9400 = ORIENTED_EDGE ( 'NONE', *, *, #2820, .T. ) ;
#9401 = DIRECTION ( 'NONE',  ( -1.000000000000000000, -0.000000000000000000, 0.000000000000000000 ) ) ;
#9402 = DIRECTION ( 'NONE',  ( 0.000000000000000000, 1.000000000000000000, 0.000000000000000000 ) ) ;
#9403 = DIRECTION ( 'NONE',  ( -1.000000000000000000, 0.000000000000000000, 0.000000000000000000 ) ) ;
#9404 = ORIENTED_EDGE ( 'NONE', *, *, #8408, .T. ) ;
#9405 = CARTESIAN_POINT ( 'NONE',  ( 17.99999999999999645, -51.98489025774233596, -108.7109110710166391 ) ) ;
#9406 = CARTESIAN_POINT ( 'NONE',  ( -10.00000000000000000, 0.000000000000000000, 0.000000000000000000 ) ) ;
#9407 = EDGE_CURVE ( 'NONE', #20671, #2041, #35020, .T. ) ;
#9408 = CARTESIAN_POINT ( 'NONE',  ( 17.99999999999999645, 47.58001226230536673, 110.7096808509485300 ) ) ;
#9409 = EDGE_CURVE ( 'NONE', #9666, #14373, #33607, .T. ) ;
#9410 = CIRCLE ( 'NONE', #10129, 2.799122904894268959 ) ;
#9412 = CARTESIAN_POINT ( 'NONE',  ( -10.00000000000000000, 0.000000000000000000, 116.0000000000000000 ) ) ;
#9411 = CARTESIAN_POINT ( 'NONE',  ( 17.99999999999999645, 0.000000000000000000, 0.000000000000000000 ) ) ;
#9413 = AXIS2_PLACEMENT_3D ( 'NONE', #29937, #42987, #13144 ) ;
#9414 = DIRECTION ( 'NONE',  ( 1.000000000000000000, 0.000000000000000000, 0.000000000000000000 ) ) ;
#9415 = AXIS2_PLACEMENT_3D ( 'NONE', #33503, #37794, #7912 ) ;
#9416 = ORIENTED_EDGE ( 'NONE', *, *, #28891, .T. ) ;
#9417 = CIRCLE ( 'NONE', #33122, 116.0000000000000000 ) ;
#9418 = DIRECTION ( 'NONE',  ( 0.9980725836333634859, 2.103535471517291975E-19, 0.06205737506068762649 ) ) ;
#9419 = CARTESIAN_POINT ( 'NONE',  ( -21.73352778766994575, 31.00000000000000355, 19.07242603999910457 ) ) ;
#9420 = VERTEX_POINT ( 'NONE', #20942 ) ;
#9421 = STYLED_ITEM ( 'NONE', ( #37381 ), #13444 ) ;
#9422 = CARTESIAN_POINT ( 'NONE',  ( 0.000000000000000000, -39.64889472655755043, 33.64468972902493960 ) ) ;
#9423 = VECTOR ( 'NONE', #25514, 1000.000000000000000 ) ;
#9424 = DIRECTION ( 'NONE',  ( 0.000000000000000000, 0.000000000000000000, 1.000000000000000000 ) ) ;
#9425 = ORIENTED_EDGE ( 'NONE', *, *, #19283, .T. ) ;
#9426 = STYLED_ITEM ( 'NONE', ( #33686 ), #27879 ) ;
#9427 = DIRECTION ( 'NONE',  ( -1.000000000000000000, -0.000000000000000000, -0.000000000000000000 ) ) ;
#9428 = CARTESIAN_POINT ( 'NONE',  ( -12.24460912605626106, 40.00000000000000000, 36.08157028455360660 ) ) ;
#9429 = EDGE_CURVE ( 'NONE', #29862, #38233, #3624, .T. ) ;
#9430 = CARTESIAN_POINT ( 'NONE',  ( -10.89792128226954482, 40.00000000000000000, -32.25956908328721795 ) ) ;
#9431 = VECTOR ( 'NONE', #11247, 1000.000000000000000 ) ;
#9432 = ORIENTED_EDGE ( 'NONE', *, *, #10930, .T. ) ;
#9433 = ORIENTED_EDGE ( 'NONE', *, *, #25867, .F. ) ;
#9434 = CARTESIAN_POINT ( 'NONE',  ( -10.00000000000000000, 0.000000000000000000, 0.000000000000000000 ) ) ;
#9435 = DIRECTION ( 'NONE',  ( 0.000000000000000000, 0.000000000000000000, 1.000000000000000000 ) ) ;
#9436 = DIRECTION ( 'NONE',  ( -1.000000000000000000, -0.000000000000000000, -0.000000000000000000 ) ) ;
#9437 = DIRECTION ( 'NONE',  ( 0.000000000000000000, 0.000000000000000000, 1.000000000000000000 ) ) ;
#9438 = EDGE_CURVE ( 'NONE', #31862, #7662, #39172, .T. ) ;
#9439 = DIRECTION ( 'NONE',  ( -1.000000000000000000, 0.000000000000000000, 0.000000000000000000 ) ) ;
#9440 = VERTEX_POINT ( 'NONE', #33551 ) ;
#9441 = CARTESIAN_POINT ( 'NONE',  ( -15.99999999999997691, 40.00000000000000711, 4.500000000000005329 ) ) ;
#9442 = VERTEX_POINT ( 'NONE', #24208 ) ;
#9443 = DIRECTION ( 'NONE',  ( -1.000000000000000000, 0.000000000000000000, -0.000000000000000000 ) ) ;
#9444 = CARTESIAN_POINT ( 'NONE',  ( 0.000000000000000000, -46.19362259308839214, 8.585149169758333088 ) ) ;
#9445 =( REPRESENTATION_RELATIONSHIP ('NONE','NONE', #330, #18009 ) REPRESENTATION_RELATIONSHIP_WITH_TRANSFORMATION ( #824 )SHAPE_REPRESENTATION_RELATIONSHIP( ) );
#9446 = EDGE_CURVE ( 'NONE', #3132, #35775, #28786, .T. ) ;
#9447 = AXIS2_PLACEMENT_3D ( 'NONE', #35172, #21920, #41504 ) ;
#9448 = CARTESIAN_POINT ( 'NONE',  ( 17.99999999999999645, 66.49630760163724119, -90.36876423295917959 ) ) ;
#9449 = DIRECTION ( 'NONE',  ( 1.000000000000000000, 0.000000000000000000, 0.000000000000000000 ) ) ;
#9450 = EDGE_CURVE ( 'NONE', #1738, #39440, #9226, .T. ) ;
#9451 = ORIENTED_EDGE ( 'NONE', *, *, #29330, .F. ) ;
#9452 = DIRECTION ( 'NONE',  ( -1.000000000000000000, 0.000000000000000000, 0.000000000000000000 ) ) ;
#9453 = VERTEX_POINT ( 'NONE', #36595 ) ;
#9454 = AXIS2_PLACEMENT_3D ( 'NONE', #24698, #20793, #34471 ) ;
#9455 = DIRECTION ( 'NONE',  ( -1.000000000000000000, 0.000000000000000000, -0.000000000000000000 ) ) ;
#9456 = AXIS2_PLACEMENT_3D ( 'NONE', #23532, #10184, #36800 ) ;
#9457 = ORIENTED_EDGE ( 'NONE', *, *, #743, .F. ) ;
#9458 = AXIS2_PLACEMENT_3D ( 'NONE', #33475, #37816, #21085 ) ;
#9460 = ORIENTED_EDGE ( 'NONE', *, *, #37170, .T. ) ;
#9459 = DIRECTION ( 'NONE',  ( 0.000000000000000000, 0.000000000000000000, 1.000000000000000000 ) ) ;
#9461 = CARTESIAN_POINT ( 'NONE',  ( 54.79583221319987985, 31.00000000000000355, -14.58025558542526490 ) ) ;
#9462 = AXIS2_PLACEMENT_3D ( 'NONE', #4924, #8207, #34817 ) ;
#9463 = ORIENTED_EDGE ( 'NONE', *, *, #24225, .T. ) ;
#9464 = DIRECTION ( 'NONE',  ( 0.000000000000000000, 0.3140767120219494779, -0.9493976084683810601 ) ) ;
#9465 = AXIS2_PLACEMENT_3D ( 'NONE', #33584, #26623, #13543 ) ;
#9466 = AXIS2_PLACEMENT_3D ( 'NONE', #37047, #10443, #20510 ) ;
#9467 = ORIENTED_EDGE ( 'NONE', *, *, #18776, .F. ) ;
#9468 = DIRECTION ( 'NONE',  ( 0.000000000000000000, 0.000000000000000000, 1.000000000000000000 ) ) ;
#9469 = AXIS2_PLACEMENT_3D ( 'NONE', #22925, #31909, #26162 ) ;
#9470 = EDGE_LOOP ( 'NONE', ( #9786, #7427, #5281, #29328 ) ) ;
#9471 = CARTESIAN_POINT ( 'NONE',  ( -55.03444096782886419, 40.00000000000000000, -48.41538206857744342 ) ) ;
#9472 = EDGE_CURVE ( 'NONE', #32590, #20200, #6717, .T. ) ;
#9474 = LINE ( 'NONE', #22827, #41576 ) ;
#9473 = CARTESIAN_POINT ( 'NONE',  ( 17.99999999999999645, -68.61497464550663494, 99.05794392877579924 ) ) ;
#9475 = EDGE_CURVE ( 'NONE', #16762, #1510, #20418, .T. ) ;
#9476 = LINE ( 'NONE', #2472, #27599 ) ;
#9477 = ORIENTED_EDGE ( 'NONE', *, *, #13060, .T. ) ;
#9478 = CARTESIAN_POINT ( 'NONE',  ( 17.99999999999999645, -92.10690493017015967, -64.06707842432270184 ) ) ;
#9479 = ORIENTED_EDGE ( 'NONE', *, *, #18512, .T. ) ;
#9480 =( NAMED_UNIT ( * ) PLANE_ANGLE_UNIT ( ) SI_UNIT ( $, .RADIAN. ) );
#9481 = LINE ( 'NONE', #5569, #2984 ) ;
#9482 = CARTESIAN_POINT ( 'NONE',  ( -100.0589655806010967, 40.00000000000002132, 21.59728106529621883 ) ) ;
#9483 = CARTESIAN_POINT ( 'NONE',  ( 66.75446398494719347, 31.00000000000000000, -32.91950810868348043 ) ) ;
#9485 = DIRECTION ( 'NONE',  ( 0.000000000000000000, -1.224646799147313518E-16, 1.000000000000000000 ) ) ;
#9484 = FACE_OUTER_BOUND ( 'NONE', #32292, .T. ) ;
#9486 = EDGE_LOOP ( 'NONE', ( #33046, #20573 ) ) ;
#9487 = CIRCLE ( 'NONE', #20677, 20.00000000000000355 ) ;
#9488 = AXIS2_PLACEMENT_3D ( 'NONE', #22712, #6091, #13521 ) ;
#9489 = CIRCLE ( 'NONE', #14405, 116.0000000000000000 ) ;
#9490 = EDGE_CURVE ( 'NONE', #12068, #15962, #25975, .T. ) ;
#9491 = DIRECTION ( 'NONE',  ( 0.000000000000000000, 0.000000000000000000, 1.000000000000000000 ) ) ;
#9492 = AXIS2_PLACEMENT_3D ( 'NONE', #14938, #25404, #28241 ) ;
#9493 = ORIENTED_EDGE ( 'NONE', *, *, #26875, .F. ) ;
#9494 = DIRECTION ( 'NONE',  ( -1.000000000000000000, 0.000000000000000000, 0.000000000000000000 ) ) ;
#9495 = DIRECTION ( 'NONE',  ( -1.000000000000000000, 0.000000000000000000, 0.000000000000000000 ) ) ;
#9496 = CARTESIAN_POINT ( 'NONE',  ( 96.56285295106283684, 31.00000000000000000, 12.84127866191736977 ) ) ;
#9498 = CARTESIAN_POINT ( 'NONE',  ( -73.90312034494817794, 40.00000000000000711, -56.84521418463217657 ) ) ;
#9497 =( GEOMETRIC_REPRESENTATION_CONTEXT ( 3 ) GLOBAL_UNCERTAINTY_ASSIGNED_CONTEXT ( ( #13462 ) ) GLOBAL_UNIT_ASSIGNED_CONTEXT ( ( #13282, #35934, #19620 ) ) REPRESENTATION_CONTEXT ( 'NONE', 'WORKASPACE' ) );
#9499 = CYLINDRICAL_SURFACE ( 'NONE', #14948, 31.49899999999999878 ) ;
#9500 = AXIS2_PLACEMENT_3D ( 'NONE', #17232, #23980, #800 ) ;
#9501 = EDGE_CURVE ( 'NONE', #9086, #28134, #36821, .T. ) ;
#9502 = CARTESIAN_POINT ( 'NONE',  ( 0.000000000000000000, -24.22031524825905890, -109.5520369638039710 ) ) ;
#9503 = VERTEX_POINT ( 'NONE', #33347 ) ;
#9504 = DIRECTION ( 'NONE',  ( 0.000000000000000000, 0.000000000000000000, 1.000000000000000000 ) ) ;
#9505 = ORIENTED_EDGE ( 'NONE', *, *, #4407, .F. ) ;
#9506 = DIRECTION ( 'NONE',  ( 0.000000000000000000, 0.7164567402983162969, -0.6976315211349835010 ) ) ;
#9507 = ADVANCED_FACE ( 'NONE', ( #3429 ), #3637, .F. ) ;
#9508 = VECTOR ( 'NONE', #28932, 1000.000000000000000 ) ;
#9509 = CARTESIAN_POINT ( 'NONE',  ( -2.649999999999993694, 150.5000000000000284, 6.999999999999998224 ) ) ;
#9510 = DIRECTION ( 'NONE',  ( -1.000000000000000000, 0.000000000000000000, 0.000000000000000000 ) ) ;
#9511 = ORIENTED_EDGE ( 'NONE', *, *, #34556, .F. ) ;
#9512 = DIRECTION ( 'NONE',  ( 1.000000000000000000, 0.000000000000000000, 0.000000000000000000 ) ) ;
#9513 = FACE_OUTER_BOUND ( 'NONE', #32814, .T. ) ;
#9514 = CARTESIAN_POINT ( 'NONE',  ( 4.000000000000000000, -2.511475576507276042, -3.469253905236643565 ) ) ;
#9516 = ORIENTED_EDGE ( 'NONE', *, *, #37648, .T. ) ;
#9515 = DIRECTION ( 'NONE',  ( -1.000000000000000000, 0.000000000000000000, 0.000000000000000000 ) ) ;
#9517 = DIRECTION ( 'NONE',  ( 0.000000000000000000, -0.2113826236296113270, -0.9774033898178695612 ) ) ;
#9518 = CARTESIAN_POINT ( 'NONE',  ( 0.000000000000000000, -51.19683565102450729, 9.104066087303294807 ) ) ;
#9519 = EDGE_CURVE ( 'NONE', #10645, #10921, #13942, .T. ) ;
#9520 = VECTOR ( 'NONE', #14357, 1000.000000000000000 ) ;
#9521 = AXIS2_PLACEMENT_3D ( 'NONE', #18332, #38341, #35068 ) ;
#9522 = CIRCLE ( 'NONE', #15141, 59.00000000000000000 ) ;
#9524 = ORIENTED_EDGE ( 'NONE', *, *, #34270, .F. ) ;
#9523 = LINE ( 'NONE', #9296, #22385 ) ;
#9525 = ORIENTED_EDGE ( 'NONE', *, *, #1654, .T. ) ;
#9526 = CARTESIAN_POINT ( 'NONE',  ( 17.99999999999999645, -25.46650492921884279, -19.29328419707811193 ) ) ;
#9527 = CARTESIAN_POINT ( 'NONE',  ( 17.99999999999999645, -112.8457601792513714, -26.86697618949492039 ) ) ;
#9528 = CARTESIAN_POINT ( 'NONE',  ( -24.78443185004241656, 40.00000000000000000, 32.19086620116434005 ) ) ;
#9529 = AXIS2_PLACEMENT_3D ( 'NONE', #11446, #28478, #5315 ) ;
#9530 = DIRECTION ( 'NONE',  ( -1.000000000000000000, 0.000000000000000000, 0.000000000000000000 ) ) ;
#9531 = ADVANCED_FACE ( 'NONE', ( #33989 ), #4075, .F. ) ;
#9532 = EDGE_CURVE ( 'NONE', #21659, #38310, #17881, .T. ) ;
#9533 = CIRCLE ( 'NONE', #31844, 116.0000000000000000 ) ;
#9534 = CARTESIAN_POINT ( 'NONE',  ( 17.99999999999999645, -3.996885678772183592, -120.4346956066682424 ) ) ;
#9535 = EDGE_CURVE ( 'NONE', #32579, #32669, #7132, .T. ) ;
#9536 = EDGE_CURVE ( 'NONE', #1383, #39440, #37678, .T. ) ;
#9537 = CARTESIAN_POINT ( 'NONE',  ( 4.999999999999997335, 0.000000000000000000, 4.250000000000000000 ) ) ;
#9538 = ORIENTED_EDGE ( 'NONE', *, *, #18626, .F. ) ;
#9539 = DIRECTION ( 'NONE',  ( -1.000000000000000000, 0.000000000000000000, 0.000000000000000000 ) ) ;
#9541 = ORIENTED_EDGE ( 'NONE', *, *, #6605, .T. ) ;
#9540 = CIRCLE ( 'NONE', #2532, 20.00000000000000355 ) ;
#9542 = FACE_OUTER_BOUND ( 'NONE', #37513, .T. ) ;
#9543 = CARTESIAN_POINT ( 'NONE',  ( 0.3000000000000028200, -14.69693845669907084, 0.000000000000000000 ) ) ;
#9544 = CIRCLE ( 'NONE', #33922, 19.19999999999999574 ) ;
#9545 = CARTESIAN_POINT ( 'NONE',  ( 23.39270017067629936, 31.00000000000000355, 40.49502024156475244 ) ) ;
#9546 = LINE ( 'NONE', #19185, #1628 ) ;
#9547 = ORIENTED_EDGE ( 'NONE', *, *, #3409, .T. ) ;
#9548 = PRODUCT_DEFINITION_SHAPE ( 'NONE', 'NONE',  #35852 ) ;
#9549 = CARTESIAN_POINT ( 'NONE',  ( 17.99999999999999645, -30.74337109795213863, -8.695908345466433431 ) ) ;
#9550 = CARTESIAN_POINT ( 'NONE',  ( -6.054110834496889026, 31.00000000000000355, -92.39583333400220511 ) ) ;
#9551 = CARTESIAN_POINT ( 'NONE',  ( 0.000000000000000000, 119.8996782608631406, -12.02323392193236629 ) ) ;
#9553 = ORIENTED_EDGE ( 'NONE', *, *, #16121, .T. ) ;
#9552 = CIRCLE ( 'NONE', #38813, 116.0000000000000000 ) ;
#9554 = CARTESIAN_POINT ( 'NONE',  ( 52.50410707182467718, 31.00000000000000000, -40.15145572480454916 ) ) ;
#9555 = CARTESIAN_POINT ( 'NONE',  ( -31.81746463534672387, 40.00000000000000000, -55.29958784370776925 ) ) ;
#9556 = LINE ( 'NONE', #15917, #18343 ) ;
#9557 = CIRCLE ( 'NONE', #3231, 47.49900000000000944 ) ;
#9558 = AXIS2_PLACEMENT_3D ( 'NONE', #26001, #36647, #39062 ) ;
#9559 = ORIENTED_EDGE ( 'NONE', *, *, #37927, .F. ) ;
#9560 = CIRCLE ( 'NONE', #21451, 120.5010000000000190 ) ;
#9561 = AXIS2_PLACEMENT_3D ( 'NONE', #22432, #41811, #11958 ) ;
#9562 = CARTESIAN_POINT ( 'NONE',  ( 18.00000000000000355, -39.64889472655706726, -33.64468972902550092 ) ) ;
#9563 = DIRECTION ( 'NONE',  ( -1.000000000000000000, -0.000000000000000000, 0.000000000000000000 ) ) ;
#9565 = ORIENTED_EDGE ( 'NONE', *, *, #20142, .F. ) ;
#9564 = CARTESIAN_POINT ( 'NONE',  ( 0.000000000000000000, -29.02167576844178853, 108.3790330702168774 ) ) ;
#9567 = AXIS2_PLACEMENT_3D ( 'NONE', #17528, #4829, #37549 ) ;
#9566 = CARTESIAN_POINT ( 'NONE',  ( 9.000000000000001776, 107.1354928292875996, -44.47455650397954230 ) ) ;
#9568 = CARTESIAN_POINT ( 'NONE',  ( 23.00000000000000000, 2.816687638038912352E-15, -6.000000000000000000 ) ) ;
#9569 = AXIS2_PLACEMENT_3D ( 'NONE', #12712, #6144, #15777 ) ;
#9570 = CARTESIAN_POINT ( 'NONE',  ( 46.64447153568531945, 40.00000000000000000, 60.78881617101084345 ) ) ;
#9571 = DIRECTION ( 'NONE',  ( -1.000000000000000000, 0.000000000000000000, 0.000000000000000000 ) ) ;
#9572 = CIRCLE ( 'NONE', #34640, 120.5010000000000190 ) ;
#9573 = ORIENTED_EDGE ( 'NONE', *, *, #42762, .F. ) ;
#9574 = DIRECTION ( 'NONE',  ( -1.000000000000000000, 0.000000000000000000, 0.000000000000000000 ) ) ;
#9575 = DIRECTION ( 'NONE',  ( 1.000000000000000000, 0.000000000000000000, 0.000000000000000000 ) ) ;
#9576 = VERTEX_POINT ( 'NONE', #27900 ) ;
#9577 = VERTEX_POINT ( 'NONE', #31580 ) ;
#9578 = LINE ( 'NONE', #13514, #2357 ) ;
#9579 = ORIENTED_EDGE ( 'NONE', *, *, #956, .T. ) ;
#9580 = DIRECTION ( 'NONE',  ( 1.000000000000000000, 0.000000000000000000, 0.000000000000000000 ) ) ;
#9581 = DIRECTION ( 'NONE',  ( -1.000000000000000000, 1.373900992973642066E-15, 4.525365589504737954E-16 ) ) ;
#9582 = AXIS2_PLACEMENT_3D ( 'NONE', #28901, #35828, #38473 ) ;
#9583 = CARTESIAN_POINT ( 'NONE',  ( 0.000000000000000000, 29.60891106212838508, -37.14118181634735549 ) ) ;
#9584 = EDGE_CURVE ( 'NONE', #38581, #17370, #42655, .T. ) ;
#9585 = ADVANCED_FACE ( 'NONE', ( #24861 ), #21156, .F. ) ;
#9586 = CARTESIAN_POINT ( 'NONE',  ( 0.000000000000000000, -41.62036691425451096, -113.0850832732718914 ) ) ;
#9587 = VERTEX_POINT ( 'NONE', #31803 ) ;
#9588 = AXIS2_PLACEMENT_3D ( 'NONE', #21245, #37123, #10734 ) ;
#9589 = DIRECTION ( 'NONE',  ( -1.000000000000000000, 0.000000000000000000, -0.000000000000000000 ) ) ;
#9590 = AXIS2_PLACEMENT_3D ( 'NONE', #2150, #21437, #1302 ) ;
#9591 = EDGE_CURVE ( 'NONE', #17334, #17987, #37811, .T. ) ;
#9592 = ORIENTED_EDGE ( 'NONE', *, *, #38807, .F. ) ;
#9593 = CIRCLE ( 'NONE', #42304, 31.49900000000000588 ) ;
#9594 = CARTESIAN_POINT ( 'NONE',  ( 6.999999999999999112, 7.118024431592597790E-15, 0.000000000000000000 ) ) ;
#9595 = VERTEX_POINT ( 'NONE', #38532 ) ;
#9596 = CARTESIAN_POINT ( 'NONE',  ( 0.000000000000000000, -150.5000000000000284, 9.999999999999998224 ) ) ;
#9597 = VECTOR ( 'NONE', #32156, 1000.000000000000114 ) ;
#9598 = DIRECTION ( 'NONE',  ( -1.000000000000000000, 0.000000000000000000, 0.000000000000000000 ) ) ;
#9599 = ITEM_DEFINED_TRANSFORMATION ( 'NONE', 'NONE', #39281,  #13552 ) ;
#9600 = DIRECTION ( 'NONE',  ( 0.000000000000000000, 0.000000000000000000, 1.000000000000000000 ) ) ;
#9601 = CARTESIAN_POINT ( 'NONE',  ( -56.43872490705654599, 31.00000000000000711, 19.17141758013517716 ) ) ;
#9602 = CIRCLE ( 'NONE', #39538, 13.40000000000000213 ) ;
#9603 = ADVANCED_FACE ( 'NONE', ( #28332 ), #34404, .T. ) ;
#9604 = ORIENTED_EDGE ( 'NONE', *, *, #33858, .F. ) ;
#9605 = CARTESIAN_POINT ( 'NONE',  ( -15.23573235977617379, 31.00000000000000355, 26.30445775087292404 ) ) ;
#9606 = CARTESIAN_POINT ( 'NONE',  ( -45.35818215263140019, 40.00000000000000000, 51.72168634911185592 ) ) ;
#9607 = CARTESIAN_POINT ( 'NONE',  ( 17.99999999999999645, -110.1579703617967567, 21.29539948940213634 ) ) ;
#9608 = LINE ( 'NONE', #3666, #35365 ) ;
#9609 = VECTOR ( 'NONE', #13135, 1000.000000000000000 ) ;
#9610 = CARTESIAN_POINT ( 'NONE',  ( 17.99999999999999645, -12.43843445475394027, 111.5058645182329116 ) ) ;
#9611 = EDGE_CURVE ( 'NONE', #34305, #27015, #10637, .T. ) ;
#9612 = DIRECTION ( 'NONE',  ( 0.000000000000000000, -0.6736956436465636466, 0.7390089172206532053 ) ) ;
#9613 = CIRCLE ( 'NONE', #20814, 13.60000000000000142 ) ;
#9614 = AXIS2_PLACEMENT_3D ( 'NONE', #36096, #23261, #13007 ) ;
#9615 = VERTEX_POINT ( 'NONE', #14808 ) ;
#9616 = CARTESIAN_POINT ( 'NONE',  ( 39.77940265867437120, 40.00000000000000000, 22.96373720238702276 ) ) ;
#9617 = CIRCLE ( 'NONE', #15939, 116.0000000000000000 ) ;
#9618 = DIRECTION ( 'NONE',  ( 0.000000000000000000, 0.000000000000000000, -1.000000000000000000 ) ) ;
#9619 = CARTESIAN_POINT ( 'NONE',  ( 17.99999999999999645, 0.04937522221122418731, 31.94951095880159286 ) ) ;
#9620 = AXIS2_PLACEMENT_3D ( 'NONE', #7076, #10578, #31307 ) ;
#9621 = ORIENTED_EDGE ( 'NONE', *, *, #16089, .F. ) ;
#9622 = LINE ( 'NONE', #11902, #13394 ) ;
#9623 = CIRCLE ( 'NONE', #1954, 0.08402000000000062196 ) ;
#9624 = DIRECTION ( 'NONE',  ( -1.000000000000000000, -0.000000000000000000, -0.000000000000000000 ) ) ;
#9625 = ORIENTED_EDGE ( 'NONE', *, *, #11978, .F. ) ;
#9626 = CARTESIAN_POINT ( 'NONE',  ( 0.000000000000000000, -25.46650492921910924, 19.29328419707777087 ) ) ;
#9627 = ORIENTED_EDGE ( 'NONE', *, *, #27639, .T. ) ;
#9628 = VERTEX_POINT ( 'NONE', #5393 ) ;
#9629 = CARTESIAN_POINT ( 'NONE',  ( 17.99999999999999645, -16.77566611177701006, -119.3275660838943963 ) ) ;
#9630 = CARTESIAN_POINT ( 'NONE',  ( -59.98614492175870794, 31.00000000000000711, 68.21249229744711329 ) ) ;
#9631 = ORIENTED_EDGE ( 'NONE', *, *, #16170, .F. ) ;
#9632 = CYLINDRICAL_SURFACE ( 'NONE', #35626, 120.5010000000000190 ) ;
#9633 = CARTESIAN_POINT ( 'NONE',  ( 130.0000000000000568, -2.127378845942283338E-13, -39.99999999999995026 ) ) ;
#9634 = EDGE_CURVE ( 'NONE', #30173, #1677, #165, .T. ) ;
#9635 = DIRECTION ( 'NONE',  ( -1.000000000000000000, -0.000000000000000000, 0.000000000000000000 ) ) ;
#9636 = ORIENTED_EDGE ( 'NONE', *, *, #42670, .T. ) ;
#9637 = DIRECTION ( 'NONE',  ( -1.000000000000000000, -0.000000000000000000, -0.000000000000000000 ) ) ;
#9638 = DIRECTION ( 'NONE',  ( -1.000000000000000000, 0.000000000000000000, -0.000000000000000000 ) ) ;
#9639 = CIRCLE ( 'NONE', #14529, 12.59999999999999964 ) ;
#9640 = AXIS2_PLACEMENT_3D ( 'NONE', #17281, #41652, #15075 ) ;
#9642 = CARTESIAN_POINT ( 'NONE',  ( 2.500000000000000000, 1.178949249685212974, -2.042000000000001148 ) ) ;
#9641 = DIRECTION ( 'NONE',  ( 1.000000000000000000, 0.000000000000000000, 0.000000000000000000 ) ) ;
#9643 = EDGE_CURVE ( 'NONE', #30408, #27215, #16226, .T. ) ;
#9644 = CARTESIAN_POINT ( 'NONE',  ( 17.99999999999999645, -34.03109950475653989, -115.5957406979053133 ) ) ;
#9645 = CIRCLE ( 'NONE', #22217, 19.19999999999999574 ) ;
#9646 = ORIENTED_EDGE ( 'NONE', *, *, #39699, .F. ) ;
#9647 = EDGE_CURVE ( 'NONE', #2925, #23705, #5734, .T. ) ;
#9648 = CARTESIAN_POINT ( 'NONE',  ( 2.127120017302678523, 31.00000000000000355, -32.60416666460785962 ) ) ;
#9649 = AXIS2_PLACEMENT_3D ( 'NONE', #42799, #20171, #33432 ) ;
#9650 = ORIENTED_EDGE ( 'NONE', *, *, #19399, .T. ) ;
#9651 = DIRECTION ( 'NONE',  ( 0.000000000000000000, 0.9957341762950341346, 0.09226835946330559646 ) ) ;
#9652 = ADVANCED_FACE ( 'NONE', ( #25286 ), #4746, .F. ) ;
#9653 = CARTESIAN_POINT ( 'NONE',  ( -10.00000000000000000, 0.000000000000000000, 0.000000000000000000 ) ) ;
#9654 = ORIENTED_EDGE ( 'NONE', *, *, #40797, .T. ) ;
#9655 = CARTESIAN_POINT ( 'NONE',  ( 0.000000000000000000, -40.13512380273891011, -113.6206972269525863 ) ) ;
#9656 = CARTESIAN_POINT ( 'NONE',  ( 34.89583333524210218, 40.00000000000000000, -2.290744634698907767 ) ) ;
#9657 = CARTESIAN_POINT ( 'NONE',  ( 21.53706125533296500, 40.00000000000000000, 43.87245753945351368 ) ) ;
#9658 = ORIENTED_EDGE ( 'NONE', *, *, #42203, .F. ) ;
#9659 = ORIENTED_EDGE ( 'NONE', *, *, #26038, .T. ) ;
#9660 = DIRECTION ( 'NONE',  ( 0.000000000000000000, 0.000000000000000000, 1.000000000000000000 ) ) ;
#9661 = DIRECTION ( 'NONE',  ( 0.000000000000000000, 0.000000000000000000, 1.000000000000000000 ) ) ;
#9662 = DIRECTION ( 'NONE',  ( 0.000000000000000000, 0.000000000000000000, 1.000000000000000000 ) ) ;
#9664 = EDGE_CURVE ( 'NONE', #5593, #27822, #40569, .T. ) ;
#9663 = DIRECTION ( 'NONE',  ( 0.000000000000000000, 0.000000000000000000, 1.000000000000000000 ) ) ;
#9665 = DIRECTION ( 'NONE',  ( 0.000000000000000000, 0.000000000000000000, 1.000000000000000000 ) ) ;
#9666 = VERTEX_POINT ( 'NONE', #35054 ) ;
#9667 = CARTESIAN_POINT ( 'NONE',  ( 0.000000000000000000, -44.75336757549769118, -14.30704879393654316 ) ) ;
#9668 = EDGE_LOOP ( 'NONE', ( #11309, #22460, #12446, #8763 ) ) ;
#9669 = CYLINDRICAL_SURFACE ( 'NONE', #20906, 13.59999999999999964 ) ;
#9670 = ADVANCED_FACE ( 'NONE', ( #34629 ), #24424, .T. ) ;
#9671 = DIRECTION ( 'NONE',  ( -0.000000000000000000, -0.000000000000000000, 1.000000000000000000 ) ) ;
#9672 = AXIS2_PLACEMENT_3D ( 'NONE', #29700, #3254, #36870 ) ;
#9673 = CIRCLE ( 'NONE', #15293, 58.99999999999999289 ) ;
#9674 = DIRECTION ( 'NONE',  ( -1.000000000000000000, 0.000000000000000000, 0.000000000000000000 ) ) ;
#9675 = CARTESIAN_POINT ( 'NONE',  ( -10.00000000000000000, 0.000000000000000000, 0.000000000000000000 ) ) ;
#9676 = ORIENTED_EDGE ( 'NONE', *, *, #41591, .T. ) ;
#9677 = DIRECTION ( 'NONE',  ( -1.000000000000000000, 0.000000000000000000, 0.000000000000000000 ) ) ;
#9678 = ORIENTED_EDGE ( 'NONE', *, *, #20978, .F. ) ;
#9679 = CIRCLE ( 'NONE', #32662, 12.59999999999999964 ) ;
#9680 = DIRECTION ( 'NONE',  ( -1.000000000000000000, -0.000000000000000000, -0.000000000000000000 ) ) ;
#9681 = ORIENTED_EDGE ( 'NONE', *, *, #26998, .F. ) ;
#9683 = ORIENTED_EDGE ( 'NONE', *, *, #8070, .T. ) ;
#9682 = DIRECTION ( 'NONE',  ( 0.000000000000000000, 0.5877852522924742473, -0.8090169943749466741 ) ) ;
#9684 = CARTESIAN_POINT ( 'NONE',  ( -3.998040010416403334, 31.00000000000000355, 59.59469406578620720 ) ) ;
#9685 = ORIENTED_EDGE ( 'NONE', *, *, #34517, .T. ) ;
#9686 = CARTESIAN_POINT ( 'NONE',  ( -91.96080130434580724, -40.05525454449572464, 14.45886780445738218 ) ) ;
#9687 = ADVANCED_FACE ( 'NONE', ( #41816 ), #1249, .F. ) ;
#9688 = ORIENTED_EDGE ( 'NONE', *, *, #37907, .T. ) ;
#9689 = CARTESIAN_POINT ( 'NONE',  ( 17.99999999999999645, 0.000000000000000000, 0.000000000000000000 ) ) ;
#9690 = ORIENTED_EDGE ( 'NONE', *, *, #10949, .F. ) ;
#9691 = CARTESIAN_POINT ( 'NONE',  ( -20.82795069772234342, 40.00000000000000000, 77.32795358076222669 ) ) ;
#9693 = CARTESIAN_POINT ( 'NONE',  ( 17.99999999999999645, -69.90696807222551001, 98.15042952503490881 ) ) ;
#9692 = CARTESIAN_POINT ( 'NONE',  ( 18.00000000000000355, 44.61570720899074161, 14.73072383765644133 ) ) ;
#9694 = DIRECTION ( 'NONE',  ( 0.000000000000000000, 0.6736956436465532105, 0.7390089172206629753 ) ) ;
#9695 = VERTEX_POINT ( 'NONE', #2725 ) ;
#9696 = LINE ( 'NONE', #33668, #7726 ) ;
#9697 = VERTEX_POINT ( 'NONE', #16524 ) ;
#9698 = EDGE_CURVE ( 'NONE', #18411, #31896, #28097, .T. ) ;
#9699 = DIRECTION ( 'NONE',  ( -1.000000000000000000, -0.000000000000000000, -0.000000000000000000 ) ) ;
#9700 = CYLINDRICAL_SURFACE ( 'NONE', #12217, 125.9999999999993605 ) ;
#9701 = CARTESIAN_POINT ( 'NONE',  ( -80.10416666582359824, 31.00000000000000711, -5.235987747607834031 ) ) ;
#9702 = AXIS2_PLACEMENT_3D ( 'NONE', #27622, #28277, #38062 ) ;
#9704 = CARTESIAN_POINT ( 'NONE',  ( 17.99999999999999645, -116.4607004671426438, -30.94182036827323756 ) ) ;
#9703 = CARTESIAN_POINT ( 'NONE',  ( 5.991980000000000750, 0.000000000000000000, 0.000000000000000000 ) ) ;
#9705 = TOROIDAL_SURFACE ( 'NONE', #37571, 11.08000000000000007, 0.08000000000000020983 ) ;
#9706 = ORIENTED_EDGE ( 'NONE', *, *, #24960, .F. ) ;
#9707 = EDGE_CURVE ( 'NONE', #30260, #19475, #12765, .T. ) ;
#9708 = CIRCLE ( 'NONE', #3390, 10.99999999999999645 ) ;
#9709 = CARTESIAN_POINT ( 'NONE',  ( 17.99999999999999645, 28.35267316522783432, 22.18391138608718549 ) ) ;
#9710 = ORIENTED_EDGE ( 'NONE', *, *, #14381, .F. ) ;
#9711 = CARTESIAN_POINT ( 'NONE',  ( 17.99999999999999645, -12.43843445475238063, -111.5058645182330963 ) ) ;
#9712 = CYLINDRICAL_SURFACE ( 'NONE', #31119, 47.49900000000000233 ) ;
#9713 = CARTESIAN_POINT ( 'NONE',  ( 49.34100556531812742, 31.00000000000000355, 85.68208892729249726 ) ) ;
#9714 = CARTESIAN_POINT ( 'NONE',  ( 73.86091552542920624, 39.99999999999999289, 64.94433634442138725 ) ) ;
#9715 = FACE_OUTER_BOUND ( 'NONE', #16897, .T. ) ;
#9716 = CARTESIAN_POINT ( 'NONE',  ( 5.000000000000002665, 3.306546357697854226E-16, 2.700000000000000622 ) ) ;
#9717 = ORIENTED_EDGE ( 'NONE', *, *, #42169, .F. ) ;
#9718 = CYLINDRICAL_SURFACE ( 'NONE', #1920, 20.00000000000000355 ) ;
#9719 = ORIENTED_EDGE ( 'NONE', *, *, #42636, .T. ) ;
#9720 = ADVANCED_FACE ( 'NONE', ( #25712 ), #23081, .F. ) ;
#9721 = CARTESIAN_POINT ( 'NONE',  ( 0.000000000000000000, 31.81777574834305966, -2.898764365605425830 ) ) ;
#9722 = EDGE_CURVE ( 'NONE', #22119, #35461, #36121, .T. ) ;
#9723 = DIRECTION ( 'NONE',  ( -1.000000000000000000, 0.000000000000000000, 0.000000000000000000 ) ) ;
#9724 = CARTESIAN_POINT ( 'NONE',  ( 0.000000000000000000, 18.53613841426857434, -48.58406706613883586 ) ) ;
#9725 = VERTEX_POINT ( 'NONE', #42654 ) ;
#9726 = CARTESIAN_POINT ( 'NONE',  ( 8.999999999999998224, 0.6168405712486720871, 35.99471499692226928 ) ) ;
#9727 = CYLINDRICAL_SURFACE ( 'NONE', #3956, 116.0000000000000000 ) ;
#9728 = DIRECTION ( 'NONE',  ( -1.000000000000000000, 0.000000000000000000, 0.000000000000000000 ) ) ;
#9730 = VERTEX_POINT ( 'NONE', #39382 ) ;
#9729 = CARTESIAN_POINT ( 'NONE',  ( 17.99999999999999645, 103.4151313792879421, -61.85306461934305844 ) ) ;
#9731 = CARTESIAN_POINT ( 'NONE',  ( 17.75583184595726749, 31.00000000000000355, -30.63479189996604646 ) ) ;
#9732 = AXIS2_PLACEMENT_3D ( 'NONE', #20187, #16695, #33880 ) ;
#9733 = CARTESIAN_POINT ( 'NONE',  ( 17.99999999999999645, 0.000000000000000000, 0.000000000000000000 ) ) ;
#9735 = VERTEX_POINT ( 'NONE', #19161 ) ;
#9734 = DIRECTION ( 'NONE',  ( -1.000000000000000000, -0.000000000000000000, 0.000000000000000000 ) ) ;
#9736 = ORIENTED_EDGE ( 'NONE', *, *, #42433, .F. ) ;
#9737 = DIRECTION ( 'NONE',  ( -1.000000000000000000, 0.000000000000000000, 0.000000000000000000 ) ) ;
#9738 = CARTESIAN_POINT ( 'NONE',  ( 0.000000000000000000, -25.61928775981074935, 45.25098998563468911 ) ) ;
#9739 = CARTESIAN_POINT ( 'NONE',  ( -52.09564885855072447, 40.00000000000000000, -3.498939618562995513 ) ) ;
#9740 = CARTESIAN_POINT ( 'NONE',  ( 17.99999999999999645, -115.9750404417043939, -2.406240749598616446 ) ) ;
#9741 = CARTESIAN_POINT ( 'NONE',  ( -3.511755186886750479, 2.826662030176366081, -3.597382984111578086 ) ) ;
#9742 = CARTESIAN_POINT ( 'NONE',  ( 3.333333333333335702, -2.694301256218268215, -3.300726591567084256 ) ) ;
#9743 = ORIENTED_EDGE ( 'NONE', *, *, #19512, .T. ) ;
#9744 = CARTESIAN_POINT ( 'NONE',  ( 17.99999999999999645, -47.58001226230465619, -110.7096808509488284 ) ) ;
#9745 = ORIENTED_EDGE ( 'NONE', *, *, #3638, .T. ) ;
#9746 = EDGE_CURVE ( 'NONE', #17173, #24522, #39604, .T. ) ;
#9747 = DIRECTION ( 'NONE',  ( 1.000000000000000000, 0.000000000000000000, 0.000000000000000000 ) ) ;
#9748 = DIRECTION ( 'NONE',  ( -1.000000000000000000, -0.000000000000000000, 0.000000000000000000 ) ) ;
#9749 = EDGE_CURVE ( 'NONE', #26054, #42401, #12804, .T. ) ;
#9750 = CARTESIAN_POINT ( 'NONE',  ( -50.10416666532988472, 31.00000000000000355, -3.272492339034341224 ) ) ;
#9751 = CYLINDRICAL_SURFACE ( 'NONE', #23252, 59.00000000000000000 ) ;
#9752 = VERTEX_POINT ( 'NONE', #9518 ) ;
#9753 = CARTESIAN_POINT ( 'NONE',  ( 0.000000000000000000, -79.18387647320706435, -84.76976882518842160 ) ) ;
#9754 = CARTESIAN_POINT ( 'NONE',  ( 43.43872713698582544, 31.00000000000000355, 75.20828420317944563 ) ) ;
#9755 = CIRCLE ( 'NONE', #32095, 120.5010000000000332 ) ;
#9756 = CIRCLE ( 'NONE', #17467, 116.0000000000000000 ) ;
#9757 = LINE ( 'NONE', #32459, #22704 ) ;
#9758 = ORIENTED_EDGE ( 'NONE', *, *, #6366, .T. ) ;
#9759 = CARTESIAN_POINT ( 'NONE',  ( -58.36801134197498442, 31.00000000000000711, 19.71467013092928866 ) ) ;
#9760 = CARTESIAN_POINT ( 'NONE',  ( -61.79211991639481028, 40.00000000000000711, -8.240724169186190551 ) ) ;
#9761 = CARTESIAN_POINT ( 'NONE',  ( 6.381360069253262601, 40.00000000000000000, 97.39583333395333398 ) ) ;
#9762 = ORIENTED_EDGE ( 'NONE', *, *, #27157, .F. ) ;
#9763 = DIRECTION ( 'NONE',  ( -1.000000000000000000, 0.000000000000000000, 0.000000000000000000 ) ) ;
#9764 = EDGE_CURVE ( 'NONE', #6594, #34488, #1592, .T. ) ;
#9765 = CARTESIAN_POINT ( 'NONE',  ( 17.99999999999999645, 24.22031524825977300, 109.5520369638038289 ) ) ;
#9766 = DIRECTION ( 'NONE',  ( 0.000000000000000000, 0.7980172272802363853, 0.6026346363792605132 ) ) ;
#9767 = EDGE_CURVE ( 'NONE', #34370, #21317, #15659, .T. ) ;
#9768 = ADVANCED_FACE ( 'NONE', ( #22875 ), #33062, .T. ) ;
#9769 = ADVANCED_FACE ( 'NONE', ( #2934 ), #29183, .T. ) ;
#9771 = VERTEX_POINT ( 'NONE', #29598 ) ;
#9770 = CARTESIAN_POINT ( 'NONE',  ( 9.000000000000001776, -98.69720329640996681, 60.94966826379877745 ) ) ;
#9772 = CYLINDRICAL_SURFACE ( 'NONE', #17073, 13.59999999999999787 ) ;
#9773 = ORIENTED_EDGE ( 'NONE', *, *, #4057, .T. ) ;
#9774 = CARTESIAN_POINT ( 'NONE',  ( 17.99999999999999645, 3.996885678773026029, 120.4346956066682424 ) ) ;
#9775 = CARTESIAN_POINT ( 'NONE',  ( 57.37208743749949491, 40.00000000000000000, 50.31438278193533620 ) ) ;
#9776 = CYLINDRICAL_SURFACE ( 'NONE', #37511, 2.649999999999957723 ) ;
#9777 = ORIENTED_EDGE ( 'NONE', *, *, #16267, .F. ) ;
#9778 = AXIS2_PLACEMENT_3D ( 'NONE', #41884, #5668, #29253 ) ;
#9779 = DIRECTION ( 'NONE',  ( 0.000000000000000000, 0.000000000000000000, 1.000000000000000000 ) ) ;
#9780 = CARTESIAN_POINT ( 'NONE',  ( 0.000000000000000000, -88.00363688980490906, -82.31555682352745862 ) ) ;
#9781 = ORIENTED_EDGE ( 'NONE', *, *, #6964, .F. ) ;
#9782 = CIRCLE ( 'NONE', #9096, 47.49899999999999523 ) ;
#9783 = ORIENTED_EDGE ( 'NONE', *, *, #4701, .F. ) ;
#9784 = DIRECTION ( 'NONE',  ( 0.000000000000000000, 9.408669700213191589E-16, -1.000000000000000000 ) ) ;
#9786 = ORIENTED_EDGE ( 'NONE', *, *, #41838, .T. ) ;
#9785 = CIRCLE ( 'NONE', #37652, 52.00000000000000000 ) ;
#9787 = AXIS2_PLACEMENT_3D ( 'NONE', #7536, #29828, #14109 ) ;
#9788 = FACE_OUTER_BOUND ( 'NONE', #13036, .T. ) ;
#9789 = DIRECTION ( 'NONE',  ( -3.009274222672345096E-17, -1.000000000000000000, 2.455023325076454960E-18 ) ) ;
#9790 = AXIS2_PLACEMENT_3D ( 'NONE', #36862, #179, #6967 ) ;
#9791 = LINE ( 'NONE', #26812, #1821 ) ;
#9792 = VERTEX_POINT ( 'NONE', #12171 ) ;
#9793 = DIRECTION ( 'NONE',  ( -1.000000000000000000, 0.000000000000000000, -0.000000000000000000 ) ) ;
#9794 = VERTEX_POINT ( 'NONE', #25491 ) ;
#9795 = EDGE_CURVE ( 'NONE', #6539, #1566, #41294, .T. ) ;
#9796 = CYLINDRICAL_SURFACE ( 'NONE', #12727, 116.0000000000000000 ) ;
#9797 = CARTESIAN_POINT ( 'NONE',  ( -15.93581279029885422, 31.00000000000000355, -13.96891150189262021 ) ) ;
#9798 = ORIENTED_EDGE ( 'NONE', *, *, #7125, .F. ) ;
#9799 = DIRECTION ( 'NONE',  ( -1.000000000000000000, 0.000000000000000000, 0.000000000000000000 ) ) ;
#9800 = DIRECTION ( 'NONE',  ( 1.000000000000000000, 0.000000000000000000, 0.000000000000000000 ) ) ;
#9801 = PRODUCT_CONTEXT ( 'NONE', #767, 'mechanical' ) ;
#9802 = CARTESIAN_POINT ( 'NONE',  ( 0.000000000000000000, 0.000000000000000000, -5.000000000000000888 ) ) ;
#9803 = CARTESIAN_POINT ( 'NONE',  ( 18.36587843422771016, 31.00000000000000355, 54.06640964556338957 ) ) ;
#9804 = AXIS2_PLACEMENT_3D ( 'NONE', #36619, #3229, #33365 ) ;
#9805 = VERTEX_POINT ( 'NONE', #38751 ) ;
#9806 = CARTESIAN_POINT ( 'NONE',  ( -26.24023198663968515, 31.00000000000000355, -20.19409642360271917 ) ) ;
#9807 = CARTESIAN_POINT ( 'NONE',  ( -69.34045338167970840, 40.00000000000000711, 9.142281554609933636 ) ) ;
#9808 = AXIS2_PLACEMENT_3D ( 'NONE', #41564, #7973, #1633 ) ;
#9809 = AXIS2_PLACEMENT_3D ( 'NONE', #29550, #13199, #16252 ) ;
#9810 = VECTOR ( 'NONE', #10099, 1000.000000000000000 ) ;
#9811 = DIRECTION ( 'NONE',  ( 0.000000000000000000, 0.000000000000000000, 1.000000000000000000 ) ) ;
#9812 = ADVANCED_FACE ( 'NONE', ( #8881 ), #35480, .F. ) ;
#9813 = EDGE_CURVE ( 'NONE', #34600, #23370, #16075, .T. ) ;
#9814 = EDGE_CURVE ( 'NONE', #34305, #433, #27921, .T. ) ;
#9815 = DIRECTION ( 'NONE',  ( -1.000000000000000000, 0.000000000000000000, 0.000000000000000000 ) ) ;
#9816 = CARTESIAN_POINT ( 'NONE',  ( 8.999999999999998224, 1.543054966925665076E-15, 12.59999999999999964 ) ) ;
#9817 = ADVANCED_FACE ( 'NONE', ( #15880 ), #9294, .T. ) ;
#9818 = ORIENTED_EDGE ( 'NONE', *, *, #22519, .F. ) ;
#9819 = CARTESIAN_POINT ( 'NONE',  ( -38.92335646797288717, 40.00000000000000000, 29.86975225897632313 ) ) ;
#9820 = DIRECTION ( 'NONE',  ( -1.000000000000000000, -0.000000000000000000, 0.000000000000000000 ) ) ;
#9821 = DIRECTION ( 'NONE',  ( -1.058513553088275437E-16, -1.000000000000000000, 8.813324511995299047E-17 ) ) ;
#9822 = AXIS2_PLACEMENT_3D ( 'NONE', #39025, #2359, #15728 ) ;
#9823 = EDGE_LOOP ( 'NONE', ( #26961, #29977, #17627, #22621 ) ) ;
#9824 = DIRECTION ( 'NONE',  ( 0.000000000000000000, 0.05322217484217878214, -0.9985826956767620555 ) ) ;
#9825 = CARTESIAN_POINT ( 'NONE',  ( 17.99999999999999645, -2.007101075699733173, -31.43498920425971832 ) ) ;
#9826 = ORIENTED_EDGE ( 'NONE', *, *, #4165, .F. ) ;
#9827 = CARTESIAN_POINT ( 'NONE',  ( 17.99999999999999645, -103.1672962317648512, -44.09967643725973119 ) ) ;
#9828 = EDGE_CURVE ( 'NONE', #9154, #6244, #26524, .T. ) ;
#9829 = ORIENTED_EDGE ( 'NONE', *, *, #22749, .F. ) ;
#9830 = ORIENTED_EDGE ( 'NONE', *, *, #13395, .F. ) ;
#9831 = CARTESIAN_POINT ( 'NONE',  ( 142.4999999999992610, -1.771709463423323217E-13, 6.999999999999945821 ) ) ;
#9832 = EDGE_CURVE ( 'NONE', #7063, #15282, #37412, .T. ) ;
#9833 = CARTESIAN_POINT ( 'NONE',  ( -11.85673204380701939, 31.00000000000000355, 89.11174773313419450 ) ) ;
#9834 = ORIENTED_EDGE ( 'NONE', *, *, #8448, .T. ) ;
#9835 = DIRECTION ( 'NONE',  ( 0.000000000000000000, 0.000000000000000000, 1.000000000000000000 ) ) ;
#9836 = FACE_OUTER_BOUND ( 'NONE', #31839, .T. ) ;
#9837 = DIRECTION ( 'NONE',  ( 0.000000000000000000, -0.9968120070307493474, -0.07978610555309324781 ) ) ;
#9838 = ORIENTED_EDGE ( 'NONE', *, *, #16974, .F. ) ;
#9839 = DIRECTION ( 'NONE',  ( -1.000000000000000000, 0.000000000000000000, -0.000000000000000000 ) ) ;
#9840 = AXIS2_PLACEMENT_3D ( 'NONE', #23456, #23883, #33660 ) ;
#9841 = VECTOR ( 'NONE', #9401, 1000.000000000000000 ) ;
#9842 = DIRECTION ( 'NONE',  ( -1.058513553088275437E-16, -1.000000000000000000, 8.813324511995299047E-17 ) ) ;
#9844 = FACE_OUTER_BOUND ( 'NONE', #30417, .T. ) ;
#9843 = DIRECTION ( 'NONE',  ( 1.000000000000000000, 1.836909530733573776E-16, 0.000000000000000000 ) ) ;
#9845 = AXIS2_PLACEMENT_3D ( 'NONE', #19154, #29382, #39163 ) ;
#9846 = ADVANCED_FACE ( 'NONE', ( #39809 ), #37194, .F. ) ;
#9847 = CARTESIAN_POINT ( 'NONE',  ( 17.99999999999999645, -117.6086855750636460, 26.24286718912065552 ) ) ;
#9848 = ORIENTED_EDGE ( 'NONE', *, *, #16957, .F. ) ;
#9849 = CARTESIAN_POINT ( 'NONE',  ( -30.01493782828161017, 31.00000000000000355, -3.947526014606304035 ) ) ;
#9850 = AXIS2_PLACEMENT_3D ( 'NONE', #22399, #43053, #12763 ) ;
#9851 = ORIENTED_EDGE ( 'NONE', *, *, #26411, .F. ) ;
#9852 = CARTESIAN_POINT ( 'NONE',  ( 17.99999999999999645, -12.42760411676062127, 33.78690065568420664 ) ) ;
#9853 = DIRECTION ( 'NONE',  ( 0.000000000000000000, -0.8951632913550664483, 0.4457383557765300930 ) ) ;
#9854 = ORIENTED_EDGE ( 'NONE', *, *, #2501, .F. ) ;
#9855 = DIRECTION ( 'NONE',  ( 0.000000000000000000, 1.000000000000000000, 0.000000000000000000 ) ) ;
#9856 = CARTESIAN_POINT ( 'NONE',  ( 34.98270738856093232, 40.00000000000000000, 4.602016392115340970 ) ) ;
#9857 = CARTESIAN_POINT ( 'NONE',  ( -44.44570800418432555, 40.00000000000000000, 25.56477902013099524 ) ) ;
#9858 = ORIENTED_EDGE ( 'NONE', *, *, #33956, .T. ) ;
#9859 = EDGE_LOOP ( 'NONE', ( #30125, #13271, #32907, #33199 ) ) ;
#9860 = DIRECTION ( 'NONE',  ( 1.000000000000000000, 1.836909530733573776E-16, 0.000000000000000000 ) ) ;
#9861 = ADVANCED_FACE ( 'NONE', ( #86 ), #304, .F. ) ;
#9862 = CARTESIAN_POINT ( 'NONE',  ( 8.999999999999998224, 0.000000000000000000, 0.000000000000000000 ) ) ;
#9863 = EDGE_CURVE ( 'NONE', #12090, #13726, #9071, .T. ) ;
#9864 = CARTESIAN_POINT ( 'NONE',  ( 9.000000000000001776, -17.77780072541623113, -114.6296200873377842 ) ) ;
#9865 = LINE ( 'NONE', #9229, #5729 ) ;
#9866 = DIRECTION ( 'NONE',  ( -1.000000000000000000, -0.000000000000000000, -0.000000000000000000 ) ) ;
#9867 = ORIENTED_EDGE ( 'NONE', *, *, #20925, .T. ) ;
#9868 = DIRECTION ( 'NONE',  ( -1.000000000000000000, 0.000000000000000000, 0.000000000000000000 ) ) ;
#9869 = ORIENTED_EDGE ( 'NONE', *, *, #30853, .T. ) ;
#9870 = CYLINDRICAL_SURFACE ( 'NONE', #2699, 59.00000000000000000 ) ;
#9871 = CIRCLE ( 'NONE', #41946, 47.49900000000000233 ) ;
#9872 = DIRECTION ( 'NONE',  ( 1.000000000000000000, 0.000000000000000000, 0.000000000000000000 ) ) ;
#9873 = VECTOR ( 'NONE', #33300, 1000.000000000000000 ) ;
#9874 = VERTEX_POINT ( 'NONE', #23926 ) ;
#9875 = CARTESIAN_POINT ( 'NONE',  ( 17.99999999999999645, 107.5680526044919674, -31.89649718262133149 ) ) ;
#9876 = CIRCLE ( 'NONE', #42594, 4.500000000000002665 ) ;
#9877 = CYLINDRICAL_SURFACE ( 'NONE', #11550, 59.00000000000000000 ) ;
#9878 = ORIENTED_EDGE ( 'NONE', *, *, #31522, .T. ) ;
#9879 = DIRECTION ( 'NONE',  ( 0.000000000000000000, 0.000000000000000000, 1.000000000000000000 ) ) ;
#9880 = ORIENTED_EDGE ( 'NONE', *, *, #31649, .F. ) ;
#9881 = DIRECTION ( 'NONE',  ( 1.000000000000000000, 0.000000000000000000, 0.000000000000000000 ) ) ;
#9882 = EDGE_CURVE ( 'NONE', #10144, #5171, #18192, .T. ) ;
#9883 = ORIENTED_EDGE ( 'NONE', *, *, #9111, .F. ) ;
#9885 = EDGE_LOOP ( 'NONE', ( #19166, #9067, #37262 ) ) ;
#9884 = DIRECTION ( 'NONE',  ( 1.000000000000000000, -0.000000000000000000, -0.000000000000000000 ) ) ;
#9886 = EDGE_CURVE ( 'NONE', #14013, #41712, #22353, .T. ) ;
#9887 = CARTESIAN_POINT ( 'NONE',  ( -60.39136959358631174, 31.00000000000000711, -16.27924862579292054 ) ) ;
#9888 = ORIENTED_EDGE ( 'NONE', *, *, #41082, .T. ) ;
#9889 = CARTESIAN_POINT ( 'NONE',  ( 17.99999999999999645, -71.21168426767047777, -86.70160608319397966 ) ) ;
#9890 = ORIENTED_EDGE ( 'NONE', *, *, #5649, .F. ) ;
#9891 = DIRECTION ( 'NONE',  ( -1.000000000000000000, 0.000000000000000000, 0.000000000000000000 ) ) ;
#9892 = PRODUCT ( 'needle roller bearing_nh_iso_ISO 3245 - 3022D - 20,SI,NC,20', 'needle roller bearing_nh_iso_ISO 3245 - 3022D - 20,SI,NC,20', '', ( #34706 ) ) ;
#9893 = ORIENTED_EDGE ( 'NONE', *, *, #32240, .T. ) ;
#9894 = CARTESIAN_POINT ( 'NONE',  ( -40.35386350238497499, 40.00000000000000000, 69.65762217234959053 ) ) ;
#9896 = DIRECTION ( 'NONE',  ( 0.000000000000000000, 0.000000000000000000, 1.000000000000000000 ) ) ;
#9895 = CARTESIAN_POINT ( 'NONE',  ( 0.000000000000000000, 17.50309955389612426, 43.60271849949370448 ) ) ;
#9897 = DIRECTION ( 'NONE',  ( -1.000000000000000000, 0.000000000000000000, 0.000000000000000000 ) ) ;
#9898 = ORIENTED_EDGE ( 'NONE', *, *, #41893, .T. ) ;
#9899 = CARTESIAN_POINT ( 'NONE',  ( 17.99999999999999645, -25.52601536738605859, 19.21447964122688390 ) ) ;
#9900 = VERTEX_POINT ( 'NONE', #27192 ) ;
#9901 = SURFACE_STYLE_USAGE ( .BOTH. , #12771 ) ;
#9902 = AXIS2_PLACEMENT_3D ( 'NONE', #6098, #19652, #32922 ) ;
#9903 = DIRECTION ( 'NONE',  ( 0.000000000000000000, 0.000000000000000000, -1.000000000000000000 ) ) ;
#9904 = VECTOR ( 'NONE', #43020, 1000.000000000000000 ) ;
#9905 = CARTESIAN_POINT ( 'NONE',  ( -70.15350862410126354, 31.00000000000000711, -40.50401079722123399 ) ) ;
#9907 = CARTESIAN_POINT ( 'NONE',  ( -135.4416936590755540, -12.05525454449572109, -102.7350398871816424 ) ) ;
#9906 = DIRECTION ( 'NONE',  ( 0.000000000000000000, 0.000000000000000000, 1.000000000000000000 ) ) ;
#9908 = ORIENTED_EDGE ( 'NONE', *, *, #33246, .T. ) ;
#9909 = CIRCLE ( 'NONE', #31513, 13.59999999999999964 ) ;
#9910 = CARTESIAN_POINT ( 'NONE',  ( -9.000000000000005329, 14.91999999999999815, 0.000000000000000000 ) ) ;
#9911 = CIRCLE ( 'NONE', #34304, 59.00000000000000000 ) ;
#9912 = ORIENTED_EDGE ( 'NONE', *, *, #27910, .T. ) ;
#9913 = LINE ( 'NONE', #30012, #11736 ) ;
#9914 = CARTESIAN_POINT ( 'NONE',  ( 18.00000000000000355, 46.87740477351718482, -3.172455868805370560 ) ) ;
#9915 = LINE ( 'NONE', #23263, #26853 ) ;
#9916 = EDGE_CURVE ( 'NONE', #27181, #20720, #3792, .T. ) ;
#9917 = CYLINDRICAL_SURFACE ( 'NONE', #34435, 59.00000000000000000 ) ;
#9918 = ADVANCED_FACE ( 'NONE', ( #36766 ), #750, .T. ) ;
#9919 = CYLINDRICAL_SURFACE ( 'NONE', #41503, 158.4999999999992042 ) ;
#9920 = ORIENTED_EDGE ( 'NONE', *, *, #37505, .T. ) ;
#9921 = CYLINDRICAL_SURFACE ( 'NONE', #24968, 47.49900000000000233 ) ;
#9922 = ORIENTED_EDGE ( 'NONE', *, *, #33799, .T. ) ;
#9923 = CARTESIAN_POINT ( 'NONE',  ( 9.000000000000001776, -0.6505223195679212811, -51.99593080916758936 ) ) ;
#9924 = CARTESIAN_POINT ( 'NONE',  ( 0.000000000000000000, 27.83061035787114079, -117.2431154827794586 ) ) ;
#9925 = DIRECTION ( 'NONE',  ( -1.000000000000000000, 0.000000000000000000, -0.000000000000000000 ) ) ;
#9926 = VERTEX_POINT ( 'NONE', #10151 ) ;
#9927 = CARTESIAN_POINT ( 'NONE',  ( 103.7695705685741387, 106.4195705685767166, 6.999999999999998224 ) ) ;
#9928 = CARTESIAN_POINT ( 'NONE',  ( 0.000000000000000000, 74.56001736500617483, 88.86396238369059120 ) ) ;
#9929 = EDGE_CURVE ( 'NONE', #8178, #29573, #32765, .T. ) ;
#9930 = CIRCLE ( 'NONE', #2280, 120.5010000000000474 ) ;
#9931 = DIRECTION ( 'NONE',  ( -1.000000000000000000, -0.000000000000000000, 0.000000000000000000 ) ) ;
#9933 = EDGE_LOOP ( 'NONE', ( #3866, #32045, #8042, #9777 ) ) ;
#9932 = CARTESIAN_POINT ( 'NONE',  ( 11.90854556226686789, -40.05525454449572464, -74.83297477053821467 ) ) ;
#9934 = EDGE_CURVE ( 'NONE', #10316, #4569, #7699, .T. ) ;
#9935 = CARTESIAN_POINT ( 'NONE',  ( -32.09999204393464822, 31.00000000000000355, -2.147948991655045159 ) ) ;
#9936 = DIRECTION ( 'NONE',  ( -1.000000000000000000, 0.000000000000000000, 0.000000000000000000 ) ) ;
#9937 = VECTOR ( 'NONE', #20722, 1000.000000000000000 ) ;
#9939 = EDGE_LOOP ( 'NONE', ( #38032, #32165, #3780 ) ) ;
#9938 = CARTESIAN_POINT ( 'NONE',  ( 17.99999999999999645, 0.000000000000000000, 0.000000000000000000 ) ) ;
#9940 = EDGE_LOOP ( 'NONE', ( #23654, #29326, #5965, #7548 ) ) ;
#9941 = CARTESIAN_POINT ( 'NONE',  ( 0.000000000000000000, 73.78980555658731078, -95.26571049921918188 ) ) ;
#9942 = CARTESIAN_POINT ( 'NONE',  ( 17.99999999999999645, 98.39501399267960835, 53.91376164787712355 ) ) ;
#9944 = CARTESIAN_POINT ( 'NONE',  ( 3.665567271000699012, 40.00000000000000000, -54.59530427606813419 ) ) ;
#9943 = CIRCLE ( 'NONE', #33643, 120.5010000000000190 ) ;
#9945 = CARTESIAN_POINT ( 'NONE',  ( 17.99999999999999645, 0.000000000000000000, 0.000000000000000000 ) ) ;
#9946 = CARTESIAN_POINT ( 'NONE',  ( 0.000000000000000000, 21.48775762007893420, -23.64423737150114135 ) ) ;
#9947 = CYLINDRICAL_SURFACE ( 'NONE', #18611, 20.00000000000000355 ) ;
#9948 = ORIENTED_EDGE ( 'NONE', *, *, #18711, .T. ) ;
#9949 = CARTESIAN_POINT ( 'NONE',  ( 17.99999999999999645, 0.000000000000000000, 0.000000000000000000 ) ) ;
#9950 = VERTEX_POINT ( 'NONE', #33294 ) ;
#9951 = ADVANCED_FACE ( 'NONE', ( #7091 ), #30460, .T. ) ;
#9952 = CARTESIAN_POINT ( 'NONE',  ( 17.99999999999999645, -88.00363688980490906, -82.31555682352745862 ) ) ;
#9953 = PLANE ( 'NONE',  #4562 ) ;
#9955 = EDGE_CURVE ( 'NONE', #4247, #22654, #13987, .T. ) ;
#9954 = CARTESIAN_POINT ( 'NONE',  ( 43.19851606872948935, 31.00000000000000355, 14.66122656362567689 ) ) ;
#9956 = DIRECTION ( 'NONE',  ( 0.000000000000000000, 0.000000000000000000, -1.000000000000000000 ) ) ;
#9957 = ORIENTED_EDGE ( 'NONE', *, *, #34849, .F. ) ;
#9958 = CARTESIAN_POINT ( 'NONE',  ( 18.00000000000000355, 17.08890430202750110, 43.76671000081951490 ) ) ;
#9959 = ORIENTED_EDGE ( 'NONE', *, *, #12072, .T. ) ;
#9960 = AXIS2_PLACEMENT_3D ( 'NONE', #24392, #978, #14558 ) ;
#9961 = CARTESIAN_POINT ( 'NONE',  ( -10.86393331615775892, 40.00000000000000000, -18.79923026442779843 ) ) ;
#9962 = ORIENTED_EDGE ( 'NONE', *, *, #19222, .T. ) ;
#9963 = LINE ( 'NONE', #339, #18579 ) ;
#9964 = EDGE_LOOP ( 'NONE', ( #42989, #22084, #17529, #30149 ) ) ;
#9965 = CARTESIAN_POINT ( 'NONE',  ( -37.00582609755892349, 31.00000000000000355, 48.07482304779467341 ) ) ;
#9966 = CARTESIAN_POINT ( 'NONE',  ( 66.37122006405570573, 39.99999999999999289, -8.639838683448301637 ) ) ;
#9967 = CARTESIAN_POINT ( 'NONE',  ( 8.999999999999998224, 69.72480978690171582, -92.70626138605945243 ) ) ;
#9968 =( GEOMETRIC_REPRESENTATION_CONTEXT ( 3 ) GLOBAL_UNCERTAINTY_ASSIGNED_CONTEXT ( ( #1959 ) ) GLOBAL_UNIT_ASSIGNED_CONTEXT ( ( #24390, #37639, #41117 ) ) REPRESENTATION_CONTEXT ( 'NONE', 'WORKASPACE' ) );
#9969 = ADVANCED_FACE ( 'NONE', ( #20445 ), #1, .T. ) ;
#9970 = VERTEX_POINT ( 'NONE', #40667 ) ;
#9971 = ORIENTED_EDGE ( 'NONE', *, *, #32896, .F. ) ;
#9972 = AXIS2_PLACEMENT_3D ( 'NONE', #13693, #19817, #37003 ) ;
#9973 = CARTESIAN_POINT ( 'NONE',  ( 0.02511973781850649831, -4.877415612947427981, -3.751298745799844792 ) ) ;
#9974 = DIRECTION ( 'NONE',  ( 1.000000000000000000, -0.000000000000000000, -0.000000000000000000 ) ) ;
#9975 = CARTESIAN_POINT ( 'NONE',  ( -132.0000507999999968, 0.000000000000000000, 0.000000000000000000 ) ) ;
#9977 = ORIENTED_EDGE ( 'NONE', *, *, #3207, .F. ) ;
#9976 = DIRECTION ( 'NONE',  ( 0.000000000000000000, 0.2486898871648482723, 0.9685831611286328524 ) ) ;
#9978 = DIRECTION ( 'NONE',  ( 0.000000000000000000, -1.000000000000000000, 5.297542245118643184E-16 ) ) ;
#9979 = VERTEX_POINT ( 'NONE', #542 ) ;
#9980 = FACE_OUTER_BOUND ( 'NONE', #32179, .T. ) ;
#9981 = ADVANCED_FACE ( 'NONE', ( #20668 ), #33935, .T. ) ;
#9982 = CARTESIAN_POINT ( 'NONE',  ( 5.726861599741335240, 40.00000000000000000, 87.39583333411552246 ) ) ;
#9983 = DIRECTION ( 'NONE',  ( -1.000000000000000000, 0.000000000000000000, -0.000000000000000000 ) ) ;
#9984 = EDGE_LOOP ( 'NONE', ( #79, #41965, #11497, #2320 ) ) ;
#9985 = CARTESIAN_POINT ( 'NONE',  ( 18.00000000000000355, -25.61928775981074580, 45.25098998563467489 ) ) ;
#9986 = EDGE_CURVE ( 'NONE', #4386, #11416, #24375, .T. ) ;
#9987 = CARTESIAN_POINT ( 'NONE',  ( 17.99999999999999645, 0.000000000000000000, 0.000000000000000000 ) ) ;
#9988 = AXIS2_PLACEMENT_3D ( 'NONE', #21876, #12243, #18615 ) ;
#9989 = EDGE_CURVE ( 'NONE', #9115, #24259, #39019, .T. ) ;
#9990 = EDGE_LOOP ( 'NONE', ( #16201, #10985, #41390, #31763 ) ) ;
#9991 = AXIS2_PLACEMENT_3D ( 'NONE', #20534, #39898, #40338 ) ;
#9992 = ORIENTED_EDGE ( 'NONE', *, *, #38700, .T. ) ;
#9993 = DIRECTION ( 'NONE',  ( -1.000000000000000000, -0.000000000000000000, 0.000000000000000000 ) ) ;
#9994 = VERTEX_POINT ( 'NONE', #40893 ) ;
#9995 = CARTESIAN_POINT ( 'NONE',  ( 0.000000000000000000, -88.00363688980601751, 82.31555682352626491 ) ) ;
#9996 = DIRECTION ( 'NONE',  ( -1.000000000000000000, -0.000000000000000000, -0.000000000000000000 ) ) ;
#9997 = FACE_OUTER_BOUND ( 'NONE', #29660, .T. ) ;
#9998 = DIRECTION ( 'NONE',  ( 0.000000000000000000, 0.000000000000000000, 1.000000000000000000 ) ) ;
#9999 = DIRECTION ( 'NONE',  ( 0.000000000000000000, 0.8951632913550634507, -0.4457383557765359217 ) ) ;
#10000 = VERTEX_POINT ( 'NONE', #18063 ) ;
#10002 = DIRECTION ( 'NONE',  ( 0.000000000000000000, 0.000000000000000000, 1.000000000000000000 ) ) ;
#10001 = MECHANICAL_DESIGN_GEOMETRIC_PRESENTATION_REPRESENTATION (  '', ( #17715 ), #37156 ) ;
#10003 = ORIENTED_EDGE ( 'NONE', *, *, #7583, .F. ) ;
#10004 = AXIS2_PLACEMENT_3D ( 'NONE', #43062, #39572, #23255 ) ;
#10005 = LINE ( 'NONE', #160, #13422 ) ;
#10007 = EDGE_CURVE ( 'NONE', #21541, #28496, #14314, .T. ) ;
#10006 = DIRECTION ( 'NONE',  ( -1.000000000000000000, -0.000000000000000000, 0.000000000000000000 ) ) ;
#10008 = ORIENTED_EDGE ( 'NONE', *, *, #22208, .F. ) ;
#10009 = CARTESIAN_POINT ( 'NONE',  ( 0.000000000000000000, -3.996885678773838713, 120.4346956066681713 ) ) ;
#10010 = EDGE_CURVE ( 'NONE', #14078, #23500, #38065, .T. ) ;
#10011 = FACE_OUTER_BOUND ( 'NONE', #13234, .T. ) ;
#10012 = CIRCLE ( 'NONE', #34399, 47.49899999999998812 ) ;
#10013 = PRODUCT_CONTEXT ( 'NONE', #18697, 'mechanical' ) ;
#10014 = CARTESIAN_POINT ( 'NONE',  ( -93.98204972788910538, -2.055254544495720648, 39.37702493556011518 ) ) ;
#10015 = CARTESIAN_POINT ( 'NONE',  ( -43.59452257625678584, 31.00000000000000355, -56.81327804312699925 ) ) ;
#10016 = APPLICATION_CONTEXT ( 'automotive_design' ) ;
#10017 = ORIENTED_EDGE ( 'NONE', *, *, #21960, .F. ) ;
#10018 = CARTESIAN_POINT ( 'NONE',  ( -32.09999204393464822, 31.00000000000000355, -2.147948991655045159 ) ) ;
#10019 = AXIS2_PLACEMENT_3D ( 'NONE', #5879, #2371, #32506 ) ;
#10020 = CARTESIAN_POINT ( 'NONE',  ( -61.47519263390311295, 40.00000000000000711, -35.49250405581909007 ) ) ;
#10021 = CIRCLE ( 'NONE', #36481, 36.00000000000000000 ) ;
#10022 = LINE ( 'NONE', #16382, #16600 ) ;
#10023 = ORIENTED_EDGE ( 'NONE', *, *, #21729, .F. ) ;
#10024 = LINE ( 'NONE', #6758, #1647 ) ;
#10025 = CARTESIAN_POINT ( 'NONE',  ( 8.999999999999998224, 97.97378550988226209, 62.10585602713793207 ) ) ;
#10026 = AXIS2_PLACEMENT_3D ( 'NONE', #23843, #37108, #7213 ) ;
#10027 = EDGE_CURVE ( 'NONE', #22504, #26216, #41770, .T. ) ;
#10028 = ORIENTED_EDGE ( 'NONE', *, *, #6856, .T. ) ;
#10029 = CARTESIAN_POINT ( 'NONE',  ( 41.10549127292548377, 40.00000000000000000, 20.25863663968860706 ) ) ;
#10030 = DIRECTION ( 'NONE',  ( 0.000000000000000000, -0.9911528310040056411, -0.1327255272837324085 ) ) ;
#10031 = CIRCLE ( 'NONE', #26104, 116.0000000000000000 ) ;
#10032 = DIRECTION ( 'NONE',  ( 0.000000000000000000, -0.9574220383620081209, 0.2886919473396123981 ) ) ;
#10033 = ORIENTED_EDGE ( 'NONE', *, *, #9535, .T. ) ;
#10034 = EDGE_CURVE ( 'NONE', #18362, #43113, #6974, .T. ) ;
#10035 = CARTESIAN_POINT ( 'NONE',  ( -105.9879088449591933, 31.00000000000000355, -0.3807199291576673361 ) ) ;
#10036 = DIRECTION ( 'NONE',  ( -1.000000000000000000, -0.000000000000000000, -0.000000000000000000 ) ) ;
#10037 = VERTEX_POINT ( 'NONE', #11049 ) ;
#10038 = DIRECTION ( 'NONE',  ( 0.000000000000000000, 0.8993121301712172500, 0.4373073204588593388 ) ) ;
#10039 = VERTEX_POINT ( 'NONE', #14544 ) ;
#10040 = VECTOR ( 'NONE', #35734, 1000.000000000000000 ) ;
#10041 = AXIS2_PLACEMENT_3D ( 'NONE', #3219, #36608, #13520 ) ;
#10042 = ORIENTED_EDGE ( 'NONE', *, *, #33568, .T. ) ;
#10043 = AXIS2_PLACEMENT_3D ( 'NONE', #21736, #38042, #34990 ) ;
#10044 = CARTESIAN_POINT ( 'NONE',  ( 0.000000000000000000, 30.93515269692114344, 36.04401931830261674 ) ) ;
#10045 = CARTESIAN_POINT ( 'NONE',  ( 30.72743980831337751, 31.00000000000000355, -90.12673907452091271 ) ) ;
#10046 = EDGE_LOOP ( 'NONE', ( #17778, #37315, #32923, #20943 ) ) ;
#10047 = FACE_OUTER_BOUND ( 'NONE', #40695, .T. ) ;
#10048 = VECTOR ( 'NONE', #40481, 1000.000000000000000 ) ;
#10049 = CARTESIAN_POINT ( 'NONE',  ( 0.000000000000000000, -30.74337109795213863, -8.695908345466433431 ) ) ;
#10050 = PLANE ( 'NONE',  #31049 ) ;
#10051 = ORIENTED_EDGE ( 'NONE', *, *, #29533, .F. ) ;
#10052 = DIRECTION ( 'NONE',  ( 1.000000000000000000, 0.000000000000000000, 0.000000000000000000 ) ) ;
#10053 = CIRCLE ( 'NONE', #37925, 31.49899999999999878 ) ;
#10054 = DIRECTION ( 'NONE',  ( -1.000000000000000000, 0.000000000000000000, 0.000000000000000000 ) ) ;
#10055 = EDGE_CURVE ( 'NONE', #6806, #40193, #10475, .T. ) ;
#10056 = EDGE_CURVE ( 'NONE', #22786, #24835, #17828, .T. ) ;
#10058 = DIRECTION ( 'NONE',  ( -1.000000000000000000, 0.000000000000000000, -0.000000000000000000 ) ) ;
#10057 = DIRECTION ( 'NONE',  ( -1.000000000000000000, 0.000000000000000000, 0.000000000000000000 ) ) ;
#10059 = EDGE_CURVE ( 'NONE', #10843, #5501, #4909, .T. ) ;
#10060 = ADVANCED_FACE ( 'NONE', ( #18270 ), #18480, .F. ) ;
#10061 = CYLINDRICAL_SURFACE ( 'NONE', #5421, 120.5010000000000190 ) ;
#10062 = CARTESIAN_POINT ( 'NONE',  ( 0.000000000000000000, 0.000000000000000000, 0.000000000000000000 ) ) ;
#10063 = ORIENTED_EDGE ( 'NONE', *, *, #28081, .F. ) ;
#10064 = CIRCLE ( 'NONE', #1717, 59.00000000000000711 ) ;
#10065 = CARTESIAN_POINT ( 'NONE',  ( 10.63353083439206870, 31.00000000000000355, -31.33693976183458219 ) ) ;
#10066 = ORIENTED_EDGE ( 'NONE', *, *, #14932, .T. ) ;
#10067 = DIRECTION ( 'NONE',  ( 1.000000000000000000, 0.000000000000000000, 0.000000000000000000 ) ) ;
#10068 = LINE ( 'NONE', #3502, #12476 ) ;
#10069 = ORIENTED_EDGE ( 'NONE', *, *, #28986, .T. ) ;
#10070 = CARTESIAN_POINT ( 'NONE',  ( 17.99999999999999645, 0.000000000000000000, 0.000000000000000000 ) ) ;
#10071 = CARTESIAN_POINT ( 'NONE',  ( -20.88694679984194380, 40.00000000000000000, -36.15586224631631751 ) ) ;
#10072 = AXIS2_PLACEMENT_3D ( 'NONE', #17012, #37255, #30297 ) ;
#10073 = CARTESIAN_POINT ( 'NONE',  ( -32.45554871466747215, 40.00000000000000000, -28.56710966684967090 ) ) ;
#10074 = EDGE_LOOP ( 'NONE', ( #36005, #10953, #3575, #4072 ) ) ;
#10075 = ORIENTED_EDGE ( 'NONE', *, *, #38940, .T. ) ;
#10076 = DIRECTION ( 'NONE',  ( 0.000000000000000000, 0.000000000000000000, -1.000000000000000000 ) ) ;
#10077 = CYLINDRICAL_SURFACE ( 'NONE', #24202, 59.00000000000000000 ) ;
#10078 = DIRECTION ( 'NONE',  ( 0.000000000000000000, 0.000000000000000000, 1.000000000000000000 ) ) ;
#10079 = CARTESIAN_POINT ( 'NONE',  ( -91.96080130434580724, -40.05525454449572464, 14.45886780445738218 ) ) ;
#10080 = AXIS2_PLACEMENT_3D ( 'NONE', #30663, #1611, #31524 ) ;
#10081 = ORIENTED_EDGE ( 'NONE', *, *, #19989, .F. ) ;
#10082 = DIRECTION ( 'NONE',  ( -3.996523416598930318E-16, 2.658563593772947863E-15, 1.000000000000000000 ) ) ;
#10083 = ORIENTED_EDGE ( 'NONE', *, *, #40753, .T. ) ;
#10084 = CYLINDRICAL_SURFACE ( 'NONE', #15993, 116.0000000000000000 ) ;
#10085 = LINE ( 'NONE', #3307, #1922 ) ;
#10086 = EDGE_LOOP ( 'NONE', ( #26281, #3736, #1474 ) ) ;
#10087 = DIRECTION ( 'NONE',  ( -1.000000000000000000, 0.000000000000000000, -0.000000000000000000 ) ) ;
#10088 = DIRECTION ( 'NONE',  ( 1.000000000000000000, 0.000000000000000000, 0.000000000000000000 ) ) ;
#10089 = VERTEX_POINT ( 'NONE', #21963 ) ;
#10090 = DIRECTION ( 'NONE',  ( -1.000000000000000000, -0.000000000000000000, -0.000000000000000000 ) ) ;
#10091 = ORIENTED_EDGE ( 'NONE', *, *, #15199, .T. ) ;
#10092 = DIRECTION ( 'NONE',  ( 0.000000000000000000, 4.469118107601265561E-15, -1.000000000000000000 ) ) ;
#10093 = VECTOR ( 'NONE', #14941, 1000.000000000000000 ) ;
#10094 = ORIENTED_EDGE ( 'NONE', *, *, #22622, .F. ) ;
#10096 = ORIENTED_EDGE ( 'NONE', *, *, #20552, .F. ) ;
#10095 = DIRECTION ( 'NONE',  ( 0.02040816326530612776, -0.9997917317482359900, 0.000000000000000000 ) ) ;
#10097 = CARTESIAN_POINT ( 'NONE',  ( 64.47787635702036368, 31.00000000000000000, -17.16423577041365789 ) ) ;
#10098 = ORIENTED_EDGE ( 'NONE', *, *, #8917, .F. ) ;
#10099 = DIRECTION ( 'NONE',  ( 1.000000000000000000, -0.000000000000000000, -0.000000000000000000 ) ) ;
#10100 = VECTOR ( 'NONE', #12705, 1000.000000000000000 ) ;
#10101 = ORIENTED_EDGE ( 'NONE', *, *, #3582, .F. ) ;
#10102 = CARTESIAN_POINT ( 'NONE',  ( 0.000000000000000000, 118.8387007424473580, -19.94628303336371644 ) ) ;
#10103 = ORIENTED_EDGE ( 'NONE', *, *, #37302, .T. ) ;
#10104 = CARTESIAN_POINT ( 'NONE',  ( 86.24314314301659579, 39.99999999999999289, -11.24622374122959201 ) ) ;
#10105 = CIRCLE ( 'NONE', #16395, 36.00000000000000000 ) ;
#10107 = CARTESIAN_POINT ( 'NONE',  ( 0.000000000000000000, 0.000000000000000000, 0.000000000000000000 ) ) ;
#10106 = DIRECTION ( 'NONE',  ( 0.02040816326530612776, 0.9997917317482359900, -0.000000000000000000 ) ) ;
#10108 = AXIS2_PLACEMENT_3D ( 'NONE', #9910, #23259, #36512 ) ;
#10109 = ADVANCED_FACE ( 'NONE', ( #41105 ), #15205, .T. ) ;
#10110 = EDGE_CURVE ( 'NONE', #13372, #11747, #17493, .T. ) ;
#10111 = CYLINDRICAL_SURFACE ( 'NONE', #35235, 59.00000000000000000 ) ;
#10112 = VERTEX_POINT ( 'NONE', #37836 ) ;
#10113 = CARTESIAN_POINT ( 'NONE',  ( -15.99999999999997691, 40.00000000000000000, 5.571627607371296764E-15 ) ) ;
#10114 = VERTEX_POINT ( 'NONE', #35220 ) ;
#10115 = EDGE_CURVE ( 'NONE', #13510, #14100, #31535, .T. ) ;
#10116 = AXIS2_PLACEMENT_3D ( 'NONE', #18902, #25651, #18700 ) ;
#10117 = CARTESIAN_POINT ( 'NONE',  ( 9.000000000000001776, -35.11945359308136716, 38.34871548466002622 ) ) ;
#10118 = CARTESIAN_POINT ( 'NONE',  ( 46.64447153568531945, 31.00000000000000355, 60.78881617101084345 ) ) ;
#10120 = CARTESIAN_POINT ( 'NONE',  ( 2.836893136758676270, 3.208949435745843903, -3.505054077164911241 ) ) ;
#10119 = DIRECTION ( 'NONE',  ( -3.009274222672345096E-17, -1.000000000000000000, 2.455023325076454960E-18 ) ) ;
#10121 = ORIENTED_EDGE ( 'NONE', *, *, #6127, .F. ) ;
#10122 = EDGE_CURVE ( 'NONE', #15605, #16577, #21107, .T. ) ;
#10123 = CARTESIAN_POINT ( 'NONE',  ( 0.000000000000000000, -46.87740477351720614, 3.172455868805039270 ) ) ;
#10124 = AXIS2_PLACEMENT_3D ( 'NONE', #32137, #25621, #22777 ) ;
#10125 = EDGE_CURVE ( 'NONE', #6385, #21574, #42505, .T. ) ;
#10126 = ORIENTED_EDGE ( 'NONE', *, *, #4522, .F. ) ;
#10127 = DIRECTION ( 'NONE',  ( 0.000000000000000000, 0.9510565162951521989, 0.3090169943749514481 ) ) ;
#10128 = CARTESIAN_POINT ( 'NONE',  ( 17.99999999999999645, -111.9370513079666409, -44.61600100275288838 ) ) ;
#10129 = AXIS2_PLACEMENT_3D ( 'NONE', #14552, #40904, #27859 ) ;
#10130 = CARTESIAN_POINT ( 'NONE',  ( 0.000000000000000000, -39.64889472655708147, -33.64468972902550803 ) ) ;
#10131 = CIRCLE ( 'NONE', #24797, 0.08000000000000020983 ) ;
#10132 = AXIS2_PLACEMENT_3D ( 'NONE', #41923, #25389, #35390 ) ;
#10133 = AXIS2_PLACEMENT_3D ( 'NONE', #35928, #42902, #42262 ) ;
#10134 = ORIENTED_EDGE ( 'NONE', *, *, #5750, .F. ) ;
#10135 = CARTESIAN_POINT ( 'NONE',  ( 17.99999999999999645, 114.6488492393079781, 37.09625815500054102 ) ) ;
#10136 = EDGE_LOOP ( 'NONE', ( #9838, #18844, #13461, #13864 ) ) ;
#10137 = DIRECTION ( 'NONE',  ( 1.000000000000000000, -1.373900992973641868E-15, -4.049512215214018063E-16 ) ) ;
#10138 = VECTOR ( 'NONE', #18304, 1000.000000000000000 ) ;
#10139 = CIRCLE ( 'NONE', #376, 120.5010000000000190 ) ;
#10140 = DIRECTION ( 'NONE',  ( 1.000000000000000000, 0.000000000000000000, 0.000000000000000000 ) ) ;
#10141 = CARTESIAN_POINT ( 'NONE',  ( 17.99999999999999645, 0.000000000000000000, 0.000000000000000000 ) ) ;
#10142 = ORIENTED_EDGE ( 'NONE', *, *, #5762, .F. ) ;
#10143 = EDGE_CURVE ( 'NONE', #24120, #27034, #21325, .T. ) ;
#10144 = VERTEX_POINT ( 'NONE', #1407 ) ;
#10145 = DIRECTION ( 'NONE',  ( 0.000000000000000000, 0.5264321628773507289, 0.8502171357296173237 ) ) ;
#10146 = LINE ( 'NONE', #36531, #29173 ) ;
#10147 = CARTESIAN_POINT ( 'NONE',  ( 17.99999999999999645, 0.000000000000000000, 0.000000000000000000 ) ) ;
#10149 = ORIENTED_EDGE ( 'NONE', *, *, #31719, .F. ) ;
#10148 = CARTESIAN_POINT ( 'NONE',  ( 103.7695705685734850, 106.4195705685780524, 10.00000000000025402 ) ) ;
#10150 = CARTESIAN_POINT ( 'NONE',  ( -31.89861325429239258, 31.00000000000000355, 2.042328591206914012 ) ) ;
#10151 = CARTESIAN_POINT ( 'NONE',  ( 17.99999999999999645, 5.492704054966705662, 115.8698847939556344 ) ) ;
#10153 = VERTEX_POINT ( 'NONE', #28282 ) ;
#10152 = DIRECTION ( 'NONE',  ( 1.000000000000000000, 0.000000000000000000, 0.000000000000000000 ) ) ;
#10154 = ORIENTED_EDGE ( 'NONE', *, *, #15717, .F. ) ;
#10155 = CARTESIAN_POINT ( 'NONE',  ( 17.99999999999999645, 0.000000000000000000, 0.000000000000000000 ) ) ;
#10156 = CARTESIAN_POINT ( 'NONE',  ( -105.9879088449591933, 40.00000000000000000, -0.3807199291576673361 ) ) ;
#10157 = CARTESIAN_POINT ( 'NONE',  ( -16.19793102918200134, 40.00000000000000000, 47.43702525406639836 ) ) ;
#10158 = DIRECTION ( 'NONE',  ( 0.000000000000000000, -1.000000000000000000, 0.000000000000000000 ) ) ;
#10159 = AXIS2_PLACEMENT_3D ( 'NONE', #29556, #13204, #42827 ) ;
#10160 = LINE ( 'NONE', #7543, #10283 ) ;
#10161 = ADVANCED_FACE ( 'NONE', ( #41552 ), #11697, .F. ) ;
#10162 = CARTESIAN_POINT ( 'NONE',  ( 7.000000000000006217, 7.118024431592600946E-15, 0.000000000000000000 ) ) ;
#10163 = ORIENTED_EDGE ( 'NONE', *, *, #4434, .T. ) ;
#10164 = DIRECTION ( 'NONE',  ( 1.000000000000000000, 0.000000000000000000, 0.000000000000000000 ) ) ;
#10165 = VECTOR ( 'NONE', #26090, 1000.000000000000000 ) ;
#10166 = ORIENTED_EDGE ( 'NONE', *, *, #11346, .F. ) ;
#10167 = PRODUCT_RELATED_PRODUCT_CATEGORY ( 'part', '', ( #113 ) ) ;
#10168 = AXIS2_PLACEMENT_3D ( 'NONE', #7934, #724, #24122 ) ;
#10169 = DIRECTION ( 'NONE',  ( 0.000000000000000000, 0.000000000000000000, -1.000000000000000000 ) ) ;
#10170 = CARTESIAN_POINT ( 'NONE',  ( 0.000000000000000000, 0.000000000000000000, 0.000000000000000000 ) ) ;
#10171 = CARTESIAN_POINT ( 'NONE',  ( 34.77048308403384169, 31.00000000000000355, 30.48958026498159768 ) ) ;
#10172 = CARTESIAN_POINT ( 'NONE',  ( 17.99999999999999645, -40.13512380274045199, 113.6206972269520179 ) ) ;
#10174 = VERTEX_POINT ( 'NONE', #35438 ) ;
#10173 = CIRCLE ( 'NONE', #31817, 116.0000000000000000 ) ;
#10175 = ADVANCED_FACE ( 'NONE', ( #35639 ), #38921, .T. ) ;
#10176 = AXIS2_PLACEMENT_3D ( 'NONE', #17306, #40366, #40147 ) ;
#10177 = EDGE_CURVE ( 'NONE', #14877, #5508, #30024, .T. ) ;
#10179 = AXIS2_PLACEMENT_3D ( 'NONE', #40948, #20941, #25284 ) ;
#10178 = CARTESIAN_POINT ( 'NONE',  ( 17.99999999999999645, 108.8880088604276608, 39.99251838045997687 ) ) ;
#10180 = VERTEX_POINT ( 'NONE', #19114 ) ;
#10181 = CARTESIAN_POINT ( 'NONE',  ( 25.17870271038170316, 31.00000000000000355, 93.97695291299892517 ) ) ;
#10182 = EDGE_CURVE ( 'NONE', #42638, #8139, #14713, .T. ) ;
#10183 = ORIENTED_EDGE ( 'NONE', *, *, #1316, .T. ) ;
#10184 = DIRECTION ( 'NONE',  ( -1.000000000000000000, 0.000000000000000000, -0.000000000000000000 ) ) ;
#10185 = CARTESIAN_POINT ( 'NONE',  ( -61.81085491475939619, 31.00000000000000711, 35.57109242551294415 ) ) ;
#10186 = CARTESIAN_POINT ( 'NONE',  ( -71.72626536479072001, 40.00000000000000711, -9.557116936239163252 ) ) ;
#10187 = FACE_OUTER_BOUND ( 'NONE', #1181, .T. ) ;
#10188 = VERTEX_POINT ( 'NONE', #38704 ) ;
#10189 = ORIENTED_EDGE ( 'NONE', *, *, #1251, .F. ) ;
#10190 = DIRECTION ( 'NONE',  ( 0.000000000000000000, -0.9980267284282708928, -0.06279051952932446223 ) ) ;
#10191 = DIRECTION ( 'NONE',  ( 1.000000000000000000, 1.836909530733573776E-16, 0.000000000000000000 ) ) ;
#10192 = CARTESIAN_POINT ( 'NONE',  ( 17.99999999999999645, 0.000000000000000000, 0.000000000000000000 ) ) ;
#10193 = CIRCLE ( 'NONE', #32500, 120.5010000000000190 ) ;
#10195 = VERTEX_POINT ( 'NONE', #42404 ) ;
#10194 = CYLINDRICAL_SURFACE ( 'NONE', #34615, 116.0000000000000000 ) ;
#10196 = CARTESIAN_POINT ( 'NONE',  ( 9.000000000000001776, 11.65176648921190150, -115.4133282497341355 ) ) ;
#10198 = VERTEX_POINT ( 'NONE', #5557 ) ;
#10197 = CIRCLE ( 'NONE', #29745, 20.00000000000000711 ) ;
#10199 = CARTESIAN_POINT ( 'NONE',  ( 150.0000507999999968, 0.000000000000000000, 0.000000000000000000 ) ) ;
#10200 = EDGE_CURVE ( 'NONE', #42739, #8178, #25865, .T. ) ;
#10201 = CIRCLE ( 'NONE', #40834, 120.5010000000000332 ) ;
#10202 = CARTESIAN_POINT ( 'NONE',  ( 85.10416666585589951, 39.99999999999999289, 5.563236982362346872 ) ) ;
#10203 = CARTESIAN_POINT ( 'NONE',  ( 17.99999999999999645, 79.94368240339426279, 90.16373242487935613 ) ) ;
#10204 = EDGE_CURVE ( 'NONE', #7021, #28925, #39756, .T. ) ;
#10205 = AXIS2_PLACEMENT_3D ( 'NONE', #23006, #36249, #29517 ) ;
#10206 = ORIENTED_EDGE ( 'NONE', *, *, #37688, .F. ) ;
#10207 = CARTESIAN_POINT ( 'NONE',  ( 8.999999999999998224, -97.97378550988183576, -62.10585602713859288 ) ) ;
#10208 = ADVANCED_FACE ( 'NONE', ( #18914 ), #5343, .T. ) ;
#10209 = DIRECTION ( 'NONE',  ( 0.000000000000000000, 0.000000000000000000, -1.000000000000000000 ) ) ;
#10210 = AXIS2_PLACEMENT_3D ( 'NONE', #41142, #21587, #1442 ) ;
#10211 = VERTEX_POINT ( 'NONE', #2463 ) ;
#10212 = AXIS2_PLACEMENT_3D ( 'NONE', #35737, #9145, #28604 ) ;
#10213 = DIRECTION ( 'NONE',  ( 1.000000000000000000, 0.000000000000000000, 0.000000000000000000 ) ) ;
#10214 = ORIENTED_EDGE ( 'NONE', *, *, #9989, .F. ) ;
#10215 = DIRECTION ( 'NONE',  ( -1.000000000000000000, -0.000000000000000000, 0.000000000000000000 ) ) ;
#10216 = VERTEX_POINT ( 'NONE', #39552 ) ;
#10217 = CARTESIAN_POINT ( 'NONE',  ( 8.075107282079295956, 40.00000000000000000, -23.73893940452291318 ) ) ;
#10218 = CARTESIAN_POINT ( 'NONE',  ( 0.000000000000000000, -31.08872492059985504, 41.68322423723089543 ) ) ;
#10219 = DIRECTION ( 'NONE',  ( -1.000000000000000000, -0.000000000000000000, -0.000000000000000000 ) ) ;
#10220 = FACE_OUTER_BOUND ( 'NONE', #42871, .T. ) ;
#10221 = FACE_OUTER_BOUND ( 'NONE', #3411, .T. ) ;
#10222 = ORIENTED_EDGE ( 'NONE', *, *, #19119, .F. ) ;
#10224 = LINE ( 'NONE', #23572, #22757 ) ;
#10223 = DIRECTION ( 'NONE',  ( 0.000000000000000000, 0.05322217484217877520, -0.9985826956767620555 ) ) ;
#10225 = EDGE_CURVE ( 'NONE', #41306, #2648, #23777, .T. ) ;
#10226 = ORIENTED_EDGE ( 'NONE', *, *, #28139, .F. ) ;
#10227 =( NAMED_UNIT ( * ) SI_UNIT ( $, .STERADIAN. ) SOLID_ANGLE_UNIT ( ) );
#10228 = CARTESIAN_POINT ( 'NONE',  ( 17.99999999999999645, 0.000000000000000000, 0.000000000000000000 ) ) ;
#10229 = CARTESIAN_POINT ( 'NONE',  ( 17.99999999999999645, 79.18387647320879807, -84.76976882518680156 ) ) ;
#10231 = VERTEX_POINT ( 'NONE', #2049 ) ;
#10230 = VECTOR ( 'NONE', #7352, 1000.000000000000000 ) ;
#10232 = CARTESIAN_POINT ( 'NONE',  ( 0.000000000000000000, -111.2721026680459602, 44.61974821237267719 ) ) ;
#10233 = DIRECTION ( 'NONE',  ( 0.000000000000000000, 0.000000000000000000, 1.000000000000000000 ) ) ;
#10234 = AXIS2_PLACEMENT_3D ( 'NONE', #30861, #28255, #34336 ) ;
#10235 = ITEM_DEFINED_TRANSFORMATION ( 'NONE', 'NONE', #17047,  #13552 ) ;
#10236 = EDGE_CURVE ( 'NONE', #41169, #31298, #29336, .T. ) ;
#10237 = DIRECTION ( 'NONE',  ( 0.000000000000000000, 0.000000000000000000, -1.000000000000000000 ) ) ;
#10238 = CARTESIAN_POINT ( 'NONE',  ( -4.417864660710832503, 31.00000000000000355, 67.60416666563759236 ) ) ;
#10239 = CIRCLE ( 'NONE', #40279, 0.4000000000000010214 ) ;
#10240 = ORIENTED_EDGE ( 'NONE', *, *, #16310, .T. ) ;
#10242 = CARTESIAN_POINT ( 'NONE',  ( 47.09643503919448193, 31.00000000000000355, 3.164684800459845349 ) ) ;
#10241 = AXIS2_PLACEMENT_3D ( 'NONE', #6870, #30871, #40005 ) ;
#10243 = EDGE_CURVE ( 'NONE', #8823, #29283, #3501, .T. ) ;
#10244 = CARTESIAN_POINT ( 'NONE',  ( 73.00591898829820536, 39.99999999999999289, 19.54754034098114701 ) ) ;
#10245 = VECTOR ( 'NONE', #3131, 1000.000000000000000 ) ;
#10246 =( NAMED_UNIT ( * ) PLANE_ANGLE_UNIT ( ) SI_UNIT ( $, .RADIAN. ) );
#10247 = AXIS2_PLACEMENT_3D ( 'NONE', #28661, #41501, #11218 ) ;
#10248 = FACE_OUTER_BOUND ( 'NONE', #111, .T. ) ;
#10249 = ORIENTED_EDGE ( 'NONE', *, *, #29466, .T. ) ;
#10250 = LINE ( 'NONE', #30766, #39930 ) ;
#10251 = DIRECTION ( 'NONE',  ( 0.000000000000000000, -0.4132121857683668797, -0.9106347728549182285 ) ) ;
#10252 = PRODUCT_DEFINITION_SHAPE ( 'NONE', 'NONE',  #10820 ) ;
#10253 = VERTEX_POINT ( 'NONE', #35841 ) ;
#10254 = CARTESIAN_POINT ( 'NONE',  ( -29.22812062908682051, 40.00000000000000000, 50.62729764625685647 ) ) ;
#10255 = CARTESIAN_POINT ( 'NONE',  ( 17.99999999999999645, 0.000000000000000000, 0.000000000000000000 ) ) ;
#10257 = EDGE_CURVE ( 'NONE', #30765, #26249, #19535, .T. ) ;
#10256 = CYLINDRICAL_SURFACE ( 'NONE', #30543, 19.19999999999999574 ) ;
#10258 = ORIENTED_EDGE ( 'NONE', *, *, #38354, .F. ) ;
#10259 = ADVANCED_FACE ( 'NONE', ( #32804 ), #8826, .T. ) ;
#10260 = CIRCLE ( 'NONE', #23533, 59.00000000000001421 ) ;
#10261 = FACE_OUTER_BOUND ( 'NONE', #31009, .T. ) ;
#10262 = LINE ( 'NONE', #40126, #9609 ) ;
#10263 = ORIENTED_EDGE ( 'NONE', *, *, #11020, .F. ) ;
#10264 = CARTESIAN_POINT ( 'NONE',  ( -139.5000000000000000, 0.000000000000000000, 9.999999999999998224 ) ) ;
#10265 = ORIENTED_EDGE ( 'NONE', *, *, #6525, .F. ) ;
#10266 = CIRCLE ( 'NONE', #12382, 59.00000000000000000 ) ;
#10267 = AXIS2_PLACEMENT_3D ( 'NONE', #3477, #19476, #22538 ) ;
#10268 = VERTEX_POINT ( 'NONE', #15609 ) ;
#10269 = CIRCLE ( 'NONE', #14475, 120.5010000000000190 ) ;
#10270 = CARTESIAN_POINT ( 'NONE',  ( 4.000000000000000000, -2.309401076758516691, -0.4999999999999995559 ) ) ;
#10271 = AXIS2_PLACEMENT_3D ( 'NONE', #31318, #31742, #24801 ) ;
#10272 = CARTESIAN_POINT ( 'NONE',  ( -41.44813913998980581, 31.00000000000000355, -84.33308812960441969 ) ) ;
#10273 = ORIENTED_EDGE ( 'NONE', *, *, #20169, .T. ) ;
#10274 = CARTESIAN_POINT ( 'NONE',  ( 17.99999999999999645, 0.000000000000000000, 0.000000000000000000 ) ) ;
#10275 = EDGE_CURVE ( 'NONE', #267, #32870, #34893, .T. ) ;
#10276 = AXIS2_PLACEMENT_3D ( 'NONE', #15594, #2237, #26264 ) ;
#10277 = LINE ( 'NONE', #39919, #36560 ) ;
#10278 = DIRECTION ( 'NONE',  ( -1.000000000000000000, 0.000000000000000000, 0.000000000000000000 ) ) ;
#10279 = VERTEX_POINT ( 'NONE', #42177 ) ;
#10280 = CYLINDRICAL_SURFACE ( 'NONE', #42621, 116.0000000000000000 ) ;
#10281 = EDGE_CURVE ( 'NONE', #1786, #40777, #31423, .T. ) ;
#10282 = EDGE_CURVE ( 'NONE', #25436, #34149, #25661, .T. ) ;
#10283 = VECTOR ( 'NONE', #6889, 1000.000000000000000 ) ;
#10284 = DIRECTION ( 'NONE',  ( -1.000000000000000000, -0.000000000000000000, -0.000000000000000000 ) ) ;
#10286 = CARTESIAN_POINT ( 'NONE',  ( 0.000000000000000000, 0.000000000000000000, 0.000000000000000000 ) ) ;
#10285 = CYLINDRICAL_SURFACE ( 'NONE', #36345, 36.00000000000000000 ) ;
#10287 = DIRECTION ( 'NONE',  ( 0.000000000000000000, 0.000000000000000000, 1.000000000000000000 ) ) ;
#10288 = VERTEX_POINT ( 'NONE', #42816 ) ;
#10289 = CARTESIAN_POINT ( 'NONE',  ( 0.000000000000000000, 0.000000000000000000, 0.000000000000000000 ) ) ;
#10290 = EDGE_CURVE ( 'NONE', #13830, #22307, #36967, .T. ) ;
#10291 = CARTESIAN_POINT ( 'NONE',  ( -39.95047694894377344, 31.00000000000000355, -5.256506769647570465 ) ) ;
#10292 = EDGE_LOOP ( 'NONE', ( #8973, #18638, #10557, #12955 ) ) ;
#10293 = CARTESIAN_POINT ( 'NONE',  ( 17.99999999999999645, 42.87700105098607395, 107.7847984684006377 ) ) ;
#10294 = EDGE_CURVE ( 'NONE', #20690, #31728, #25861, .T. ) ;
#10295 = DIRECTION ( 'NONE',  ( 0.000000000000000000, 0.000000000000000000, 1.000000000000000000 ) ) ;
#10296 = CIRCLE ( 'NONE', #1913, 116.0000000000000000 ) ;
#10297 = VERTEX_POINT ( 'NONE', #36931 ) ;
#10298 = DIRECTION ( 'NONE',  ( -1.000000000000000000, 0.000000000000000000, -0.000000000000000000 ) ) ;
#10299 = CARTESIAN_POINT ( 'NONE',  ( -40.58740609958903889, 40.00000000000000000, -31.12922691583434798 ) ) ;
#10300 = CIRCLE ( 'NONE', #2609, 36.00000000000000000 ) ;
#10301 = CARTESIAN_POINT ( 'NONE',  ( -14.09736097164574709, 40.00000000000000000, -41.75563764761122343 ) ) ;
#10302 = CIRCLE ( 'NONE', #11700, 59.00000000000001421 ) ;
#10303 = AXIS2_PLACEMENT_3D ( 'NONE', #35599, #32758, #28665 ) ;
#10304 = AXIS2_PLACEMENT_3D ( 'NONE', #4438, #30868, #37610 ) ;
#10305 = VERTEX_POINT ( 'NONE', #7042 ) ;
#10306 = CYLINDRICAL_SURFACE ( 'NONE', #29071, 120.5010000000000190 ) ;
#10307 = DIRECTION ( 'NONE',  ( 0.000000000000000000, 0.000000000000000000, 1.000000000000000000 ) ) ;
#10308 = DIRECTION ( 'NONE',  ( 0.000000000000000000, 0.000000000000000000, 1.000000000000000000 ) ) ;
#10309 = ORIENTED_EDGE ( 'NONE', *, *, #41149, .T. ) ;
#10310 = CARTESIAN_POINT ( 'NONE',  ( 20.70971545910534672, 40.00000000000000000, 15.87948211774388518 ) ) ;
#10311 = VERTEX_POINT ( 'NONE', #13845 ) ;
#10312 = CARTESIAN_POINT ( 'NONE',  ( 17.99999999999999645, -110.3490479609633752, 20.28201389785361641 ) ) ;
#10313 = CARTESIAN_POINT ( 'NONE',  ( 22.90854556226710415, -14.05525454449572997, -74.83297477053821467 ) ) ;
#10314 = AXIS2_PLACEMENT_3D ( 'NONE', #14323, #7311, #33944 ) ;
#10315 = EDGE_CURVE ( 'NONE', #9453, #17146, #16807, .T. ) ;
#10316 = VERTEX_POINT ( 'NONE', #23449 ) ;
#10317 = EDGE_CURVE ( 'NONE', #34636, #21461, #24508, .T. ) ;
#10318 = CARTESIAN_POINT ( 'NONE',  ( 0.000000000000000000, 35.89808275599445153, 2.706964063997353342 ) ) ;
#10319 = EDGE_CURVE ( 'NONE', #39631, #13079, #38374, .T. ) ;
#10320 = EDGE_CURVE ( 'NONE', #7063, #33075, #19973, .T. ) ;
#10321 = DIRECTION ( 'NONE',  ( 1.000000000000000000, 0.000000000000000000, 0.000000000000000000 ) ) ;
#10322 = VERTEX_POINT ( 'NONE', #13197 ) ;
#10323 = CARTESIAN_POINT ( 'NONE',  ( 17.99999999999999645, 0.000000000000000000, 0.000000000000000000 ) ) ;
#10324 = VERTEX_POINT ( 'NONE', #26702 ) ;
#10325 = DIRECTION ( 'NONE',  ( 0.000000000000000000, 0.000000000000000000, -1.000000000000000000 ) ) ;
#10326 = ORIENTED_EDGE ( 'NONE', *, *, #11338, .T. ) ;
#10328 = ORIENTED_EDGE ( 'NONE', *, *, #15054, .F. ) ;
#10327 = DIRECTION ( 'NONE',  ( -1.000000000000000000, 0.000000000000000000, 0.000000000000000000 ) ) ;
#10329 = CARTESIAN_POINT ( 'NONE',  ( -41.78821403078461572, 31.00000000000000355, -47.79414628086201589 ) ) ;
#10330 = ORIENTED_EDGE ( 'NONE', *, *, #27210, .F. ) ;
#10331 = CARTESIAN_POINT ( 'NONE',  ( 17.99999999999999645, -69.72480978690109055, 92.70626138605992139 ) ) ;
#10332 = VECTOR ( 'NONE', #15759, 1000.000000000000000 ) ;
#10333 = AXIS2_PLACEMENT_3D ( 'NONE', #16390, #29696, #42967 ) ;
#10334 = CIRCLE ( 'NONE', #24297, 116.0000000000000000 ) ;
#10335 = EDGE_LOOP ( 'NONE', ( #13319, #41304, #16722, #8147 ) ) ;
#10336 = AXIS2_PLACEMENT_3D ( 'NONE', #14133, #4718, #17858 ) ;
#10337 = CARTESIAN_POINT ( 'NONE',  ( 17.99999999999999645, -52.19040376560500505, 99.31985817764160629 ) ) ;
#10338 = ORIENTED_EDGE ( 'NONE', *, *, #38340, .T. ) ;
#10339 = CARTESIAN_POINT ( 'NONE',  ( 58.29702017945731995, 39.99999999999999289, 66.63806913872475945 ) ) ;
#10340 = AXIS2_PLACEMENT_3D ( 'NONE', #12749, #6824, #20181 ) ;
#10341 = AXIS2_PLACEMENT_3D ( 'NONE', #18754, #37520, #38527 ) ;
#10343 = DIRECTION ( 'NONE',  ( -1.000000000000000000, -0.000000000000000000, 0.000000000000000000 ) ) ;
#10342 = DIRECTION ( 'NONE',  ( -1.000000000000000000, 0.000000000000000000, 0.000000000000000000 ) ) ;
#10344 = CARTESIAN_POINT ( 'NONE',  ( 9.000000000000001776, 19.74581912682842599, 48.10512059033399623 ) ) ;
#10345 = EDGE_LOOP ( 'NONE', ( #13545, #6734, #9245, #3905 ) ) ;
#10346 = CARTESIAN_POINT ( 'NONE',  ( 0.000000000000000000, 118.8387007424470738, 19.94628303336527608 ) ) ;
#10347 = ORIENTED_EDGE ( 'NONE', *, *, #33012, .T. ) ;
#10348 = EDGE_CURVE ( 'NONE', #33962, #15592, #27146, .T. ) ;
#10349 = CARTESIAN_POINT ( 'NONE',  ( 17.99999999999999645, -31.80866420683989304, -2.997093558041628025 ) ) ;
#10350 = CYLINDRICAL_SURFACE ( 'NONE', #9375, 20.00000000000000711 ) ;
#10351 = CARTESIAN_POINT ( 'NONE',  ( 6.054110834496887250, 31.00000000000000355, -92.60416666599778068 ) ) ;
#10352 = EDGE_CURVE ( 'NONE', #16718, #18043, #19602, .T. ) ;
#10353 = DIRECTION ( 'NONE',  ( 0.000000000000000000, -0.7865515558026479059, 0.6175246149461850464 ) ) ;
#10354 = VERTEX_POINT ( 'NONE', #16699 ) ;
#10355 = EDGE_CURVE ( 'NONE', #13399, #31470, #12613, .T. ) ;
#10356 = DIRECTION ( 'NONE',  ( -1.000000000000000000, 0.000000000000000000, 0.000000000000000000 ) ) ;
#10357 = ORIENTED_EDGE ( 'NONE', *, *, #41900, .F. ) ;
#10358 = FACE_OUTER_BOUND ( 'NONE', #25618, .T. ) ;
#10359 = DIRECTION ( 'NONE',  ( 0.000000000000000000, 0.000000000000000000, 1.000000000000000000 ) ) ;
#10360 = DIRECTION ( 'NONE',  ( 1.058513553088275437E-16, 1.000000000000000000, -8.813324511995299047E-17 ) ) ;
#10361 = VECTOR ( 'NONE', #32263, 1000.000000000000000 ) ;
#10362 = CARTESIAN_POINT ( 'NONE',  ( 0.000000000000000000, -100.6739960869714139, -49.52796165323368172 ) ) ;
#10363 = AXIS2_PLACEMENT_3D ( 'NONE', #21947, #32362, #2235 ) ;
#10364 = VERTEX_POINT ( 'NONE', #10544 ) ;
#10365 = DIRECTION ( 'NONE',  ( 0.000000000000000000, 0.000000000000000000, 1.000000000000000000 ) ) ;
#10366 = ORIENTED_EDGE ( 'NONE', *, *, #2305, .F. ) ;
#10367 = CARTESIAN_POINT ( 'NONE',  ( 17.99999999999999645, 40.13512380273970592, 113.6206972269522737 ) ) ;
#10368 = FACE_OUTER_BOUND ( 'NONE', #30738, .T. ) ;
#10369 = EDGE_CURVE ( 'NONE', #40182, #3503, #39759, .T. ) ;
#10370 = ADVANCED_FACE ( 'NONE', ( #27353 ), #33009, .T. ) ;
#10371 = DIRECTION ( 'NONE',  ( -1.000000000000000000, 0.000000000000000000, -0.000000000000000000 ) ) ;
#10372 = VERTEX_POINT ( 'NONE', #3536 ) ;
#10373 = ORIENTED_EDGE ( 'NONE', *, *, #37739, .T. ) ;
#10374 = CARTESIAN_POINT ( 'NONE',  ( 9.000000000000001776, -31.17727234463771424, 111.7317219465818852 ) ) ;
#10375 = CYLINDRICAL_SURFACE ( 'NONE', #17297, 59.00000000000000000 ) ;
#10376 = ADVANCED_FACE ( 'NONE', ( #36279 ), #30630, .F. ) ;
#10377 = CARTESIAN_POINT ( 'NONE',  ( 4.203935335434060505, 1.640780671294165272, -3.598452447879202598 ) ) ;
#10379 = ORIENTED_EDGE ( 'NONE', *, *, #38446, .F. ) ;
#10378 = CARTESIAN_POINT ( 'NONE',  ( 0.000000000000000000, 47.22458491092819344, 5.098390039074386593 ) ) ;
#10380 = CARTESIAN_POINT ( 'NONE',  ( 4.597210615069569961, 31.00000000000000355, -34.47704375836577384 ) ) ;
#10381 = CARTESIAN_POINT ( 'NONE',  ( -106.4195705685749402, 106.4195705685765745, 7.000000000000337508 ) ) ;
#10383 = ORIENTED_EDGE ( 'NONE', *, *, #29504, .T. ) ;
#10382 = CARTESIAN_POINT ( 'NONE',  ( 9.000000000000001776, 115.0622509503834578, -14.72000021165029082 ) ) ;
#10384 = UNCERTAINTY_MEASURE_WITH_UNIT (LENGTH_MEASURE( 1.000000000000000082E-05 ), #23770, 'distance_accuracy_value', 'NONE');
#10385 = ORIENTED_EDGE ( 'NONE', *, *, #19445, .T. ) ;
#10386 = CARTESIAN_POINT ( 'NONE',  ( 17.99999999999999645, 0.000000000000000000, 0.000000000000000000 ) ) ;
#10387 = CARTESIAN_POINT ( 'NONE',  ( 22.99999999999988987, -9.790568863845134872E-14, -26.00000000000001421 ) ) ;
#10388 = CARTESIAN_POINT ( 'NONE',  ( 50.14038141241296387, 40.00000000000000000, 29.06424286984033145 ) ) ;
#10389 = ADVANCED_FACE ( 'NONE', ( #13406 ), #40194, .F. ) ;
#10390 = AXIS2_PLACEMENT_3D ( 'NONE', #30235, #30457, #30033 ) ;
#10391 = CIRCLE ( 'NONE', #8989, 18.77999999999999048 ) ;
#10392 = DIRECTION ( 'NONE',  ( 0.9247238835424299586, 4.035472873002398249E-16, 0.3806385939525924744 ) ) ;
#10393 = PRODUCT_DEFINITION_CONTEXT ( 'detailed design', #22886, 'design' ) ;
#10394 = CARTESIAN_POINT ( 'NONE',  ( 8.999999999999998224, -64.69195966009955612, 96.28577441832231898 ) ) ;
#10395 = EDGE_LOOP ( 'NONE', ( #7185, #40809, #2645, #31258, #12083, #28003, #9260, #27534, #20029, #33412, #39773, #30040, #21251, #19062, #16185, #7279 ) ) ;
#10396 = CIRCLE ( 'NONE', #13907, 51.99999999999999289 ) ;
#10397 = CARTESIAN_POINT ( 'NONE',  ( 0.000000000000000000, 19.74581912682909035, -48.10512059033372623 ) ) ;
#10398 = ORIENTED_EDGE ( 'NONE', *, *, #11544, .T. ) ;
#10399 = LINE ( 'NONE', #23732, #21861 ) ;
#10400 = CARTESIAN_POINT ( 'NONE',  ( 8.999999999999998224, 64.69195966010022403, -96.28577441832183581 ) ) ;
#10401 = CARTESIAN_POINT ( 'NONE',  ( -16.10381281257427943, 31.00000000000000355, -60.09637020943575436 ) ) ;
#10402 = DIRECTION ( 'NONE',  ( 1.000000000000000000, 0.000000000000000000, 0.000000000000000000 ) ) ;
#10403 = VERTEX_POINT ( 'NONE', #10331 ) ;
#10404 = DIRECTION ( 'NONE',  ( 0.000000000000000000, -0.5076658003388468954, 0.8615540813938020737 ) ) ;
#10405 = ORIENTED_EDGE ( 'NONE', *, *, #16296, .T. ) ;
#10406 = CARTESIAN_POINT ( 'NONE',  ( 94.89583333399441756, 31.00000000000000000, -6.217735451874103703 ) ) ;
#10407 = ORIENTED_EDGE ( 'NONE', *, *, #29480, .T. ) ;
#10408 = CYLINDRICAL_SURFACE ( 'NONE', #12415, 116.0000000000000000 ) ;
#10409 = DIRECTION ( 'NONE',  ( 0.000000000000000000, 0.000000000000000000, -1.000000000000000000 ) ) ;
#10410 = CARTESIAN_POINT ( 'NONE',  ( -35.65230965298280097, 31.00000000000000355, 72.05959145978816593 ) ) ;
#10411 = CARTESIAN_POINT ( 'NONE',  ( -82.09281090897877675, 40.00000000000000711, -5.486092462564050365 ) ) ;
#10412 = DIRECTION ( 'NONE',  ( -3.996523416598930318E-16, 2.658563593772947863E-15, 1.000000000000000000 ) ) ;
#10413 = EDGE_LOOP ( 'NONE', ( #17719, #42045, #32251, #8341 ) ) ;
#10414 = DIRECTION ( 'NONE',  ( -1.000000000000000000, -0.000000000000000000, -0.000000000000000000 ) ) ;
#10415 = VERTEX_POINT ( 'NONE', #23239 ) ;
#10416 = CIRCLE ( 'NONE', #12614, 10.49999999999998934 ) ;
#10417 = CYLINDRICAL_SURFACE ( 'NONE', #22803, 47.49900000000000233 ) ;
#10418 = EDGE_CURVE ( 'NONE', #29283, #16283, #36275, .T. ) ;
#10419 = DIRECTION ( 'NONE',  ( -1.000000000000000000, -0.000000000000000000, -0.000000000000000000 ) ) ;
#10420 = AXIS2_PLACEMENT_3D ( 'NONE', #16036, #25859, #19110 ) ;
#10421 = CIRCLE ( 'NONE', #24382, 52.00000000000000000 ) ;
#10423 = VERTEX_POINT ( 'NONE', #23673 ) ;
#10422 = CARTESIAN_POINT ( 'NONE',  ( 8.999999999999998224, -95.31344542257777164, 66.11616384574416827 ) ) ;
#10424 = EDGE_CURVE ( 'NONE', #3149, #22707, #13220, .T. ) ;
#10425 = CARTESIAN_POINT ( 'NONE',  ( 18.00000000000000355, 0.000000000000000000, 0.000000000000000000 ) ) ;
#10426 = ORIENTED_EDGE ( 'NONE', *, *, #39262, .F. ) ;
#10427 = CARTESIAN_POINT ( 'NONE',  ( 2.345747346278113987, -3.264484291692503870, -0.01223254789874484924 ) ) ;
#10428 = VECTOR ( 'NONE', #34241, 1000.000000000000000 ) ;
#10429 = CARTESIAN_POINT ( 'NONE',  ( 84.24376206367318787, 39.99999999999999289, -11.10575268747775901 ) ) ;
#10430 = CARTESIAN_POINT ( 'NONE',  ( -1.317756351988340180, 3.857995168970202116, -0.04852650426601388955 ) ) ;
#10431 = ORIENTED_EDGE ( 'NONE', *, *, #30528, .F. ) ;
#10432 = LINE ( 'NONE', #36819, #33853 ) ;
#10433 = CARTESIAN_POINT ( 'NONE',  ( 0.000000000000000000, 0.000000000000000000, 0.000000000000000000 ) ) ;
#10434 = SHAPE_REPRESENTATION ( 'Planetary Gear Carrier Assembly', ( #13552 ), #21242 ) ;
#10435 = ORIENTED_EDGE ( 'NONE', *, *, #5045, .T. ) ;
#10436 = EDGE_CURVE ( 'NONE', #24676, #4662, #17526, .T. ) ;
#10437 = DIRECTION ( 'NONE',  ( -1.000000000000000000, 0.000000000000000000, -0.000000000000000000 ) ) ;
#10438 = ORIENTED_EDGE ( 'NONE', *, *, #3584, .F. ) ;
#10439 = FACE_OUTER_BOUND ( 'NONE', #18848, .T. ) ;
#10440 = ORIENTED_EDGE ( 'NONE', *, *, #9929, .T. ) ;
#10441 = CARTESIAN_POINT ( 'NONE',  ( -102.9608013043458072, -40.05525454449572464, 14.45886780445738218 ) ) ;
#10442 = DIRECTION ( 'NONE',  ( -1.000000000000000000, 0.000000000000000000, -0.000000000000000000 ) ) ;
#10443 = DIRECTION ( 'NONE',  ( -1.000000000000000000, -0.000000000000000000, 0.000000000000000000 ) ) ;
#10444 = EDGE_CURVE ( 'NONE', #1566, #10322, #24326, .T. ) ;
#10445 = CARTESIAN_POINT ( 'NONE',  ( 0.000000000000000000, 117.6086855750634470, 26.24286718912143712 ) ) ;
#10446 = DIRECTION ( 'NONE',  ( 0.000000000000000000, 0.5963673585384970943, 0.8027116379309668925 ) ) ;
#10447 = ORIENTED_EDGE ( 'NONE', *, *, #38715, .F. ) ;
#10449 = DIRECTION ( 'NONE',  ( 0.000000000000000000, 0.2486898871648482723, 0.9685831611286327414 ) ) ;
#10448 = DIRECTION ( 'NONE',  ( 0.000000000000000000, 0.000000000000000000, -1.000000000000000000 ) ) ;
#10450 = ORIENTED_EDGE ( 'NONE', *, *, #23626, .T. ) ;
#10451 = CIRCLE ( 'NONE', #24411, 120.5010000000000190 ) ;
#10452 = FACE_OUTER_BOUND ( 'NONE', #37609, .T. ) ;
#10454 = DIRECTION ( 'NONE',  ( -1.000000000000000000, -0.000000000000000000, 0.000000000000000000 ) ) ;
#10453 = AXIS2_PLACEMENT_3D ( 'NONE', #21052, #24978, #31043 ) ;
#10455 = ORIENTED_EDGE ( 'NONE', *, *, #12238, .T. ) ;
#10456 = DIRECTION ( 'NONE',  ( 0.000000000000000000, 0.000000000000000000, 1.000000000000000000 ) ) ;
#10457 = DIRECTION ( 'NONE',  ( -1.000000000000000000, 0.000000000000000000, 0.000000000000000000 ) ) ;
#10458 = ITEM_DEFINED_TRANSFORMATION ( 'NONE', 'NONE', #10026,  #13552 ) ;
#10459 = FACE_OUTER_BOUND ( 'NONE', #31264, .T. ) ;
#10460 = CARTESIAN_POINT ( 'NONE',  ( 4.745113895470035814, 31.00000000000000355, -72.60416666572081112 ) ) ;
#10461 = EDGE_CURVE ( 'NONE', #37611, #30532, #11417, .T. ) ;
#10462 = ORIENTED_EDGE ( 'NONE', *, *, #32955, .F. ) ;
#10463 = CARTESIAN_POINT ( 'NONE',  ( -20.27214883179046367, 31.00000000000000355, 34.96734655410254788 ) ) ;
#10464 = CARTESIAN_POINT ( 'NONE',  ( -40.93297376624923345, 40.00000000000000000, -70.86912620794510076 ) ) ;
#10465 = CARTESIAN_POINT ( 'NONE',  ( 0.000000000000000000, 0.000000000000000000, 0.000000000000000000 ) ) ;
#10466 = DIRECTION ( 'NONE',  ( 3.996523416598930318E-16, -2.658563593772947863E-15, -1.000000000000000000 ) ) ;
#10467 = ORIENTED_EDGE ( 'NONE', *, *, #42316, .F. ) ;
#10468 = FACE_OUTER_BOUND ( 'NONE', #8934, .T. ) ;
#10469 = CARTESIAN_POINT ( 'NONE',  ( 17.99999999999999645, 80.74349901498510462, -77.90224541347200216 ) ) ;
#10470 = EDGE_CURVE ( 'NONE', #10990, #35040, #4229, .T. ) ;
#10471 = ORIENTED_EDGE ( 'NONE', *, *, #33011, .T. ) ;
#10472 = CARTESIAN_POINT ( 'NONE',  ( -57.67632858778466698, 40.00000000000000711, 15.45560639130400205 ) ) ;
#10473 = CARTESIAN_POINT ( 'NONE',  ( 6.896599878636567205, -12.98179148322719101, 0.000000000000000000 ) ) ;
#10474 = DIRECTION ( 'NONE',  ( 0.000000000000000000, 0.000000000000000000, -1.000000000000000000 ) ) ;
#10475 = CIRCLE ( 'NONE', #11909, 116.0000000000000000 ) ;
#10476 = VERTEX_POINT ( 'NONE', #27798 ) ;
#10477 = AXIS2_PLACEMENT_3D ( 'NONE', #21865, #35535, #22288 ) ;
#10478 = DIRECTION ( 'NONE',  ( -1.000000000000000000, 0.000000000000000000, 0.000000000000000000 ) ) ;
#10479 = CARTESIAN_POINT ( 'NONE',  ( 18.00000000000000355, 44.61570720899074161, 14.73072383765644133 ) ) ;
#10480 = CIRCLE ( 'NONE', #14683, 59.00000000000000711 ) ;
#10481 = ORIENTED_EDGE ( 'NONE', *, *, #3957, .F. ) ;
#10482 = DIRECTION ( 'NONE',  ( 0.000000000000000000, 0.000000000000000000, 1.000000000000000000 ) ) ;
#10483 = ORIENTED_EDGE ( 'NONE', *, *, #3005, .F. ) ;
#10484 = EDGE_CURVE ( 'NONE', #24756, #39386, #11640, .T. ) ;
#10485 = CYLINDRICAL_SURFACE ( 'NONE', #21248, 59.00000000000000000 ) ;
#10486 = ORIENTED_EDGE ( 'NONE', *, *, #32018, .F. ) ;
#10487 = CARTESIAN_POINT ( 'NONE',  ( 18.00000000000000355, 0.000000000000000000, 0.000000000000000000 ) ) ;
#10488 = DIRECTION ( 'NONE',  ( -1.000000000000000000, 0.000000000000000000, 0.000000000000000000 ) ) ;
#10489 = EDGE_CURVE ( 'NONE', #32708, #41990, #27568, .T. ) ;
#10490 = ORIENTED_EDGE ( 'NONE', *, *, #31955, .T. ) ;
#10491 = DIRECTION ( 'NONE',  ( 0.000000000000000000, 0.000000000000000000, 1.000000000000000000 ) ) ;
#10492 = CARTESIAN_POINT ( 'NONE',  ( -2.797566391619251075E-15, 1.860994515641065082E-14, 7.000000000000002665 ) ) ;
#10493 = ADVANCED_FACE ( 'NONE', ( #41489 ), #31486, .F. ) ;
#10494 = LINE ( 'NONE', #23831, #39395 ) ;
#10495 = VERTEX_POINT ( 'NONE', #37582 ) ;
#10496 = FACE_OUTER_BOUND ( 'NONE', #39299, .T. ) ;
#10497 = DIRECTION ( 'NONE',  ( -1.000000000000000000, 0.000000000000000000, 0.000000000000000000 ) ) ;
#10499 = FACE_OUTER_BOUND ( 'NONE', #15318, .T. ) ;
#10498 = DIRECTION ( 'NONE',  ( 0.000000000000000000, 0.000000000000000000, 1.000000000000000000 ) ) ;
#10500 = CIRCLE ( 'NONE', #32094, 13.59999999999999787 ) ;
#10501 = LINE ( 'NONE', #6561, #18716 ) ;
#10502 = ORIENTED_EDGE ( 'NONE', *, *, #10484, .F. ) ;
#10503 = DIRECTION ( 'NONE',  ( 1.000000000000000000, 0.000000000000000000, -3.491481338843133355E-15 ) ) ;
#10504 = CARTESIAN_POINT ( 'NONE',  ( 0.000000000000000000, -51.85248208264514602, -3.914090171286729980 ) ) ;
#10505 = CARTESIAN_POINT ( 'NONE',  ( 34.94781834021004840, 31.00000000000000355, -26.81980329959834108 ) ) ;
#10507 = EDGE_CURVE ( 'NONE', #26054, #25656, #35, .T. ) ;
#10506 = CIRCLE ( 'NONE', #34892, 20.00000000000000355 ) ;
#10508 = ORIENTED_EDGE ( 'NONE', *, *, #22354, .F. ) ;
#10509 = DIRECTION ( 'NONE',  ( 0.000000000000000000, -0.7164567402983209599, 0.6976315211349787271 ) ) ;
#10511 = ADVANCED_FACE ( 'NONE', ( #14489 ), #21058, .F. ) ;
#10510 = AXIS2_PLACEMENT_3D ( 'NONE', #25918, #12398, #4970 ) ;
#10512 = DIRECTION ( 'NONE',  ( -1.000000000000000000, 0.000000000000000000, 0.000000000000000000 ) ) ;
#10513 = VERTEX_POINT ( 'NONE', #41717 ) ;
#10514 = VECTOR ( 'NONE', #32474, 1000.000000000000000 ) ;
#10515 = CARTESIAN_POINT ( 'NONE',  ( 17.99999999999999645, -119.8996782608629275, -12.02323392193477325 ) ) ;
#10516 = CARTESIAN_POINT ( 'NONE',  ( -49.88601606984090608, 40.00000000000000000, -6.565487524765669214 ) ) ;
#10517 = CARTESIAN_POINT ( 'NONE',  ( 5.928665350384931365, 40.00000000000000000, -44.40877992885556580 ) ) ;
#10518 = VECTOR ( 'NONE', #4525, 1000.000000000000000 ) ;
#10519 = ORIENTED_EDGE ( 'NONE', *, *, #9450, .F. ) ;
#10520 = CARTESIAN_POINT ( 'NONE',  ( 8.999999999999998224, 73.51007459736429439, 89.73443560133387109 ) ) ;
#10521 = CARTESIAN_POINT ( 'NONE',  ( 0.000000000000000000, -45.89132998248120288, 102.3829004574628385 ) ) ;
#10522 = CARTESIAN_POINT ( 'NONE',  ( 17.99999999999999645, -119.7318547011702634, 13.59315897125686412 ) ) ;
#10523 = ORIENTED_EDGE ( 'NONE', *, *, #13430, .F. ) ;
#10524 = CARTESIAN_POINT ( 'NONE',  ( -21.73352778766994575, 40.00000000000000000, 19.07242603999910457 ) ) ;
#10525 = ORIENTED_EDGE ( 'NONE', *, *, #34261, .F. ) ;
#10526 = FACE_OUTER_BOUND ( 'NONE', #31267, .T. ) ;
#10527 = DIRECTION ( 'NONE',  ( 0.000000000000000000, 0.9213119778704114138, 0.3888241754733244848 ) ) ;
#10528 = ORIENTED_EDGE ( 'NONE', *, *, #27929, .T. ) ;
#10529 = DIRECTION ( 'NONE',  ( 0.000000000000000000, 0.2113826236296247607, -0.9774033898178666746 ) ) ;
#10530 = CARTESIAN_POINT ( 'NONE',  ( 17.99999999999999645, 0.000000000000000000, 0.000000000000000000 ) ) ;
#10531 = EDGE_LOOP ( 'NONE', ( #15016, #13644, #8871, #14646 ) ) ;
#10532 = DIRECTION ( 'NONE',  ( -1.000000000000000000, 0.000000000000000000, 0.000000000000000000 ) ) ;
#10533 = VERTEX_POINT ( 'NONE', #34100 ) ;
#10534 = CARTESIAN_POINT ( 'NONE',  ( 8.999999999999998224, -104.0201923570372173, -51.34003878071168003 ) ) ;
#10535 = EDGE_CURVE ( 'NONE', #19546, #4953, #33485, .T. ) ;
#10536 = AXIS2_PLACEMENT_3D ( 'NONE', #35845, #2886, #19329 ) ;
#10537 = ORIENTED_EDGE ( 'NONE', *, *, #5889, .F. ) ;
#10539 = ORIENTED_EDGE ( 'NONE', *, *, #2944, .T. ) ;
#10538 = CARTESIAN_POINT ( 'NONE',  ( 0.000000000000000000, 0.000000000000000000, 0.000000000000000000 ) ) ;
#10540 = AXIS2_PLACEMENT_3D ( 'NONE', #4403, #7482, #4631 ) ;
#10541 = CARTESIAN_POINT ( 'NONE',  ( -62.09442273006147417, 31.00000000000000711, -4.163950221635984938 ) ) ;
#10542 = EDGE_CURVE ( 'NONE', #1655, #28779, #22389, .T. ) ;
#10543 = VERTEX_POINT ( 'NONE', #38228 ) ;
#10544 = CARTESIAN_POINT ( 'NONE',  ( 17.99999999999999645, 119.0898412705474385, 18.38751498043773935 ) ) ;
#10545 = AXIS2_PLACEMENT_3D ( 'NONE', #36320, #293, #30030 ) ;
#10546 = ADVANCED_FACE ( 'NONE', ( #31046 ), #31690, .T. ) ;
#10547 = ORIENTED_EDGE ( 'NONE', *, *, #5940, .T. ) ;
#10548 = CYLINDRICAL_SURFACE ( 'NONE', #14080, 1.999999999999998668 ) ;
#10549 = ORIENTED_EDGE ( 'NONE', *, *, #16727, .T. ) ;
#10550 = CARTESIAN_POINT ( 'NONE',  ( -21.69137426901471954, 40.00000000000000000, -81.42030341110599068 ) ) ;
#10551 = VECTOR ( 'NONE', #35339, 1000.000000000000000 ) ;
#10553 = DIRECTION ( 'NONE',  ( 1.000000000000000000, 0.000000000000000000, 0.000000000000000000 ) ) ;
#10552 = DIRECTION ( 'NONE',  ( 0.000000000000000000, -0.5877852522924801315, 0.8090169943749422332 ) ) ;
#10554 = CARTESIAN_POINT ( 'NONE',  ( 158.5000000000000284, 0.000000000000000000, 6.999999999999998224 ) ) ;
#10555 = ORIENTED_EDGE ( 'NONE', *, *, #19658, .T. ) ;
#10556 = CARTESIAN_POINT ( 'NONE',  ( 0.000000000000000000, -98.39501399267994941, 53.91376164787647696 ) ) ;
#10557 = ORIENTED_EDGE ( 'NONE', *, *, #33010, .F. ) ;
#10558 = FILL_AREA_STYLE_COLOUR ( '', #23278 ) ;
#10559 = AXIS2_PLACEMENT_3D ( 'NONE', #11385, #24717, #16176 ) ;
#10560 = SURFACE_STYLE_USAGE ( .BOTH. , #7268 ) ;
#10561 = CARTESIAN_POINT ( 'NONE',  ( 17.99999999999999645, 35.78425302087544679, -3.935382540232420734 ) ) ;
#10562 = EDGE_CURVE ( 'NONE', #31846, #37721, #34231, .T. ) ;
#10563 = CARTESIAN_POINT ( 'NONE',  ( -23.88228986782336349, 31.00000000000000355, -89.13686966975919290 ) ) ;
#10564 = ADVANCED_FACE ( 'NONE', ( #31271 ), #36281, .F. ) ;
#10565 = CARTESIAN_POINT ( 'NONE',  ( -0.02511973781850462134, 4.877415612947412882, -3.751298745799839462 ) ) ;
#10566 = ORIENTED_EDGE ( 'NONE', *, *, #27280, .T. ) ;
#10567 = EDGE_CURVE ( 'NONE', #37692, #31975, #4971, .T. ) ;
#10568 = EDGE_CURVE ( 'NONE', #38781, #38690, #42122, .T. ) ;
#10569 = PLANE ( 'NONE',  #28952 ) ;
#10570 = CIRCLE ( 'NONE', #24532, 20.00000000000000711 ) ;
#10571 = CIRCLE ( 'NONE', #1495, 19.99999999999989342 ) ;
#10572 = EDGE_LOOP ( 'NONE', ( #20458, #14340 ) ) ;
#10573 = FILL_AREA_STYLE_COLOUR ( '', #34562 ) ;
#10574 = DIRECTION ( 'NONE',  ( 1.000000000000000000, 0.000000000000000000, 0.000000000000000000 ) ) ;
#10575 = AXIS2_PLACEMENT_3D ( 'NONE', #24139, #21318, #17818 ) ;
#10576 = CARTESIAN_POINT ( 'NONE',  ( 17.99999999999999645, 0.000000000000000000, 0.000000000000000000 ) ) ;
#10577 = EDGE_LOOP ( 'NONE', ( #25844, #16959 ) ) ;
#10578 = DIRECTION ( 'NONE',  ( 0.000000000000000000, 0.000000000000000000, 1.000000000000000000 ) ) ;
#10579 = ORIENTED_EDGE ( 'NONE', *, *, #12384, .F. ) ;
#10580 = CIRCLE ( 'NONE', #16144, 58.99999999999999289 ) ;
#10581 = DIRECTION ( 'NONE',  ( -1.000000000000000000, 0.000000000000000000, 0.000000000000000000 ) ) ;
#10582 = DIRECTION ( 'NONE',  ( 0.000000000000000000, 0.000000000000000000, 1.000000000000000000 ) ) ;
#10583 = CARTESIAN_POINT ( 'NONE',  ( -25.39999999999999147, 0.000000000000000000, 15.00000000000000000 ) ) ;
#10584 = ORIENTED_EDGE ( 'NONE', *, *, #11991, .T. ) ;
#10585 = ORIENTED_EDGE ( 'NONE', *, *, #41649, .F. ) ;
#10586 = CARTESIAN_POINT ( 'NONE',  ( 17.99999999999999645, 0.000000000000000000, 0.000000000000000000 ) ) ;
#10587 = CARTESIAN_POINT ( 'NONE',  ( 8.999999999999998224, -54.09091620264651823, -102.6166301549523467 ) ) ;
#10588 = EDGE_CURVE ( 'NONE', #36784, #9269, #30759, .T. ) ;
#10589 = LINE ( 'NONE', #4450, #14624 ) ;
#10591 = ORIENTED_EDGE ( 'NONE', *, *, #3727, .T. ) ;
#10590 = DIRECTION ( 'NONE',  ( 0.000000000000000000, 0.000000000000000000, 1.000000000000000000 ) ) ;
#10592 = CARTESIAN_POINT ( 'NONE',  ( -27.06829236441750552, 31.00000000000000355, 15.58100167312263018 ) ) ;
#10593 = EDGE_CURVE ( 'NONE', #28966, #17321, #39077, .T. ) ;
#10594 = CARTESIAN_POINT ( 'NONE',  ( 0.000000000000000000, 32.32520163883631170, -34.09746168776002406 ) ) ;
#10596 = ORIENTED_EDGE ( 'NONE', *, *, #7578, .T. ) ;
#10595 = DIRECTION ( 'NONE',  ( 0.000000000000000000, -3.810511228586342406E-14, -1.000000000000000000 ) ) ;
#10597 = ORIENTED_EDGE ( 'NONE', *, *, #26095, .T. ) ;
#10598 = AXIS2_PLACEMENT_3D ( 'NONE', #29243, #16365, #16154 ) ;
#10599 = CYLINDRICAL_SURFACE ( 'NONE', #24593, 2.649999999999971934 ) ;
#10600 = CARTESIAN_POINT ( 'NONE',  ( 35.58199112951898968, 40.00000000000000000, 46.53705319855855294 ) ) ;
#10601 = CIRCLE ( 'NONE', #830, 116.0000000000000000 ) ;
#10602 = CARTESIAN_POINT ( 'NONE',  ( -101.1532682021072134, 31.00000000000000355, -3.256983028635321187 ) ) ;
#10603 = AXIS2_PLACEMENT_3D ( 'NONE', #26385, #13296, #33115 ) ;
#10604 = LINE ( 'NONE', #10394, #17848 ) ;
#10605 = VERTEX_POINT ( 'NONE', #21911 ) ;
#10606 = CARTESIAN_POINT ( 'NONE',  ( 18.00000000000000355, 13.85708833600031475, -45.43276465116650087 ) ) ;
#10607 = EDGE_LOOP ( 'NONE', ( #12120, #32903, #35241, #30848 ) ) ;
#10608 = CIRCLE ( 'NONE', #39147, 120.5010000000000332 ) ;
#10609 = CARTESIAN_POINT ( 'NONE',  ( 0.000000000000000000, 0.000000000000000000, -1.199999999999999956 ) ) ;
#10610 = LINE ( 'NONE', #3603, #3860 ) ;
#10611 = EDGE_CURVE ( 'NONE', #11646, #42007, #29365, .T. ) ;
#10612 = CARTESIAN_POINT ( 'NONE',  ( 47.00375723443311671, 31.00000000000000355, -27.15133022689256137 ) ) ;
#10613 = ADVANCED_FACE ( 'NONE', ( #29284 ), #19060, .T. ) ;
#10614 = CYLINDRICAL_SURFACE ( 'NONE', #17690, 116.0000000000000000 ) ;
#10615 = ORIENTED_EDGE ( 'NONE', *, *, #16067, .F. ) ;
#10616 = EDGE_CURVE ( 'NONE', #12490, #384, #35163, .T. ) ;
#10617 = EDGE_CURVE ( 'NONE', #41650, #14228, #36304, .T. ) ;
#10618 = PRODUCT_DEFINITION_SHAPE ( 'NONE', 'NONE',  #43192 ) ;
#10619 = EDGE_CURVE ( 'NONE', #4705, #42617, #6352, .T. ) ;
#10620 = DIRECTION ( 'NONE',  ( 0.000000000000000000, 0.000000000000000000, 1.000000000000000000 ) ) ;
#10621 = ORIENTED_EDGE ( 'NONE', *, *, #37838, .T. ) ;
#10622 = CARTESIAN_POINT ( 'NONE',  ( 63.67823170517923614, 31.00000000000000000, 72.58713758494482704 ) ) ;
#10623 = ORIENTED_EDGE ( 'NONE', *, *, #16228, .F. ) ;
#10624 = FACE_OUTER_BOUND ( 'NONE', #27357, .T. ) ;
#10625 = CARTESIAN_POINT ( 'NONE',  ( 18.00000000000000355, 0.000000000000000000, 0.000000000000000000 ) ) ;
#10626 = CARTESIAN_POINT ( 'NONE',  ( -64.10496366466531981, 31.00000000000000711, 31.48763712508877077 ) ) ;
#10627 = CARTESIAN_POINT ( 'NONE',  ( -48.39074809477736494, 40.00000000000000000, -55.33250407649475733 ) ) ;
#10628 = EDGE_CURVE ( 'NONE', #25554, #27794, #16866, .T. ) ;
#10629 = CYLINDRICAL_SURFACE ( 'NONE', #19541, 51.99999999999999289 ) ;
#10630 = CIRCLE ( 'NONE', #35014, 59.00000000000000711 ) ;
#10631 = ORIENTED_EDGE ( 'NONE', *, *, #13641, .T. ) ;
#10632 = CARTESIAN_POINT ( 'NONE',  ( 17.99999999999999645, 0.000000000000000000, 0.000000000000000000 ) ) ;
#10633 = ORIENTED_EDGE ( 'NONE', *, *, #31645, .T. ) ;
#10634 = FILL_AREA_STYLE_COLOUR ( '', #8847 ) ;
#10635 = CIRCLE ( 'NONE', #7130, 120.5010000000000190 ) ;
#10636 = CYLINDRICAL_SURFACE ( 'NONE', #15045, 47.49900000000000233 ) ;
#10637 = CIRCLE ( 'NONE', #8541, 116.0000000000000000 ) ;
#10639 = ORIENTED_EDGE ( 'NONE', *, *, #9490, .F. ) ;
#10638 = CARTESIAN_POINT ( 'NONE',  ( 17.99999999999999645, -21.55123232222391394, -118.5581519187674360 ) ) ;
#10640 = DIRECTION ( 'NONE',  ( 0.000000000000000000, 0.000000000000000000, 1.000000000000000000 ) ) ;
#10641 = VERTEX_POINT ( 'NONE', #41921 ) ;
#10642 = DIRECTION ( 'NONE',  ( 0.000000000000000000, 0.000000000000000000, 1.000000000000000000 ) ) ;
#10643 = CARTESIAN_POINT ( 'NONE',  ( 81.15556025174309696, 39.99999999999999289, 27.54985289775053658 ) ) ;
#10644 = CARTESIAN_POINT ( 'NONE',  ( 17.99999999999999645, -31.48608500567869584, -0.9019157472707834966 ) ) ;
#10645 = VERTEX_POINT ( 'NONE', #25607 ) ;
#10646 = DIRECTION ( 'NONE',  ( 0.000000000000000000, 0.9714298932647090767, 0.2373266998711184850 ) ) ;
#10647 = DIRECTION ( 'NONE',  ( 0.000000000000000000, 0.000000000000000000, 1.000000000000000000 ) ) ;
#10648 = VERTEX_POINT ( 'NONE', #25387 ) ;
#10649 = CARTESIAN_POINT ( 'NONE',  ( 17.99999999999999645, 97.97378550988308632, -62.10585602713662468 ) ) ;
#10650 = ORIENTED_EDGE ( 'NONE', *, *, #11889, .F. ) ;
#10651 = DIRECTION ( 'NONE',  ( 1.000000000000000000, 0.000000000000000000, 0.000000000000000000 ) ) ;
#10652 = EDGE_LOOP ( 'NONE', ( #37736, #1145, #21815, #20558 ) ) ;
#10653 = CARTESIAN_POINT ( 'NONE',  ( -14.30682334061562422, 40.00000000000000000, -18.65445469299709202 ) ) ;
#10654 = FACE_OUTER_BOUND ( 'NONE', #27435, .T. ) ;
#10655 = CARTESIAN_POINT ( 'NONE',  ( 0.000000000000000000, 0.000000000000000000, 0.000000000000000000 ) ) ;
#10656 = DIRECTION ( 'NONE',  ( -1.000000000000000000, 0.000000000000000000, 0.000000000000000000 ) ) ;
#10657 = ORIENTED_EDGE ( 'NONE', *, *, #6026, .F. ) ;
#10659 = CARTESIAN_POINT ( 'NONE',  ( 18.00000000000000355, -8.053585752061598768, -46.81126742072031988 ) ) ;
#10658 = LINE ( 'NONE', #17249, #4238 ) ;
#10660 = ORIENTED_EDGE ( 'NONE', *, *, #2376, .T. ) ;
#10661 = AXIS2_PLACEMENT_3D ( 'NONE', #23521, #6460, #36998 ) ;
#10662 = CARTESIAN_POINT ( 'NONE',  ( 0.000000000000000000, -111.2721026680459602, -14.38025178762732104 ) ) ;
#10663 = CARTESIAN_POINT ( 'NONE',  ( -29.44516979616424024, 31.00000000000000355, -7.879824757621473275 ) ) ;
#10664 = ORIENTED_EDGE ( 'NONE', *, *, #986, .T. ) ;
#10665 = DIRECTION ( 'NONE',  ( -1.000000000000000000, 1.058513553088275437E-16, 0.000000000000000000 ) ) ;
#10666 = EDGE_CURVE ( 'NONE', #13305, #976, #15987, .T. ) ;
#10667 = EDGE_CURVE ( 'NONE', #21659, #40725, #15468, .T. ) ;
#10668 = DIRECTION ( 'NONE',  ( -1.000000000000000000, -0.000000000000000000, 0.000000000000000000 ) ) ;
#10670 = STYLED_ITEM ( 'NONE', ( #19761 ), #38478 ) ;
#10669 = CONTEXT_DEPENDENT_SHAPE_REPRESENTATION ( #16755, #22822 ) ;
#10671 = EDGE_CURVE ( 'NONE', #22892, #20369, #7763, .T. ) ;
#10672 = DIRECTION ( 'NONE',  ( -3.996523416598930318E-16, 2.658563593772947863E-15, 1.000000000000000000 ) ) ;
#10673 = CARTESIAN_POINT ( 'NONE',  ( 9.510694223897102617, 31.00000000000000355, -72.24097909213479340 ) ) ;
#10674 = AXIS2_PLACEMENT_3D ( 'NONE', #21830, #25104, #38352 ) ;
#10675 = ORIENTED_EDGE ( 'NONE', *, *, #27297, .T. ) ;
#10676 = CARTESIAN_POINT ( 'NONE',  ( -16.19793102917653371, 31.00000000000000355, 47.43702525407732651 ) ) ;
#10677 = CARTESIAN_POINT ( 'NONE',  ( 73.03870520561201829, 39.99999999999999289, -42.18585045165268355 ) ) ;
#10678 = EDGE_CURVE ( 'NONE', #12487, #12248, #8767, .T. ) ;
#10679 = CARTESIAN_POINT ( 'NONE',  ( 18.00000000000000355, -13.56094713063606427, 50.20060470671735686 ) ) ;
#10680 = EDGE_CURVE ( 'NONE', #5519, #37013, #42562, .T. ) ;
#10681 = LINE ( 'NONE', #27719, #8905 ) ;
#10682 = DIRECTION ( 'NONE',  ( 1.000000000000000000, 0.000000000000000000, -0.000000000000000000 ) ) ;
#10683 = VECTOR ( 'NONE', #658, 1000.000000000000000 ) ;
#10684 = ORIENTED_EDGE ( 'NONE', *, *, #27058, .F. ) ;
#10685 = CARTESIAN_POINT ( 'NONE',  ( 17.99999999999999645, -115.9750404417044223, 2.406240749597103434 ) ) ;
#10686 = DIRECTION ( 'NONE',  ( -1.000000000000000000, -0.000000000000000000, -0.000000000000000000 ) ) ;
#10687 = AXIS2_PLACEMENT_3D ( 'NONE', #2607, #32101, #2180 ) ;
#10688 = VERTEX_POINT ( 'NONE', #25186 ) ;
#10689 = CARTESIAN_POINT ( 'NONE',  ( 3.436116956419347002, 40.00000000000000000, -52.60416666537189911 ) ) ;
#10690 = DIRECTION ( 'NONE',  ( 1.000000000000000000, 0.000000000000000000, 0.000000000000000000 ) ) ;
#10691 = CARTESIAN_POINT ( 'NONE',  ( 3.999999999999999112, 1.941961291383486277, -0.3515519931180248192 ) ) ;
#10692 = VERTEX_POINT ( 'NONE', #38433 ) ;
#10693 = DIRECTION ( 'NONE',  ( 0.000000000000000000, 0.000000000000000000, 1.000000000000000000 ) ) ;
#10694 = CARTESIAN_POINT ( 'NONE',  ( 17.99999999999999645, -51.27532863109435368, 99.79535634195110561 ) ) ;
#10695 = ORIENTED_EDGE ( 'NONE', *, *, #15509, .F. ) ;
#10696 = CARTESIAN_POINT ( 'NONE',  ( 153.1500000000000057, 1.576403824487674918E-12, 10.00000000000000000 ) ) ;
#10697 = ORIENTED_EDGE ( 'NONE', *, *, #6214, .F. ) ;
#10698 = PRESENTATION_LAYER_ASSIGNMENT (  '', '', ( #6505 ) ) ;
#10699 = DIRECTION ( 'NONE',  ( -0.000000000000000000, -0.000000000000000000, -1.000000000000000000 ) ) ;
#10700 = PRESENTATION_LAYER_ASSIGNMENT (  '', '', ( #40632 ) ) ;
#10701 = EDGE_LOOP ( 'NONE', ( #29596, #4855, #147, #20283 ) ) ;
#10702 = CARTESIAN_POINT ( 'NONE',  ( 9.000000000000001776, 58.30069736313667050, 100.2847380560568951 ) ) ;
#10703 = FACE_OUTER_BOUND ( 'NONE', #3354, .T. ) ;
#10704 = ORIENTED_EDGE ( 'NONE', *, *, #11733, .F. ) ;
#10705 = CARTESIAN_POINT ( 'NONE',  ( 8.999999999999998224, -12.42760411676013810, -33.78690065568439138 ) ) ;
#10706 = FACE_OUTER_BOUND ( 'NONE', #37632, .T. ) ;
#10707 = VERTEX_POINT ( 'NONE', #5502 ) ;
#10708 = DIRECTION ( 'NONE',  ( 0.000000000000000000, -0.9996456111234522934, -0.02662052143778456323 ) ) ;
#10709 = DIRECTION ( 'NONE',  ( -1.000000000000000000, -0.000000000000000000, -0.000000000000000000 ) ) ;
#10710 = CIRCLE ( 'NONE', #21909, 31.49899999999999878 ) ;
#10711 = DIRECTION ( 'NONE',  ( -1.000000000000000000, -0.000000000000000000, -0.000000000000000000 ) ) ;
#10712 = AXIS2_PLACEMENT_3D ( 'NONE', #32716, #36622, #9600 ) ;
#10713 = ADVANCED_FACE ( 'NONE', ( #32119 ), #2200, .T. ) ;
#10714 = CARTESIAN_POINT ( 'NONE',  ( 0.000000000000000000, -84.77518783075045405, -73.49448960231443095 ) ) ;
#10715 = ADVANCED_FACE ( 'NONE', ( #10047 ), #42985, .F. ) ;
#10716 = VERTEX_POINT ( 'NONE', #6987 ) ;
#10717 = DIRECTION ( 'NONE',  ( 1.276222519706427582E-16, -1.000000000000000000, 5.451477089573672491E-17 ) ) ;
#10719 = CIRCLE ( 'NONE', #17704, 116.0000000000000000 ) ;
#10718 = DIRECTION ( 'NONE',  ( 0.000000000000000000, 0.000000000000000000, 1.000000000000000000 ) ) ;
#10720 = CARTESIAN_POINT ( 'NONE',  ( 33.03432996520027132, 31.00000000000000355, -28.98482729919588863 ) ) ;
#10721 = ORIENTED_EDGE ( 'NONE', *, *, #24562, .F. ) ;
#10722 = DIRECTION ( 'NONE',  ( 0.000000000000000000, 1.000000000000000000, -1.060184893785364939E-15 ) ) ;
#10723 = DIRECTION ( 'NONE',  ( -1.000000000000000000, 0.000000000000000000, 0.000000000000000000 ) ) ;
#10724 = ORIENTED_EDGE ( 'NONE', *, *, #7014, .F. ) ;
#10725 = CARTESIAN_POINT ( 'NONE',  ( 6.004904395537136175, -19.19999999999999574, 2.351321854362918473E-15 ) ) ;
#10726 = CARTESIAN_POINT ( 'NONE',  ( -31.39472673864601049, 40.00000000000000000, -40.91112553188754930 ) ) ;
#10727 = AXIS2_PLACEMENT_3D ( 'NONE', #20570, #30367, #4149 ) ;
#10728 = CARTESIAN_POINT ( 'NONE',  ( -61.89998375879795844, 40.00000000000000711, 3.952486745199417673 ) ) ;
#10729 = ADVANCED_FACE ( 'NONE', ( #13143 ), #20344, .T. ) ;
#10730 = AXIS2_PLACEMENT_3D ( 'NONE', #2268, #38504, #42195 ) ;
#10731 = ORIENTED_EDGE ( 'NONE', *, *, #41784, .T. ) ;
#10732 = CARTESIAN_POINT ( 'NONE',  ( 0.000000000000000000, 0.000000000000000000, 0.000000000000000000 ) ) ;
#10733 = EDGE_CURVE ( 'NONE', #1445, #21287, #23621, .T. ) ;
#10734 = DIRECTION ( 'NONE',  ( 0.000000000000000000, 0.000000000000000000, 1.000000000000000000 ) ) ;
#10735 = EDGE_CURVE ( 'NONE', #42150, #26382, #21163, .T. ) ;
#10736 = CARTESIAN_POINT ( 'NONE',  ( 17.99999999999999645, -21.56073507908662634, 23.57770962728557151 ) ) ;
#10737 = AXIS2_PLACEMENT_3D ( 'NONE', #27905, #4081, #7368 ) ;
#10738 = CARTESIAN_POINT ( 'NONE',  ( 17.99999999999999645, -63.24564713401724703, -102.5693868539701299 ) ) ;
#10739 = VERTEX_POINT ( 'NONE', #19692 ) ;
#10740 = CARTESIAN_POINT ( 'NONE',  ( 3.579113344806025054, 40.00000000000000000, 27.11441211503905535 ) ) ;
#10741 = VERTEX_POINT ( 'NONE', #26220 ) ;
#10742 = LINE ( 'NONE', #37345, #27830 ) ;
#10743 = CARTESIAN_POINT ( 'NONE',  ( 17.99999999999999645, 0.000000000000000000, 0.000000000000000000 ) ) ;
#10744 = CIRCLE ( 'NONE', #14248, 51.99999999999999289 ) ;
#10745 = ORIENTED_EDGE ( 'NONE', *, *, #21530, .F. ) ;
#10746 = CARTESIAN_POINT ( 'NONE',  ( 17.99999999999999645, 31.11570115861502828, -4.898994019976315784 ) ) ;
#10747 = VECTOR ( 'NONE', #35506, 1000.000000000000000 ) ;
#10748 = DIRECTION ( 'NONE',  ( 0.000000000000000000, 0.000000000000000000, 1.000000000000000000 ) ) ;
#10749 = ORIENTED_EDGE ( 'NONE', *, *, #30974, .F. ) ;
#10750 = CARTESIAN_POINT ( 'NONE',  ( 0.000000000000000000, -6.486220790509180212, 112.0098273076987283 ) ) ;
#10751 = ORIENTED_EDGE ( 'NONE', *, *, #34361, .T. ) ;
#10752 = CARTESIAN_POINT ( 'NONE',  ( -106.4195705685749402, 106.4195705685765745, 10.00000000000033751 ) ) ;
#10753 = ADVANCED_FACE ( 'NONE', ( #23187 ), #21745, .F. ) ;
#10754 = AXIS2_PLACEMENT_3D ( 'NONE', #32897, #25537, #12846 ) ;
#10755 = ADVANCED_FACE ( 'NONE', ( #6548 ), #13794, .T. ) ;
#10756 = EDGE_LOOP ( 'NONE', ( #16511, #16642 ) ) ;
#10758 = VERTEX_POINT ( 'NONE', #20140 ) ;
#10757 = FACE_BOUND ( 'NONE', #29880, .T. ) ;
#10759 = CARTESIAN_POINT ( 'NONE',  ( 57.21690105881322097, 31.00000000000000000, -50.04162206024282966 ) ) ;
#10761 = EDGE_CURVE ( 'NONE', #12470, #2577, #39496, .T. ) ;
#10760 = ORIENTED_EDGE ( 'NONE', *, *, #36221, .F. ) ;
#10762 = DIRECTION ( 'NONE',  ( 0.000000000000000000, 0.000000000000000000, 1.000000000000000000 ) ) ;
#10763 = CARTESIAN_POINT ( 'NONE',  ( 0.000000000000000000, 1.347111479062088405E-15, 11.00000000000000000 ) ) ;
#10764 = ORIENTED_EDGE ( 'NONE', *, *, #8445, .F. ) ;
#10766 = TOROIDAL_SURFACE ( 'NONE', #16348, 15.08402000000000065, 0.08402000000000148239 ) ;
#10765 = DIRECTION ( 'NONE',  ( 0.000000000000000000, 0.000000000000000000, 1.000000000000000000 ) ) ;
#10767 = ORIENTED_EDGE ( 'NONE', *, *, #37473, .T. ) ;
#10769 = CARTESIAN_POINT ( 'NONE',  ( -87.75478321342750121, 40.00000000000000711, -29.92102470460831753 ) ) ;
#10768 = CIRCLE ( 'NONE', #21956, 15.99999999999998579 ) ;
#10771 = FACE_OUTER_BOUND ( 'NONE', #39222, .T. ) ;
#10770 = CARTESIAN_POINT ( 'NONE',  ( 17.99999999999999645, -16.77727049691128869, 27.19001440037539297 ) ) ;
#10772 = CLOSED_SHELL ( 'NONE', ( #16756, #37070, #10753, #19122, #13608, #14632, #42849, #23887, #22527, #36414, #28197, #32775, #14167, #15893, #35306, #37849, #495, #37388, #2127, #23340, #29798, #19848, #2555, #21060, #42130, #16147, #24486 ) ) ;
#10773 = FACE_OUTER_BOUND ( 'NONE', #22096, .T. ) ;
#10774 = CARTESIAN_POINT ( 'NONE',  ( -6.199999999999997513, 4.693303851024319376E-15, 0.000000000000000000 ) ) ;
#10775 = ADVANCED_FACE ( 'NONE', ( #13568 ), #3689, .F. ) ;
#10776 = ORIENTED_EDGE ( 'NONE', *, *, #2610, .T. ) ;
#10777 = FILL_AREA_STYLE ('',( #28025 ) ) ;
#10778 = AXIS2_PLACEMENT_3D ( 'NONE', #39022, #28169, #3438 ) ;
#10779 = DIRECTION ( 'NONE',  ( -1.000000000000000000, 0.000000000000000000, 0.000000000000000000 ) ) ;
#10780 = CIRCLE ( 'NONE', #36533, 52.00000000000000000 ) ;
#10781 = DIRECTION ( 'NONE',  ( -1.000000000000000000, 0.000000000000000000, 0.000000000000000000 ) ) ;
#10782 = CARTESIAN_POINT ( 'NONE',  ( 55.27058341129635721, 31.00000000000000000, -63.02248852588876105 ) ) ;
#10783 = CARTESIAN_POINT ( 'NONE',  ( 0.5449313310647804220, 4.304185902836899835, -3.316620875263383894 ) ) ;
#10784 = ORIENTED_EDGE ( 'NONE', *, *, #15966, .T. ) ;
#10785 = CIRCLE ( 'NONE', #8655, 59.00000000000000711 ) ;
#10786 = CARTESIAN_POINT ( 'NONE',  ( -103.7695705685756167, 106.4195705685752529, 10.00000000000000000 ) ) ;
#10787 = EDGE_CURVE ( 'NONE', #35201, #14512, #27273, .T. ) ;
#10788 = VECTOR ( 'NONE', #34837, 1000.000000000000000 ) ;
#10789 = ORIENTED_EDGE ( 'NONE', *, *, #20169, .F. ) ;
#10790 = EDGE_LOOP ( 'NONE', ( #23825, #2672, #12521, #14057 ) ) ;
#10791 = CARTESIAN_POINT ( 'NONE',  ( 17.99999999999999645, 97.19627249181192497, -71.22763238166385236 ) ) ;
#10792 = EDGE_CURVE ( 'NONE', #2814, #37962, #16647, .T. ) ;
#10793 = CARTESIAN_POINT ( 'NONE',  ( 17.99999999999999645, 111.2721026680460596, -14.38025178762657852 ) ) ;
#10794 = DIRECTION ( 'NONE',  ( 1.000000000000000000, 0.000000000000000000, 0.000000000000000000 ) ) ;
#10795 = ADVANCED_FACE ( 'NONE', ( #13356 ), #9632, .F. ) ;
#10796 = CYLINDRICAL_SURFACE ( 'NONE', #32349, 59.00000000000000000 ) ;
#10797 = B_SPLINE_CURVE_WITH_KNOTS ( 'NONE', 3,
 ( #22276, #16338, #29644, #42696 ),
 .UNSPECIFIED., .F., .F.,
 ( 4, 4 ),
 ( 0.000000000000000000, 0.002452478801916361129 ),
 .UNSPECIFIED. ) ;
#10798 = ORIENTED_EDGE ( 'NONE', *, *, #10348, .F. ) ;
#10799 = CARTESIAN_POINT ( 'NONE',  ( -81.46080130434573618, -35.35525454449571470, 14.45886780445633946 ) ) ;
#10800 = ORIENTED_EDGE ( 'NONE', *, *, #35787, .F. ) ;
#10801 = CARTESIAN_POINT ( 'NONE',  ( 17.99999999999999645, -53.40478689619660457, -108.0204598100370816 ) ) ;
#10802 = DIRECTION ( 'NONE',  ( -1.000000000000000000, 0.000000000000000000, 0.000000000000000000 ) ) ;
#10803 = AXIS2_PLACEMENT_3D ( 'NONE', #39705, #16199, #20141 ) ;
#10804 = LINE ( 'NONE', #20657, #15696 ) ;
#10805 = ORIENTED_EDGE ( 'NONE', *, *, #9664, .T. ) ;
#10806 = ORIENTED_EDGE ( 'NONE', *, *, #39218, .F. ) ;
#10807 = DIRECTION ( 'NONE',  ( -1.000000000000000000, -0.000000000000000000, -0.000000000000000000 ) ) ;
#10808 = AXIS2_PLACEMENT_3D ( 'NONE', #2000, #38435, #22759 ) ;
#10809 = CARTESIAN_POINT ( 'NONE',  ( -17.77999999999999758, 1.836970198721029589E-15, -14.99999999999999822 ) ) ;
#10810 = AXIS2_PLACEMENT_3D ( 'NONE', #11108, #36835, #4087 ) ;
#10811 = DIRECTION ( 'NONE',  ( -1.000000000000000000, 1.577021341797097807E-16, 0.000000000000000000 ) ) ;
#10812 = ORIENTED_EDGE ( 'NONE', *, *, #24248, .F. ) ;
#10813 = VECTOR ( 'NONE', #39638, 1000.000000000000000 ) ;
#10815 = ORIENTED_EDGE ( 'NONE', *, *, #2105, .T. ) ;
#10814 = DIRECTION ( 'NONE',  ( -1.000000000000000000, 0.000000000000000000, 0.000000000000000000 ) ) ;
#10816 = CARTESIAN_POINT ( 'NONE',  ( -35.75974951333986240, 31.00000000000000355, 20.56794350806610794 ) ) ;
#10817 = VECTOR ( 'NONE', #38137, 1000.000000000000000 ) ;
#10818 = EDGE_CURVE ( 'NONE', #12767, #38581, #22980, .T. ) ;
#10819 = CARTESIAN_POINT ( 'NONE',  ( -10.00000000000000000, 0.000000000000000000, 0.000000000000000000 ) ) ;
#10820 = PRODUCT_DEFINITION ( 'UNKNOWN', '', #23306, #35965 ) ;
#10822 = ORIENTED_EDGE ( 'NONE', *, *, #13850, .T. ) ;
#10821 = DIRECTION ( 'NONE',  ( 1.000000000000000000, 0.000000000000000000, 0.000000000000000000 ) ) ;
#10823 = CIRCLE ( 'NONE', #28251, 51.99999999999999289 ) ;
#10824 = ORIENTED_EDGE ( 'NONE', *, *, #2444, .F. ) ;
#10825 = DIRECTION ( 'NONE',  ( -1.000000000000000000, 0.000000000000000000, 0.000000000000000000 ) ) ;
#10826 = CARTESIAN_POINT ( 'NONE',  ( -26.77709713318651552, 40.00000000000000000, 54.08981485145582724 ) ) ;
#10827 = EDGE_CURVE ( 'NONE', #25440, #1479, #41192, .T. ) ;
#10828 = CYLINDRICAL_SURFACE ( 'NONE', #10314, 31.49899999999999878 ) ;
#10829 = DIRECTION ( 'NONE',  ( -1.000000000000000000, 0.000000000000000000, -0.000000000000000000 ) ) ;
#10830 = ORIENTED_EDGE ( 'NONE', *, *, #3352, .F. ) ;
#10831 = CARTESIAN_POINT ( 'NONE',  ( 0.000000000000000000, -41.20225022064652620, 23.63323037071389265 ) ) ;
#10832 = EDGE_CURVE ( 'NONE', #35433, #22718, #22448, .T. ) ;
#10833 = VERTEX_POINT ( 'NONE', #3037 ) ;
#10834 = EDGE_CURVE ( 'NONE', #29542, #27165, #27980, .T. ) ;
#10835 = DIRECTION ( 'NONE',  ( -1.000000000000000000, -0.000000000000000000, -0.000000000000000000 ) ) ;
#10836 = CARTESIAN_POINT ( 'NONE',  ( 0.000000000000000000, 0.000000000000000000, 0.000000000000000000 ) ) ;
#10837 = CARTESIAN_POINT ( 'NONE',  ( -54.58798567973315841, 31.00000000000000355, -26.90590473539369754 ) ) ;
#10838 = DIRECTION ( 'NONE',  ( -1.000000000000000000, 0.000000000000000000, 0.000000000000000000 ) ) ;
#10839 = AXIS2_PLACEMENT_3D ( 'NONE', #21335, #14767, #8611 ) ;
#10840 = EDGE_LOOP ( 'NONE', ( #5014, #37198, #36272, #5738 ) ) ;
#10841 = CIRCLE ( 'NONE', #35210, 120.5010000000000190 ) ;
#10842 = CARTESIAN_POINT ( 'NONE',  ( 17.99999999999999645, 0.000000000000000000, 0.000000000000000000 ) ) ;
#10843 = VERTEX_POINT ( 'NONE', #16408 ) ;
#10844 = EDGE_CURVE ( 'NONE', #14319, #19640, #14744, .T. ) ;
#10845 = CARTESIAN_POINT ( 'NONE',  ( 76.36724925129128394, 31.00000000000000000, 58.57876755120444301 ) ) ;
#10846 = ORIENTED_EDGE ( 'NONE', *, *, #1734, .T. ) ;
#10847 = CARTESIAN_POINT ( 'NONE',  ( 17.99999999999999645, 18.42432724429473367, 30.92804820216009531 ) ) ;
#10848 = EDGE_CURVE ( 'NONE', #18098, #23944, #25889, .T. ) ;
#10849 = CARTESIAN_POINT ( 'NONE',  ( 18.00000000000000355, 44.61570720899096898, -14.73072383765582671 ) ) ;
#10850 = CARTESIAN_POINT ( 'NONE',  ( 25.34170449640226508, 31.00000000000000355, 74.97748276543396173 ) ) ;
#10852 = CARTESIAN_POINT ( 'NONE',  ( -25.88810397297939403, 40.00000000000000000, 75.89534075015936310 ) ) ;
#10851 = MECHANICAL_DESIGN_GEOMETRIC_PRESENTATION_REPRESENTATION (  '', ( #9426 ), #42861 ) ;
#10853 = LINE ( 'NONE', #40051, #8538 ) ;
#10854 = AXIS2_PLACEMENT_3D ( 'NONE', #39117, #5105, #35428 ) ;
#10855 = EDGE_LOOP ( 'NONE', ( #28597, #14293, #14708, #37760 ) ) ;
#10856 = CARTESIAN_POINT ( 'NONE',  ( 18.00000000000000355, 24.47917365150009061, -45.87777302070908547 ) ) ;
#10857 = VERTEX_POINT ( 'NONE', #34855 ) ;
#10858 = CARTESIAN_POINT ( 'NONE',  ( 18.00000000000000355, 5.667686777401707232, 46.64153600743607342 ) ) ;
#10859 = CARTESIAN_POINT ( 'NONE',  ( 0.000000000000000000, -31.17727234463623631, -111.7317219465823115 ) ) ;
#10861 = ORIENTED_EDGE ( 'NONE', *, *, #15328, .T. ) ;
#10860 = CARTESIAN_POINT ( 'NONE',  ( 18.00000000000000355, -6.109652351741465814, -46.58570277113515345 ) ) ;
#10862 = DIRECTION ( 'NONE',  ( 0.000000000000000000, 0.000000000000000000, 1.000000000000000000 ) ) ;
#10863 = VERTEX_POINT ( 'NONE', #24643 ) ;
#10864 = DIRECTION ( 'NONE',  ( -1.000000000000000000, 0.000000000000000000, 0.000000000000000000 ) ) ;
#10865 = CARTESIAN_POINT ( 'NONE',  ( -61.13902149641835138, 40.00000000000000000, -53.61851653479526902 ) ) ;
#10866 = DIRECTION ( 'NONE',  ( -1.000000000000000000, 0.000000000000000000, 0.000000000000000000 ) ) ;
#10867 =( REPRESENTATION_RELATIONSHIP ('NONE','NONE', #330, #7878 ) REPRESENTATION_RELATIONSHIP_WITH_TRANSFORMATION ( #4099 )SHAPE_REPRESENTATION_RELATIONSHIP( ) );
#10868 = ORIENTED_EDGE ( 'NONE', *, *, #9372, .T. ) ;
#10869 = EDGE_CURVE ( 'NONE', #29621, #5301, #31452, .T. ) ;
#10870 = DIRECTION ( 'NONE',  ( 1.000000000000000000, 0.000000000000000000, 0.000000000000000000 ) ) ;
#10871 = ADVANCED_FACE ( 'NONE', ( #37898 ), #11762, .T. ) ;
#10872 = DIRECTION ( 'NONE',  ( 0.000000000000000000, 0.000000000000000000, 1.000000000000000000 ) ) ;
#10873 = EDGE_CURVE ( 'NONE', #11322, #30953, #14777, .T. ) ;
#10874 = EDGE_CURVE ( 'NONE', #40855, #36072, #2197, .T. ) ;
#10875 = ADVANCED_FACE ( 'NONE', ( #31587 ), #21387, .F. ) ;
#10876 = ORIENTED_EDGE ( 'NONE', *, *, #27523, .F. ) ;
#10877 = CIRCLE ( 'NONE', #42885, 2.649999999999971934 ) ;
#10878 = VECTOR ( 'NONE', #24615, 1000.000000000000000 ) ;
#10879 = ORIENTED_EDGE ( 'NONE', *, *, #2, .F. ) ;
#10880 = LINE ( 'NONE', #41159, #33707 ) ;
#10881 = VERTEX_POINT ( 'NONE', #4968 ) ;
#10882 = CARTESIAN_POINT ( 'NONE',  ( 15.59370980024836051, 40.00000000000000000, -20.29731371384565364 ) ) ;
#10883 = PRESENTATION_LAYER_ASSIGNMENT (  '', '', ( #20652 ) ) ;
#10884 = CARTESIAN_POINT ( 'NONE',  ( 22.90854556226730310, -35.35525454449573601, -74.83297477053802993 ) ) ;
#10885 = CIRCLE ( 'NONE', #40110, 58.99999999999998579 ) ;
#10886 = CIRCLE ( 'NONE', #40084, 13.59999999999999787 ) ;
#10887 = DIRECTION ( 'NONE',  ( -1.000000000000000000, 0.000000000000000000, 0.000000000000000000 ) ) ;
#10888 = AXIS2_PLACEMENT_3D ( 'NONE', #21222, #32080, #15320 ) ;
#10889 = CARTESIAN_POINT ( 'NONE',  ( 104.9999999999993321, -2.506021480131494702E-13, -40.00000000000000000 ) ) ;
#10890 = EDGE_LOOP ( 'NONE', ( #31491, #4898, #12758, #24821 ) ) ;
#10892 = CARTESIAN_POINT ( 'NONE',  ( 9.000000000000000000, 13.57797752207923381, 33.34124362422479493 ) ) ;
#10891 = LINE ( 'NONE', #816, #23109 ) ;
#10894 = ORIENTED_EDGE ( 'NONE', *, *, #38621, .T. ) ;
#10893 = CIRCLE ( 'NONE', #12982, 0.2500000000000002220 ) ;
#10895 = CARTESIAN_POINT ( 'NONE',  ( 0.000000000000000000, 0.000000000000000000, 0.000000000000000000 ) ) ;
#10896 = CARTESIAN_POINT ( 'NONE',  ( 17.96659372829068246, 31.00000000000000355, -15.76829228678407624 ) ) ;
#10897 = ORIENTED_EDGE ( 'NONE', *, *, #14634, .F. ) ;
#10898 = DIRECTION ( 'NONE',  ( 1.058513553088275437E-16, 1.000000000000000000, -8.813324511995299047E-17 ) ) ;
#10899 = DIRECTION ( 'NONE',  ( -1.000000000000000000, 0.000000000000000000, -0.000000000000000000 ) ) ;
#10900 = CONTEXT_DEPENDENT_SHAPE_REPRESENTATION ( #18996, #32520 ) ;
#10901 = CARTESIAN_POINT ( 'NONE',  ( 0.000000000000000000, -41.62036691425604573, 113.0850832732712945 ) ) ;
#10902 = CARTESIAN_POINT ( 'NONE',  ( 4.417864660711233959, 31.00000000000000355, 67.39583333436242185 ) ) ;
#10903 = ADVANCED_FACE ( 'NONE', ( #15465 ), #35278, .T. ) ;
#10905 = ORIENTED_EDGE ( 'NONE', *, *, #33578, .T. ) ;
#10904 = VECTOR ( 'NONE', #23355, 1000.000000000000000 ) ;
#10906 = CARTESIAN_POINT ( 'NONE',  ( -30.82418422902937039, 31.00000000000000355, 26.94311707098126618 ) ) ;
#10907 = AXIS2_PLACEMENT_3D ( 'NONE', #13523, #26816, #40090 ) ;
#10908 = CARTESIAN_POINT ( 'NONE',  ( 10.81967497908702214, 40.00000000000000000, -82.17651821321413763 ) ) ;
#10909 = CIRCLE ( 'NONE', #35270, 13.59999999999999964 ) ;
#10910 = CIRCLE ( 'NONE', #16494, 116.0000000000000000 ) ;
#10911 = CIRCLE ( 'NONE', #5328, 58.99999999999999289 ) ;
#10912 = DIRECTION ( 'NONE',  ( 0.000000000000000000, 0.000000000000000000, 1.000000000000000000 ) ) ;
#10913 = CIRCLE ( 'NONE', #24168, 59.00000000000001421 ) ;
#10914 = DIRECTION ( 'NONE',  ( 1.000000000000000000, 0.000000000000000000, -0.000000000000000000 ) ) ;
#10915 = CARTESIAN_POINT ( 'NONE',  ( 8.999999999999998224, 87.74575819880270444, -75.87280091124384285 ) ) ;
#10917 = ORIENTED_EDGE ( 'NONE', *, *, #40006, .F. ) ;
#10916 = DIRECTION ( 'NONE',  ( -1.000000000000000000, 0.000000000000000000, -0.000000000000000000 ) ) ;
#10918 = LINE ( 'NONE', #33161, #33003 ) ;
#10919 = DIRECTION ( 'NONE',  ( 0.000000000000000000, -0.2631025642275088838, -0.9647678688145193693 ) ) ;
#10921 = VERTEX_POINT ( 'NONE', #5400 ) ;
#10920 = ADVANCED_BREP_SHAPE_REPRESENTATION ( '', ( #28662, #13552 ), #4416 ) ;
#10922 = CARTESIAN_POINT ( 'NONE',  ( 53.64558601427197004, 40.00000000000000000, 14.36188897069615500 ) ) ;
#10923 = DIRECTION ( 'NONE',  ( 1.000000000000000000, -0.000000000000000000, 0.000000000000000000 ) ) ;
#10924 = CARTESIAN_POINT ( 'NONE',  ( 17.99999999999999645, 35.89808275599445153, -2.706964063997355119 ) ) ;
#10925 = VERTEX_POINT ( 'NONE', #22240 ) ;
#10926 = DIRECTION ( 'NONE',  ( 0.000000000000000000, 0.000000000000000000, 1.000000000000000000 ) ) ;
#10927 = LINE ( 'NONE', #31857, #36130 ) ;
#10928 = AXIS2_PLACEMENT_3D ( 'NONE', #19991, #13427, #17143 ) ;
#10929 = EDGE_CURVE ( 'NONE', #11054, #32971, #10571, .T. ) ;
#10930 = EDGE_CURVE ( 'NONE', #15795, #18913, #36337, .T. ) ;
#10931 = ORIENTED_EDGE ( 'NONE', *, *, #38657, .T. ) ;
#10932 = CARTESIAN_POINT ( 'NONE',  ( 2.500000000000000000, 2.357898499370431722, -2.818925648462311528E-15 ) ) ;
#10933 = ORIENTED_EDGE ( 'NONE', *, *, #32405, .F. ) ;
#10934 = EDGE_CURVE ( 'NONE', #5066, #15357, #18325, .T. ) ;
#10935 = DIRECTION ( 'NONE',  ( 0.000000000000000000, 0.000000000000000000, 1.000000000000000000 ) ) ;
#10936 = ORIENTED_EDGE ( 'NONE', *, *, #4893, .T. ) ;
#10937 = DIRECTION ( 'NONE',  ( 0.000000000000000000, 3.551772811830479642E-14, -1.000000000000000000 ) ) ;
#10938 = DIRECTION ( 'NONE',  ( 1.000000000000000000, 0.000000000000000000, 0.000000000000000000 ) ) ;
#10939 = VERTEX_POINT ( 'NONE', #5174 ) ;
#10940 = CIRCLE ( 'NONE', #36685, 20.00000000000000355 ) ;
#10941 = CYLINDRICAL_SURFACE ( 'NONE', #14336, 19.99999999999999645 ) ;
#10943 = DIRECTION ( 'NONE',  ( 1.000000000000000000, 1.836909530733573776E-16, 0.000000000000000000 ) ) ;
#10942 = VECTOR ( 'NONE', #3805, 1000.000000000000000 ) ;
#10944 = VERTEX_POINT ( 'NONE', #18538 ) ;
#10945 = AXIS2_PLACEMENT_3D ( 'NONE', #7018, #43017, #13825 ) ;
#10946 = DIRECTION ( 'NONE',  ( -1.000000000000000000, -0.000000000000000000, -0.000000000000000000 ) ) ;
#10947 = AXIS2_PLACEMENT_3D ( 'NONE', #37981, #41030, #32097 ) ;
#10948 = DIRECTION ( 'NONE',  ( -1.000000000000000000, 0.000000000000000000, 0.000000000000000000 ) ) ;
#10949 = EDGE_CURVE ( 'NONE', #6259, #2948, #9191, .T. ) ;
#10950 = CARTESIAN_POINT ( 'NONE',  ( 18.00000000000000355, 46.11014828289844303, -9.022736828080878624 ) ) ;
#10951 = CIRCLE ( 'NONE', #2527, 11.00000000000000000 ) ;
#10952 = CARTESIAN_POINT ( 'NONE',  ( 9.000000000000001776, 104.6166166098445416, 50.11350645393712000 ) ) ;
#10953 = ORIENTED_EDGE ( 'NONE', *, *, #20501, .F. ) ;
#10954 = DIRECTION ( 'NONE',  ( 0.9999077429267366757, 1.283509675925409064E-16, 0.01358328513868662171 ) ) ;
#10955 = VECTOR ( 'NONE', #31637, 1000.000000000000000 ) ;
#10956 = CARTESIAN_POINT ( 'NONE',  ( 8.999999999999998224, 114.8812324315175033, 16.07179003769187986 ) ) ;
#10957 = CARTESIAN_POINT ( 'NONE',  ( -23.50435451693408950, 31.00000000000000355, 30.64856077952424940 ) ) ;
#10958 = ORIENTED_EDGE ( 'NONE', *, *, #8735, .F. ) ;
#10960 = DIRECTION ( 'NONE',  ( 0.000000000000000000, 0.000000000000000000, 1.000000000000000000 ) ) ;
#10959 = CARTESIAN_POINT ( 'NONE',  ( 0.000000000000000000, 0.04937522221168735848, -31.94951095880158576 ) ) ;
#10961 = AXIS2_PLACEMENT_3D ( 'NONE', #19121, #32386, #12764 ) ;
#10962 = CARTESIAN_POINT ( 'NONE',  ( 17.99999999999999645, 21.48775762007859669, 23.64423737150145399 ) ) ;
#10963 = ORIENTED_EDGE ( 'NONE', *, *, #9222, .T. ) ;
#10964 = FACE_OUTER_BOUND ( 'NONE', #29030, .T. ) ;
#10965 = CARTESIAN_POINT ( 'NONE',  ( -33.94102792873697183, 40.00000000000000000, -38.68473105385043453 ) ) ;
#10966 = CARTESIAN_POINT ( 'NONE',  ( -32.53655534684257589, 40.00000000000000000, -42.55839752837238166 ) ) ;
#10967 = DIRECTION ( 'NONE',  ( 0.000000000000000000, -1.000000000000000000, 5.297542245118643184E-16 ) ) ;
#10968 = DIRECTION ( 'NONE',  ( 0.000000000000000000, -0.5000000000000013323, -0.8660254037844380415 ) ) ;
#10969 = AXIS2_PLACEMENT_3D ( 'NONE', #4011, #7081, #6650 ) ;
#10970 = FACE_OUTER_BOUND ( 'NONE', #20394, .T. ) ;
#10971 = CARTESIAN_POINT ( 'NONE',  ( 18.00000000000000355, 46.19362259308845609, -8.585149169757988474 ) ) ;
#10972 = CIRCLE ( 'NONE', #31871, 59.00000000000000000 ) ;
#10973 = ORIENTED_EDGE ( 'NONE', *, *, #3804, .F. ) ;
#10974 = CARTESIAN_POINT ( 'NONE',  ( 17.42035916340572399, 40.00000000000000000, 19.85006075799527991 ) ) ;
#10975 = ORIENTED_EDGE ( 'NONE', *, *, #9285, .F. ) ;
#10976 = DIRECTION ( 'NONE',  ( -1.000000000000000000, 0.000000000000000000, 0.000000000000000000 ) ) ;
#10977 = FACE_OUTER_BOUND ( 'NONE', #28803, .T. ) ;
#10978 = AXIS2_PLACEMENT_3D ( 'NONE', #7569, #1440, #577 ) ;
#10979 = AXIS2_PLACEMENT_3D ( 'NONE', #21319, #4682, #21753 ) ;
#10980 = ORIENTED_EDGE ( 'NONE', *, *, #6501, .T. ) ;
#10981 = CIRCLE ( 'NONE', #3959, 116.0000000000000000 ) ;
#10982 = FACE_OUTER_BOUND ( 'NONE', #26734, .T. ) ;
#10983 = ADVANCED_FACE ( 'NONE', ( #1899 ), #41822, .T. ) ;
#10984 = CARTESIAN_POINT ( 'NONE',  ( 17.99999999999999645, 92.10690493017060021, 64.06707842432207656 ) ) ;
#10985 = ORIENTED_EDGE ( 'NONE', *, *, #42963, .F. ) ;
#10986 = DIRECTION ( 'NONE',  ( 0.000000000000000000, -2.305124076552231752E-14, -1.000000000000000000 ) ) ;
#10987 = AXIS2_PLACEMENT_3D ( 'NONE', #31453, #879, #1538 ) ;
#10988 = ORIENTED_EDGE ( 'NONE', *, *, #13155, .T. ) ;
#10989 = PRODUCT_DEFINITION ( 'UNKNOWN', '', #42738, #20456 ) ;
#10990 = VERTEX_POINT ( 'NONE', #8248 ) ;
#10992 = ORIENTED_EDGE ( 'NONE', *, *, #19222, .F. ) ;
#10991 = DIRECTION ( 'NONE',  ( 1.000000000000000000, 0.000000000000000000, 0.000000000000000000 ) ) ;
#10993 = AXIS2_PLACEMENT_3D ( 'NONE', #7260, #13416, #16707 ) ;
#10994 = CARTESIAN_POINT ( 'NONE',  ( 34.80713033128647993, 31.00000000000000355, 70.84796410819511436 ) ) ;
#10995 = ORIENTED_EDGE ( 'NONE', *, *, #13364, .T. ) ;
#10996 = CARTESIAN_POINT ( 'NONE',  ( -4.000000000000000000, 2.511478553582031203, -3.469254451724764543 ) ) ;
#10997 = EDGE_CURVE ( 'NONE', #15592, #17801, #95, .T. ) ;
#10998 = ORIENTED_EDGE ( 'NONE', *, *, #8559, .F. ) ;
#10999 = EDGE_CURVE ( 'NONE', #20369, #8384, #7796, .T. ) ;
#11000 = DIRECTION ( 'NONE',  ( 1.000000000000000000, 0.000000000000000000, 0.000000000000000000 ) ) ;
#11001 = VERTEX_POINT ( 'NONE', #9738 ) ;
#11002 = CARTESIAN_POINT ( 'NONE',  ( 92.49871336443506209, 39.99999999999999289, 31.53380891771211125 ) ) ;
#11003 = CIRCLE ( 'NONE', #37446, 11.08000000000000007 ) ;
#11005 = CYLINDRICAL_SURFACE ( 'NONE', #27718, 31.49899999999999878 ) ;
#11004 = DIRECTION ( 'NONE',  ( -1.000000000000000000, 0.000000000000000000, -0.000000000000000000 ) ) ;
#11006 = CARTESIAN_POINT ( 'NONE',  ( 17.99999999999999645, 0.000000000000000000, 0.000000000000000000 ) ) ;
#11007 = CARTESIAN_POINT ( 'NONE',  ( 0.000000000000000000, 35.20873326984080620, 31.88259874184042886 ) ) ;
#11008 = AXIS2_PLACEMENT_3D ( 'NONE', #29471, #12680, #17040 ) ;
#11009 = ORIENTED_EDGE ( 'NONE', *, *, #41477, .F. ) ;
#11010 = CIRCLE ( 'NONE', #31217, 20.00000000000000711 ) ;
#11011 = AXIS2_PLACEMENT_3D ( 'NONE', #24283, #11375, #1089 ) ;
#11012 = DIRECTION ( 'NONE',  ( 0.000000000000000000, 0.000000000000000000, 1.000000000000000000 ) ) ;
#11013 = AXIS2_PLACEMENT_3D ( 'NONE', #23704, #4006, #4225 ) ;
#11014 = CARTESIAN_POINT ( 'NONE',  ( 8.999999999999998224, -23.79363200506935172, -27.01597816121672224 ) ) ;
#11015 = CARTESIAN_POINT ( 'NONE',  ( -86.71682804797315214, 31.00000000000000711, 23.23408344657299196 ) ) ;
#11016 = CARTESIAN_POINT ( 'NONE',  ( -36.79328511490363240, -2.055254544495723756, -55.66638716446937707 ) ) ;
#11018 = ORIENTED_EDGE ( 'NONE', *, *, #18917, .F. ) ;
#11017 = CIRCLE ( 'NONE', #25668, 20.00000000000001066 ) ;
#11019 = CARTESIAN_POINT ( 'NONE',  ( -19.81637295874436333, 40.00000000000000000, -11.44243563873878777 ) ) ;
#11020 = EDGE_CURVE ( 'NONE', #33656, #12187, #16896, .T. ) ;
#11021 = ORIENTED_EDGE ( 'NONE', *, *, #39407, .F. ) ;
#11022 = CIRCLE ( 'NONE', #35382, 120.5010000000000190 ) ;
#11023 = VERTEX_POINT ( 'NONE', #9527 ) ;
#11024 = CYLINDRICAL_SURFACE ( 'NONE', #5998, 116.0000000000000000 ) ;
#11025 = CARTESIAN_POINT ( 'NONE',  ( 17.99999999999999645, 92.25992191227393846, 77.51514567967427638 ) ) ;
#11026 = DIRECTION ( 'NONE',  ( 1.000000000000000000, 0.000000000000000000, 0.000000000000000000 ) ) ;
#11027 = DIRECTION ( 'NONE',  ( -1.000000000000000000, -0.000000000000000000, 0.000000000000000000 ) ) ;
#11028 = ORIENTED_EDGE ( 'NONE', *, *, #18345, .F. ) ;
#11029 = DIRECTION ( 'NONE',  ( -1.000000000000000000, 0.000000000000000000, -0.000000000000000000 ) ) ;
#11030 = ORIENTED_EDGE ( 'NONE', *, *, #22559, .T. ) ;
#11031 = LINE ( 'NONE', #21741, #6834 ) ;
#11032 = CARTESIAN_POINT ( 'NONE',  ( 1.567478505476134606E-15, 4.618802153517012066, -3.433295621305382905 ) ) ;
#11033 = AXIS2_PLACEMENT_3D ( 'NONE', #27554, #40827, #5694 ) ;
#11034 = CARTESIAN_POINT ( 'NONE',  ( 18.00000000000000355, -13.85708833599937861, -45.43276465116677798 ) ) ;
#11035 = FACE_OUTER_BOUND ( 'NONE', #38057, .T. ) ;
#11036 = ORIENTED_EDGE ( 'NONE', *, *, #5799, .T. ) ;
#11037 = ORIENTED_EDGE ( 'NONE', *, *, #14908, .F. ) ;
#11038 = DIRECTION ( 'NONE',  ( 0.000000000000000000, 0.000000000000000000, 1.000000000000000000 ) ) ;
#11039 = AXIS2_PLACEMENT_3D ( 'NONE', #11341, #40982, #11133 ) ;
#11040 = EDGE_CURVE ( 'NONE', #35433, #5549, #41224, .T. ) ;
#11041 = CARTESIAN_POINT ( 'NONE',  ( 0.000000000000000000, -5.456439917445724319, 112.0647122740741963 ) ) ;
#11042 = CIRCLE ( 'NONE', #23602, 59.00000000000000000 ) ;
#11043 = CARTESIAN_POINT ( 'NONE',  ( 17.99999999999999645, -63.24564713401861837, 102.5693868539693341 ) ) ;
#11044 = AXIS2_PLACEMENT_3D ( 'NONE', #1127, #14696, #34091 ) ;
#11045 = VERTEX_POINT ( 'NONE', #33070 ) ;
#11047 = EDGE_LOOP ( 'NONE', ( #10357, #13995, #8554, #41732 ) ) ;
#11046 = CARTESIAN_POINT ( 'NONE',  ( 0.000000000000000000, -18.25486108452607681, -25.66996392254292658 ) ) ;
#11048 = CARTESIAN_POINT ( 'NONE',  ( 36.21668514974006570, 31.00000000000000355, 31.87730689759005287 ) ) ;
#11049 = CARTESIAN_POINT ( 'NONE',  ( 0.000000000000000000, 86.84764344323065188, -76.89919913989662348 ) ) ;
#11050 = AXIS2_PLACEMENT_3D ( 'NONE', #12687, #12267, #22742 ) ;
#11051 = EDGE_CURVE ( 'NONE', #18492, #42739, #13391, .T. ) ;
#11053 = FACE_OUTER_BOUND ( 'NONE', #23742, .T. ) ;
#11052 = LINE ( 'NONE', #21110, #8419 ) ;
#11054 = VERTEX_POINT ( 'NONE', #3156 ) ;
#11055 = CARTESIAN_POINT ( 'NONE',  ( 25.95756378415974908, 40.00000000000000000, 52.86556711864420066 ) ) ;
#11056 = CARTESIAN_POINT ( 'NONE',  ( 17.99999999999999645, -19.12429268481634281, -114.4126803693781085 ) ) ;
#11057 = EDGE_CURVE ( 'NONE', #37206, #23356, #29397, .T. ) ;
#11058 = DIRECTION ( 'NONE',  ( 0.000000000000000000, 0.000000000000000000, 1.000000000000000000 ) ) ;
#11059 = VERTEX_POINT ( 'NONE', #22883 ) ;
#11060 = CARTESIAN_POINT ( 'NONE',  ( 22.90854556226722138, -12.05525454449572464, -74.83297477053847047 ) ) ;
#11061 = VERTEX_POINT ( 'NONE', #36126 ) ;
#11062 =( NAMED_UNIT ( * ) PLANE_ANGLE_UNIT ( ) SI_UNIT ( $, .RADIAN. ) );
#11063 = DIRECTION ( 'NONE',  ( -1.000000000000000000, -0.000000000000000000, 0.000000000000000000 ) ) ;
#11064 = DIRECTION ( 'NONE',  ( 0.000000000000000000, 0.000000000000000000, 1.000000000000000000 ) ) ;
#11065 = CARTESIAN_POINT ( 'NONE',  ( -40.54929543462775143, 31.00000000000000355, -46.21859917192507794 ) ) ;
#11066 = AXIS2_PLACEMENT_3D ( 'NONE', #28386, #18587, #36118 ) ;
#11067 = DIRECTION ( 'NONE',  ( 0.000000000000000000, 0.000000000000000000, 1.000000000000000000 ) ) ;
#11068 = ORIENTED_EDGE ( 'NONE', *, *, #7347, .T. ) ;
#11069 = AXIS2_PLACEMENT_3D ( 'NONE', #20377, #40393, #13389 ) ;
#11070 = DIRECTION ( 'NONE',  ( -1.000000000000000000, 0.000000000000000000, 0.000000000000000000 ) ) ;
#11071 = ORIENTED_EDGE ( 'NONE', *, *, #14701, .T. ) ;
#11072 = CARTESIAN_POINT ( 'NONE',  ( -18.92511213055653130, 40.00000000000000000, 21.58621387822740090 ) ) ;
#11073 = EDGE_CURVE ( 'NONE', #29453, #5323, #31482, .T. ) ;
#11074 = ORIENTED_EDGE ( 'NONE', *, *, #13849, .T. ) ;
#11075 = DIRECTION ( 'NONE',  ( 0.000000000000000000, 0.000000000000000000, 1.000000000000000000 ) ) ;
#11076 = EDGE_CURVE ( 'NONE', #27890, #24120, #21777, .T. ) ;
#11077 = CARTESIAN_POINT ( 'NONE',  ( 0.000000000000000000, 76.48293397876373945, -82.08917884620232996 ) ) ;
#11078 = CARTESIAN_POINT ( 'NONE',  ( 57.21690105881322097, 31.00000000000000000, -50.04162206024282966 ) ) ;
#11079 = CARTESIAN_POINT ( 'NONE',  ( 37.84579180138899090, 40.00000000000000000, -65.31998993212283722 ) ) ;
#11080 = DIRECTION ( 'NONE',  ( 1.000000000000000000, 0.000000000000000000, 0.000000000000000000 ) ) ;
#11081 = ORIENTED_EDGE ( 'NONE', *, *, #17716, .T. ) ;
#11082 = DIRECTION ( 'NONE',  ( -1.000000000000000000, -0.000000000000000000, -0.000000000000000000 ) ) ;
#11083 = ORIENTED_EDGE ( 'NONE', *, *, #32405, .T. ) ;
#11084 = CARTESIAN_POINT ( 'NONE',  ( 17.99999999999999645, -57.40245293794732362, 96.40140491896615060 ) ) ;
#11085 = CARTESIAN_POINT ( 'NONE',  ( 9.000000000000000000, -35.89808275599443022, -2.706964063997606917 ) ) ;
#11087 = ORIENTED_EDGE ( 'NONE', *, *, #24169, .T. ) ;
#11086 = CARTESIAN_POINT ( 'NONE',  ( 0.2142857142857142738, -10.49781318335647917, -1.199999999999999956 ) ) ;
#11088 = DIRECTION ( 'NONE',  ( 0.000000000000000000, 0.3681245526846719240, 0.9297764858882537897 ) ) ;
#11089 = ORIENTED_EDGE ( 'NONE', *, *, #42290, .T. ) ;
#11090 = FACE_OUTER_BOUND ( 'NONE', #24452, .T. ) ;
#11091 = EDGE_CURVE ( 'NONE', #35650, #38585, #32861, .T. ) ;
#11092 = CARTESIAN_POINT ( 'NONE',  ( 91.55691129138550366, 39.99999999999999289, -24.53049628908797430 ) ) ;
#11093 = CARTESIAN_POINT ( 'NONE',  ( -15.99999999999997691, 31.00000000000000000, -4.499999999999995559 ) ) ;
#11094 = ORIENTED_EDGE ( 'NONE', *, *, #26933, .T. ) ;
#11095 = DIRECTION ( 'NONE',  ( 1.000000000000000000, 0.000000000000000000, -0.000000000000000000 ) ) ;
#11096 = AXIS2_PLACEMENT_3D ( 'NONE', #40664, #10814, #20665 ) ;
#11097 = CARTESIAN_POINT ( 'NONE',  ( 18.00000000000000355, -39.78933988720132220, 24.98727647984988920 ) ) ;
#11098 = CIRCLE ( 'NONE', #22955, 18.77999999999999048 ) ;
#11099 = VECTOR ( 'NONE', #14690, 1000.000000000000000 ) ;
#11100 = ADVANCED_FACE ( 'NONE', ( #29606 ), #42878, .F. ) ;
#11101 = DIRECTION ( 'NONE',  ( -1.000000000000000000, 0.000000000000000000, -0.000000000000000000 ) ) ;
#11102 = ORIENTED_EDGE ( 'NONE', *, *, #31360, .T. ) ;
#11103 = CYLINDRICAL_SURFACE ( 'NONE', #998, 51.99999999999999289 ) ;
#11104 = ORIENTED_EDGE ( 'NONE', *, *, #25870, .F. ) ;
#11105 = CARTESIAN_POINT ( 'NONE',  ( -31.36635120280305955, 40.00000000000000000, -8.451140850655482595 ) ) ;
#11106 = DIRECTION ( 'NONE',  ( 0.000000000000000000, 0.000000000000000000, 1.000000000000000000 ) ) ;
#11107 = EDGE_CURVE ( 'NONE', #18324, #27302, #41918, .T. ) ;
#11108 = CARTESIAN_POINT ( 'NONE',  ( 0.000000000000000000, 0.000000000000000000, 0.000000000000000000 ) ) ;
#11109 = EDGE_CURVE ( 'NONE', #4179, #17128, #37034, .T. ) ;
#11110 = CARTESIAN_POINT ( 'NONE',  ( -75.96080130434582145, -14.05525454449571221, 14.45886780445738218 ) ) ;
#11111 = ORIENTED_EDGE ( 'NONE', *, *, #30468, .T. ) ;
#11113 = DIRECTION ( 'NONE',  ( 0.000000000000000000, 0.000000000000000000, 1.000000000000000000 ) ) ;
#11112 = CARTESIAN_POINT ( 'NONE',  ( 0.000000000000000000, 0.000000000000000000, 0.000000000000000000 ) ) ;
#11114 = EDGE_LOOP ( 'NONE', ( #17658, #24600, #29715, #368 ) ) ;
#11115 = DIRECTION ( 'NONE',  ( 0.000000000000000000, 0.2631025642275152121, 0.9647678688145175929 ) ) ;
#11116 = CARTESIAN_POINT ( 'NONE',  ( -28.63582912838407069, 31.00000000000000355, 7.677129336082076705 ) ) ;
#11117 = ORIENTED_EDGE ( 'NONE', *, *, #12261, .F. ) ;
#11118 = CARTESIAN_POINT ( 'NONE',  ( 18.00000000000000355, -32.32520163883560826, -34.09746168776070618 ) ) ;
#11119 = DIRECTION ( 'NONE',  ( 0.000000000000000000, 0.000000000000000000, 1.000000000000000000 ) ) ;
#11120 = CONTEXT_DEPENDENT_SHAPE_REPRESENTATION ( #9445, #29775 ) ;
#11121 = DIRECTION ( 'NONE',  ( -1.000000000000000000, 0.000000000000000000, -0.000000000000000000 ) ) ;
#11122 = CARTESIAN_POINT ( 'NONE',  ( 65.81435062899562638, 31.00000000000000000, 37.99825742654716976 ) ) ;
#11123 = EDGE_CURVE ( 'NONE', #34690, #38106, #14082, .T. ) ;
#11125 = EDGE_CURVE ( 'NONE', #17817, #42716, #26341, .T. ) ;
#11124 = AXIS2_PLACEMENT_3D ( 'NONE', #31687, #41713, #38001 ) ;
#11126 = ORIENTED_EDGE ( 'NONE', *, *, #10929, .F. ) ;
#11127 = CARTESIAN_POINT ( 'NONE',  ( -35.75974951333986240, 31.00000000000000355, 20.56794350806610794 ) ) ;
#11128 = EDGE_CURVE ( 'NONE', #7493, #35542, #28726, .T. ) ;
#11129 = EDGE_CURVE ( 'NONE', #28874, #23736, #28037, .T. ) ;
#11130 = CARTESIAN_POINT ( 'NONE',  ( 24.81019160154284720, 40.00000000000000000, 73.04493173762017477 ) ) ;
#11131 = AXIS2_PLACEMENT_3D ( 'NONE', #2389, #11843, #22531 ) ;
#11132 = CARTESIAN_POINT ( 'NONE',  ( 0.000000000000000000, 84.09610293794170843, -74.27057253242929846 ) ) ;
#11133 = DIRECTION ( 'NONE',  ( 1.000000000000000000, 0.000000000000000000, 0.000000000000000000 ) ) ;
#11134 = CYLINDRICAL_SURFACE ( 'NONE', #21288, 20.00000000000000355 ) ;
#11136 = VERTEX_POINT ( 'NONE', #32654 ) ;
#11135 = LINE ( 'NONE', #37512, #41801 ) ;
#11137 = DIRECTION ( 'NONE',  ( -0.000000000000000000, -0.000000000000000000, 1.000000000000000000 ) ) ;
#11138 = CARTESIAN_POINT ( 'NONE',  ( 0.3208286057739604957, -4.433571671609698228, -0.3503314178412692548 ) ) ;
#11139 = EDGE_LOOP ( 'NONE', ( #5539, #6659, #8406, #29344 ) ) ;
#11140 = CARTESIAN_POINT ( 'NONE',  ( -58.48566925782336057, 40.00000000000000711, -15.65830181329500803 ) ) ;
#11141 = DIRECTION ( 'NONE',  ( 0.000000000000000000, 0.7164567402983114119, 0.6976315211349884970 ) ) ;
#11142 = DIRECTION ( 'NONE',  ( -1.000000000000000000, 0.000000000000000000, 0.000000000000000000 ) ) ;
#11143 = ORIENTED_EDGE ( 'NONE', *, *, #22349, .F. ) ;
#11144 = CARTESIAN_POINT ( 'NONE',  ( 58.80287614962789888, -12.05525454449571932, 69.29271901957253021 ) ) ;
#11145 = CARTESIAN_POINT ( 'NONE',  ( 0.000000000000000000, 0.000000000000000000, -1.199999999999999956 ) ) ;
#11146 = ORIENTED_EDGE ( 'NONE', *, *, #30193, .F. ) ;
#11147 = DIRECTION ( 'NONE',  ( 0.000000000000000000, 0.000000000000000000, 1.000000000000000000 ) ) ;
#11148 = ORIENTED_EDGE ( 'NONE', *, *, #39918, .T. ) ;
#11149 = EDGE_CURVE ( 'NONE', #32652, #26461, #30112, .T. ) ;
#11150 = FACE_OUTER_BOUND ( 'NONE', #25415, .T. ) ;
#11152 = VERTEX_POINT ( 'NONE', #38970 ) ;
#11151 = CIRCLE ( 'NONE', #3443, 0.08000000000000020983 ) ;
#11153 = CARTESIAN_POINT ( 'NONE',  ( 17.99999999999999645, 28.57802095670106723, -14.28532136906642691 ) ) ;
#11154 = AXIS2_PLACEMENT_3D ( 'NONE', #5375, #18738, #14576 ) ;
#11155 = CARTESIAN_POINT ( 'NONE',  ( 17.99999999999999645, 0.000000000000000000, 0.000000000000000000 ) ) ;
#11156 = ORIENTED_EDGE ( 'NONE', *, *, #1304, .T. ) ;
#11157 = DIRECTION ( 'NONE',  ( 1.000000000000000000, -0.000000000000000000, -0.000000000000000000 ) ) ;
#11158 = CARTESIAN_POINT ( 'NONE',  ( 17.99999999999999645, 0.000000000000000000, 0.000000000000000000 ) ) ;
#11159 = VERTEX_POINT ( 'NONE', #25719 ) ;
#11160 = DIRECTION ( 'NONE',  ( 0.000000000000000000, 0.000000000000000000, 1.000000000000000000 ) ) ;
#11161 = DIRECTION ( 'NONE',  ( 0.000000000000000000, 0.000000000000000000, 1.000000000000000000 ) ) ;
#11162 = DIRECTION ( 'NONE',  ( 0.000000000000000000, 0.000000000000000000, 1.000000000000000000 ) ) ;
#11163 = DIRECTION ( 'NONE',  ( -1.000000000000000000, -0.000000000000000000, -0.000000000000000000 ) ) ;
#11164 = VERTEX_POINT ( 'NONE', #5812 ) ;
#11165 = CARTESIAN_POINT ( 'NONE',  ( -106.4195705685756081, 1.999999999999996669, -106.4195705685752529 ) ) ;
#11166 = CARTESIAN_POINT ( 'NONE',  ( 0.000000000000000000, 0.000000000000000000, 0.000000000000000000 ) ) ;
#11167 = CARTESIAN_POINT ( 'NONE',  ( -36.61132647064156487, 31.00000000000000355, -18.04288060775211378 ) ) ;
#11168 = ORIENTED_EDGE ( 'NONE', *, *, #25701, .F. ) ;
#11170 = DIRECTION ( 'NONE',  ( 0.000000000000000000, -0.5076658003388292428, -0.8615540813938125098 ) ) ;
#11169 = CARTESIAN_POINT ( 'NONE',  ( 18.00000000000000355, 47.49120266317495265, -0.8606222198177008176 ) ) ;
#11171 = CARTESIAN_POINT ( 'NONE',  ( 0.000000000000000000, -47.31079789947556691, 105.9135893174949530 ) ) ;
#11172 = EDGE_CURVE ( 'NONE', #38476, #22945, #9089, .T. ) ;
#11173 = ORIENTED_EDGE ( 'NONE', *, *, #3008, .F. ) ;
#11174 = ADVANCED_FACE ( 'NONE', ( #9300 ), #2732, .T. ) ;
#11175 = EDGE_CURVE ( 'NONE', #16471, #30860, #25252, .T. ) ;
#11176 = CYLINDRICAL_SURFACE ( 'NONE', #38695, 13.59999999999999964 ) ;
#11177 = CARTESIAN_POINT ( 'NONE',  ( -21.36651465564686703, 40.00000000000000000, 43.35257367405362317 ) ) ;
#11178 = CARTESIAN_POINT ( 'NONE',  ( -13.93478910046542829, 40.00000000000000000, -52.37520058408175316 ) ) ;
#11179 = EDGE_CURVE ( 'NONE', #39905, #10925, #39819, .T. ) ;
#11180 = VECTOR ( 'NONE', #42796, 1000.000000000000000 ) ;
#11181 = VECTOR ( 'NONE', #31103, 1000.000000000000000 ) ;
#11182 = DIRECTION ( 'NONE',  ( 1.000000000000000000, -0.000000000000000000, 0.000000000000000000 ) ) ;
#11183 = DIRECTION ( 'NONE',  ( -1.000000000000000000, -0.000000000000000000, -0.000000000000000000 ) ) ;
#11184 = AXIS2_PLACEMENT_3D ( 'NONE', #37531, #5017, #27745 ) ;
#11185 = AXIS2_PLACEMENT_3D ( 'NONE', #9175, #26202, #39051 ) ;
#11186 = EDGE_CURVE ( 'NONE', #6140, #25968, #6383, .T. ) ;
#11187 = CARTESIAN_POINT ( 'NONE',  ( 9.000000000000001776, 39.64889472655780622, -33.64468972902464117 ) ) ;
#11188 = DIRECTION ( 'NONE',  ( -1.000000000000000000, 0.000000000000000000, 0.000000000000000000 ) ) ;
#11189 = VERTEX_POINT ( 'NONE', #313 ) ;
#11190 = CARTESIAN_POINT ( 'NONE',  ( -20.07939870814534089, 40.00000000000000000, -2.638545259751242877 ) ) ;
#11191 = ORIENTED_EDGE ( 'NONE', *, *, #12794, .F. ) ;
#11192 = CYLINDRICAL_SURFACE ( 'NONE', #15324, 13.59999999999999964 ) ;
#11193 = CARTESIAN_POINT ( 'NONE',  ( -3.436319922987618902, 2.634841920961291439, -3.531542292955721862 ) ) ;
#11194 = EDGE_CURVE ( 'NONE', #27822, #23124, #7097, .T. ) ;
#11195 = ORIENTED_EDGE ( 'NONE', *, *, #22036, .F. ) ;
#11196 = FACE_OUTER_BOUND ( 'NONE', #17963, .T. ) ;
#11197 = DIRECTION ( 'NONE',  ( 0.000000000000000000, 0.9510565162951544194, -0.3090169943749447867 ) ) ;
#11198 = ORIENTED_EDGE ( 'NONE', *, *, #38098, .F. ) ;
#11199 = DIRECTION ( 'NONE',  ( -1.000000000000000000, 3.009274222672345096E-17, 0.000000000000000000 ) ) ;
#11200 = ORIENTED_EDGE ( 'NONE', *, *, #35960, .T. ) ;
#11201 = VERTEX_POINT ( 'NONE', #24153 ) ;
#11202 = CARTESIAN_POINT ( 'NONE',  ( -10.00000000000000000, 0.000000000000000000, 0.000000000000000000 ) ) ;
#11204 = AXIS2_PLACEMENT_3D ( 'NONE', #7653, #37964, #24940 ) ;
#11203 = CARTESIAN_POINT ( 'NONE',  ( 74.15939217261870908, 31.00000000000000000, -19.75058139460982432 ) ) ;
#11205 = ORIENTED_EDGE ( 'NONE', *, *, #38450, .T. ) ;
#11206 = DIRECTION ( 'NONE',  ( 1.000000000000000000, 0.000000000000000000, 0.000000000000000000 ) ) ;
#11207 = EDGE_CURVE ( 'NONE', #42728, #19539, #33504, .T. ) ;
#11208 = ADVANCED_FACE ( 'NONE', ( #27196 ), #37420, .F. ) ;
#11209 = AXIS2_PLACEMENT_3D ( 'NONE', #30688, #23730, #764 ) ;
#11210 = DIRECTION ( 'NONE',  ( 0.000000000000000000, -0.3641605752528102591, -0.9313361774523430947 ) ) ;
#11211 = ORIENTED_EDGE ( 'NONE', *, *, #32377, .F. ) ;
#11212 = CARTESIAN_POINT ( 'NONE',  ( -4.197393957002303999, 0.4069871074557429025, -3.503767560748926257 ) ) ;
#11213 = VERTEX_POINT ( 'NONE', #40672 ) ;
#11214 = CARTESIAN_POINT ( 'NONE',  ( -55.31949386280459180, 40.00000000000000711, 71.91600076662652441 ) ) ;
#11215 = CIRCLE ( 'NONE', #38373, 59.00000000000000711 ) ;
#11216 = VECTOR ( 'NONE', #5118, 1000.000000000000000 ) ;
#11218 = DIRECTION ( 'NONE',  ( 0.000000000000000000, 0.000000000000000000, 1.000000000000000000 ) ) ;
#11217 = DIRECTION ( 'NONE',  ( 0.000000000000000000, 0.000000000000000000, 1.000000000000000000 ) ) ;
#11219 = FACE_OUTER_BOUND ( 'NONE', #24859, .T. ) ;
#11220 = CARTESIAN_POINT ( 'NONE',  ( 17.99999999999999645, 114.1529630473449686, 38.59523323561477781 ) ) ;
#11221 = VERTEX_POINT ( 'NONE', #36773 ) ;
#11222 = ORIENTED_EDGE ( 'NONE', *, *, #788, .T. ) ;
#11223 = CARTESIAN_POINT ( 'NONE',  ( 0.000000000000000000, 22.43957647427161461, 41.27978878573636479 ) ) ;
#11224 = CARTESIAN_POINT ( 'NONE',  ( -55.79431841392906222, 31.00000000000000355, -72.71543055464235294 ) ) ;
#11225 = DIRECTION ( 'NONE',  ( 1.000000000000000000, 0.000000000000000000, 0.000000000000000000 ) ) ;
#11226 = ORIENTED_EDGE ( 'NONE', *, *, #4759, .T. ) ;
#11227 = ADVANCED_FACE ( 'NONE', ( #547, #6667 ), #16962, .F. ) ;
#11228 = CARTESIAN_POINT ( 'NONE',  ( 19.49047152472583022, 40.00000000000000000, -17.07028940128360617 ) ) ;
#11229 = ORIENTED_EDGE ( 'NONE', *, *, #32748, .T. ) ;
#11230 = ORIENTED_EDGE ( 'NONE', *, *, #33183, .T. ) ;
#11231 = CARTESIAN_POINT ( 'NONE',  ( 0.000000000000000000, 0.000000000000000000, 116.0000000000000000 ) ) ;
#11232 = CARTESIAN_POINT ( 'NONE',  ( 0.000000000000000000, -5.667686777402029641, 46.64153600743603789 ) ) ;
#11233 = CARTESIAN_POINT ( 'NONE',  ( 9.000000000000001776, -18.53613841426756181, -48.58406706613921244 ) ) ;
#11234 = FACE_BOUND ( 'NONE', #34698, .T. ) ;
#11235 = AXIS2_PLACEMENT_3D ( 'NONE', #11060, #21566, #11486 ) ;
#11236 = EDGE_CURVE ( 'NONE', #25205, #8724, #40256, .T. ) ;
#11237 = ORIENTED_EDGE ( 'NONE', *, *, #175, .F. ) ;
#11238 = CARTESIAN_POINT ( 'NONE',  ( 18.00000000000000355, 20.99948489194423118, 42.60488980472788967 ) ) ;
#11239 = ORIENTED_EDGE ( 'NONE', *, *, #32486, .T. ) ;
#11240 = CARTESIAN_POINT ( 'NONE',  ( 158.4999999999992042, -1.991533622299105221E-13, 6.999999999999939604 ) ) ;
#11241 = AXIS2_PLACEMENT_3D ( 'NONE', #4690, #21553, #25664 ) ;
#11242 = PLANE ( 'NONE',  #15846 ) ;
#11243 = VECTOR ( 'NONE', #39128, 1000.000000000000000 ) ;
#11244 = EDGE_CURVE ( 'NONE', #7856, #36681, #32214, .T. ) ;
#11245 = CARTESIAN_POINT ( 'NONE',  ( -2.500000000000000888, 0.000000000000000000, -4.974599999999998801 ) ) ;
#11246 = VECTOR ( 'NONE', #22230, 1000.000000000000000 ) ;
#11247 = DIRECTION ( 'NONE',  ( -0.000000000000000000, -0.000000000000000000, -1.000000000000000000 ) ) ;
#11248 = ORIENTED_EDGE ( 'NONE', *, *, #31738, .F. ) ;
#11249 = ORIENTED_EDGE ( 'NONE', *, *, #32054, .T. ) ;
#11250 = DIRECTION ( 'NONE',  ( -1.000000000000000000, -0.000000000000000000, 0.000000000000000000 ) ) ;
#11251 = FACE_OUTER_BOUND ( 'NONE', #2273, .T. ) ;
#11252 = CIRCLE ( 'NONE', #6333, 20.00000000000000000 ) ;
#11253 = ORIENTED_EDGE ( 'NONE', *, *, #41403, .F. ) ;
#11255 = ORIENTED_EDGE ( 'NONE', *, *, #22375, .T. ) ;
#11254 = DIRECTION ( 'NONE',  ( 0.000000000000000000, 0.000000000000000000, 1.000000000000000000 ) ) ;
#11256 = CARTESIAN_POINT ( 'NONE',  ( 27.84166646522859878, 31.00000000000000355, -36.16032403484085478 ) ) ;
#11257 = CARTESIAN_POINT ( 'NONE',  ( 0.000000000000000000, 0.000000000000000000, 0.000000000000000000 ) ) ;
#11258 = AXIS2_PLACEMENT_3D ( 'NONE', #9653, #12722, #22778 ) ;
#11260 = FACE_OUTER_BOUND ( 'NONE', #36151, .T. ) ;
#11259 = DIRECTION ( 'NONE',  ( 0.000000000000000000, 0.000000000000000000, 1.000000000000000000 ) ) ;
#11261 = VERTEX_POINT ( 'NONE', #36988 ) ;
#11262 = DIRECTION ( 'NONE',  ( 0.000000000000000000, 0.000000000000000000, 1.000000000000000000 ) ) ;
#11263 = CARTESIAN_POINT ( 'NONE',  ( -48.52617905696451572, 40.00000000000000000, 37.10499320822106029 ) ) ;
#11264 = FACE_OUTER_BOUND ( 'NONE', #24099, .T. ) ;
#11265 = DIRECTION ( 'NONE',  ( 1.000000000000000000, -0.000000000000000000, -0.000000000000000000 ) ) ;
#11266 = ORIENTED_EDGE ( 'NONE', *, *, #41839, .T. ) ;
#11267 = CARTESIAN_POINT ( 'NONE',  ( 0.000000000000000000, 0.04937522221122418731, 31.94951095880159286 ) ) ;
#11268 = EDGE_LOOP ( 'NONE', ( #9654, #38600, #3519, #12393 ) ) ;
#11269 = AXIS2_PLACEMENT_3D ( 'NONE', #31279, #11000, #21064 ) ;
#11270 = CARTESIAN_POINT ( 'NONE',  ( 18.00000000000000355, -26.17370628620627571, -39.63700417846190049 ) ) ;
#11271 = DIRECTION ( 'NONE',  ( 0.000000000000000000, -0.9574220383620022368, -0.2886919473396314384 ) ) ;
#11272 = VECTOR ( 'NONE', #29077, 1000.000000000000000 ) ;
#11273 = CARTESIAN_POINT ( 'NONE',  ( -57.67632858778466698, 31.00000000000000711, 15.45560639130400205 ) ) ;
#11274 = DIRECTION ( 'NONE',  ( 0.000000000000000000, 0.000000000000000000, 1.000000000000000000 ) ) ;
#11275 = EDGE_LOOP ( 'NONE', ( #20618, #36972, #29612, #29825 ) ) ;
#11276 = ADVANCED_FACE ( 'NONE', ( #16752 ), #17402, .T. ) ;
#11277 = ORIENTED_EDGE ( 'NONE', *, *, #6640, .F. ) ;
#11278 = CARTESIAN_POINT ( 'NONE',  ( -14.08558183832706234, 40.00000000000000000, -28.55406316770863739 ) ) ;
#11279 = AXIS2_PLACEMENT_3D ( 'NONE', #13859, #34316, #4412 ) ;
#11280 = ORIENTED_EDGE ( 'NONE', *, *, #4813, .F. ) ;
#11281 = CARTESIAN_POINT ( 'NONE',  ( -2.649999999999987477, -150.5000000000000284, 10.00000000000000000 ) ) ;
#11282 = DIRECTION ( 'NONE',  ( -1.000000000000000000, -0.000000000000000000, -0.000000000000000000 ) ) ;
#11283 = CARTESIAN_POINT ( 'NONE',  ( 86.90011881125596460, 31.00000000000000000, -5.573058087428397478 ) ) ;
#11284 = CARTESIAN_POINT ( 'NONE',  ( 82.09539989320980169, 39.99999999999999289, -27.75477508813643723 ) ) ;
#11285 = CARTESIAN_POINT ( 'NONE',  ( 18.00000000000000355, -39.55064067543046491, -25.36340625197400200 ) ) ;
#11286 = EDGE_CURVE ( 'NONE', #10372, #7044, #20452, .T. ) ;
#11287 = ORIENTED_EDGE ( 'NONE', *, *, #42457, .T. ) ;
#11288 = DIRECTION ( 'NONE',  ( 1.000000000000000000, 0.000000000000000000, 0.000000000000000000 ) ) ;
#11289 = ORIENTED_EDGE ( 'NONE', *, *, #7650, .T. ) ;
#11290 = CARTESIAN_POINT ( 'NONE',  ( 17.99999999999999645, 0.000000000000000000, 0.000000000000000000 ) ) ;
#11291 = EDGE_CURVE ( 'NONE', #32870, #40129, #28068, .T. ) ;
#11292 = LINE ( 'NONE', #1660, #31056 ) ;
#11294 = ORIENTED_EDGE ( 'NONE', *, *, #28181, .F. ) ;
#11293 = CARTESIAN_POINT ( 'NONE',  ( 17.99999999999999645, -29.86146780999875716, -112.0905559814581665 ) ) ;
#11295 = ADVANCED_FACE ( 'NONE', ( #13899 ), #10599, .F. ) ;
#11296 = DIRECTION ( 'NONE',  ( 0.000000000000000000, 0.000000000000000000, 1.000000000000000000 ) ) ;
#11297 = ORIENTED_EDGE ( 'NONE', *, *, #15080, .T. ) ;
#11298 = DIRECTION ( 'NONE',  ( -1.000000000000000000, -0.000000000000000000, -0.000000000000000000 ) ) ;
#11299 = CARTESIAN_POINT ( 'NONE',  ( 70.70367055548476287, 39.99999999999999289, -62.02616482874480397 ) ) ;
#11300 = CARTESIAN_POINT ( 'NONE',  ( 0.000000000000000000, -9.744342220503709129, 46.48873837489794880 ) ) ;
#11301 = AXIS2_PLACEMENT_3D ( 'NONE', #3694, #17072, #10052 ) ;
#11302 = VECTOR ( 'NONE', #35691, 1000.000000000000000 ) ;
#11303 = ORIENTED_EDGE ( 'NONE', *, *, #35031, .T. ) ;
#11304 = DIRECTION ( 'NONE',  ( 0.000000000000000000, 0.000000000000000000, 1.000000000000000000 ) ) ;
#11305 = DIRECTION ( 'NONE',  ( 0.000000000000000000, 0.000000000000000000, 1.000000000000000000 ) ) ;
#11306 = AXIS2_PLACEMENT_3D ( 'NONE', #25331, #4563, #27951 ) ;
#11308 = DIRECTION ( 'NONE',  ( 1.000000000000000000, 0.000000000000000000, 0.000000000000000000 ) ) ;
#11307 = DIRECTION ( 'NONE',  ( -1.000000000000000000, 0.000000000000000000, 0.000000000000000000 ) ) ;
#11309 = ORIENTED_EDGE ( 'NONE', *, *, #35579, .T. ) ;
#11310 = CARTESIAN_POINT ( 'NONE',  ( 17.99999999999999645, -74.56001736500559218, -88.86396238369110279 ) ) ;
#11312 = EDGE_LOOP ( 'NONE', ( #32532, #26103, #40500, #38457 ) ) ;
#11311 = EDGE_CURVE ( 'NONE', #4861, #39523, #23010, .T. ) ;
#11313 = DIRECTION ( 'NONE',  ( 1.000000000000000000, -1.373900992973641868E-15, -3.469446951953632924E-16 ) ) ;
#11314 = CARTESIAN_POINT ( 'NONE',  ( -27.06829236441420861, 40.00000000000000000, 15.58100167311933149 ) ) ;
#11315 = FACE_OUTER_BOUND ( 'NONE', #12946, .T. ) ;
#11316 = EDGE_CURVE ( 'NONE', #37373, #14052, #9865, .T. ) ;
#11317 = LINE ( 'NONE', #35284, #16615 ) ;
#11318 = DIRECTION ( 'NONE',  ( 0.000000000000000000, 0.000000000000000000, 1.000000000000000000 ) ) ;
#11319 = ORIENTED_EDGE ( 'NONE', *, *, #34572, .T. ) ;
#11321 = CARTESIAN_POINT ( 'NONE',  ( 3.436319922986518449, -2.634841920959471562, -3.531542292954761741 ) ) ;
#11320 = DIRECTION ( 'NONE',  ( 0.000000000000000000, 0.000000000000000000, 1.000000000000000000 ) ) ;
#11322 = VERTEX_POINT ( 'NONE', #36047 ) ;
#11323 = LINE ( 'NONE', #31597, #42679 ) ;
#11324 = CARTESIAN_POINT ( 'NONE',  ( 0.000000000000000000, -101.1249659627852679, -48.60055280209521555 ) ) ;
#11325 = CARTESIAN_POINT ( 'NONE',  ( 23.22631124480444598, 31.00000000000000355, -7.893869537065737241 ) ) ;
#11326 = ORIENTED_EDGE ( 'NONE', *, *, #605, .F. ) ;
#11327 = FACE_OUTER_BOUND ( 'NONE', #2998, .T. ) ;
#11328 = CARTESIAN_POINT ( 'NONE',  ( 17.99999999999999645, -27.83061035786878890, -117.2431154827800270 ) ) ;
#11329 = ITEM_DEFINED_TRANSFORMATION ( 'NONE', 'NONE', #32334,  #13552 ) ;
#11330 = CARTESIAN_POINT ( 'NONE',  ( 17.99999999999999645, 72.00556975657821113, -86.04342158279314390 ) ) ;
#11331 = CIRCLE ( 'NONE', #37088, 59.00000000000001421 ) ;
#11332 = CARTESIAN_POINT ( 'NONE',  ( 41.75688748258168914, 31.00000000000000355, -72.32308762158416471 ) ) ;
#11333 = AXIS2_PLACEMENT_3D ( 'NONE', #16676, #42585, #35818 ) ;
#11334 = ORIENTED_EDGE ( 'NONE', *, *, #15325, .F. ) ;
#11335 = CARTESIAN_POINT ( 'NONE',  ( -7.911223860809958097, 31.00000000000000355, 59.30865348673673765 ) ) ;
#11336 = AXIS2_PLACEMENT_3D ( 'NONE', #27237, #40949, #17449 ) ;
#11337 = CARTESIAN_POINT ( 'NONE',  ( -85.90019077458921970, 40.00000000000000711, -29.16093118951848240 ) ) ;
#11338 = EDGE_CURVE ( 'NONE', #30034, #41672, #4319, .T. ) ;
#11339 = AXIS2_PLACEMENT_3D ( 'NONE', #37102, #20566, #26872 ) ;
#11340 = DIRECTION ( 'NONE',  ( 0.000000000000000000, -0.5000000000000013323, -0.8660254037844380415 ) ) ;
#11341 = CARTESIAN_POINT ( 'NONE',  ( 0.000000000000000000, 0.000000000000000000, -0.3080913168122742518 ) ) ;
#11342 = EDGE_CURVE ( 'NONE', #32645, #1677, #23184, .T. ) ;
#11343 = CARTESIAN_POINT ( 'NONE',  ( 18.00000000000000355, 0.000000000000000000, 0.000000000000000000 ) ) ;
#11345 = ORIENTED_EDGE ( 'NONE', *, *, #39785, .F. ) ;
#11344 = DIRECTION ( 'NONE',  ( 0.000000000000000000, 0.000000000000000000, 1.000000000000000000 ) ) ;
#11346 = EDGE_CURVE ( 'NONE', #19737, #18, #12528, .T. ) ;
#11347 = DIRECTION ( 'NONE',  ( 0.000000000000000000, 0.000000000000000000, 1.000000000000000000 ) ) ;
#11348 = FACE_OUTER_BOUND ( 'NONE', #16599, .T. ) ;
#11349 = ORIENTED_EDGE ( 'NONE', *, *, #34542, .F. ) ;
#11350 = CARTESIAN_POINT ( 'NONE',  ( -4.090615425948576522, 40.00000000000000000, -62.39583333438447710 ) ) ;
#11351 = DIRECTION ( 'NONE',  ( 1.000000000000000000, -0.000000000000000000, -0.000000000000000000 ) ) ;
#11352 = EDGE_LOOP ( 'NONE', ( #19713, #16182, #5724, #3757 ) ) ;
#11353 = DIRECTION ( 'NONE',  ( 1.000000000000000000, 0.000000000000000000, 0.000000000000000000 ) ) ;
#11354 = CARTESIAN_POINT ( 'NONE',  ( -4.000000000000000000, -0.7890432684750890990, -0.04868663549882315533 ) ) ;
#11355 = VERTEX_POINT ( 'NONE', #2438 ) ;
#11356 = CARTESIAN_POINT ( 'NONE',  ( 103.7695705685734708, 106.4195705685780382, 7.000000000000249578 ) ) ;
#11357 = ORIENTED_EDGE ( 'NONE', *, *, #25958, .T. ) ;
#11358 = AXIS2_PLACEMENT_3D ( 'NONE', #42891, #9747, #35498 ) ;
#11359 = CYLINDRICAL_SURFACE ( 'NONE', #24728, 59.00000000000000000 ) ;
#11360 = ORIENTED_EDGE ( 'NONE', *, *, #42578, .T. ) ;
#11361 = DIRECTION ( 'NONE',  ( -1.000000000000000000, 0.000000000000000000, 0.000000000000000000 ) ) ;
#11362 = DIRECTION ( 'NONE',  ( 0.000000000000000000, 0.000000000000000000, 1.000000000000000000 ) ) ;
#11363 = ORIENTED_EDGE ( 'NONE', *, *, #42791, .F. ) ;
#11364 = ADVANCED_FACE ( 'NONE', ( #19946 ), #39947, .T. ) ;
#11365 = EDGE_CURVE ( 'NONE', #31678, #18694, #32988, .T. ) ;
#11366 = VECTOR ( 'NONE', #6024, 1000.000000000000000 ) ;
#11367 = DIRECTION ( 'NONE',  ( -1.000000000000000000, 0.000000000000000000, 0.000000000000000000 ) ) ;
#11368 = DIRECTION ( 'NONE',  ( 0.000000000000000000, 0.000000000000000000, 1.000000000000000000 ) ) ;
#11369 = VERTEX_POINT ( 'NONE', #26466 ) ;
#11370 = CARTESIAN_POINT ( 'NONE',  ( -22.00000000000000000, 40.00000000000000000, 1.283214542831021765 ) ) ;
#11371 = AXIS2_PLACEMENT_3D ( 'NONE', #9596, #36190, #22085 ) ;
#11372 = DIRECTION ( 'NONE',  ( 0.000000000000000000, -0.3681245526846852467, 0.9297764858882484607 ) ) ;
#11373 = ORIENTED_EDGE ( 'NONE', *, *, #22672, .F. ) ;
#11374 = DIRECTION ( 'NONE',  ( 0.000000000000000000, 0.000000000000000000, 1.000000000000000000 ) ) ;
#11375 = DIRECTION ( 'NONE',  ( -3.009274222672345096E-17, -1.000000000000000000, 2.455023325076455345E-18 ) ) ;
#11376 = ORIENTED_EDGE ( 'NONE', *, *, #26800, .F. ) ;
#11377 =( NAMED_UNIT ( * ) PLANE_ANGLE_UNIT ( ) SI_UNIT ( $, .RADIAN. ) );
#11378 = EDGE_CURVE ( 'NONE', #33094, #37148, #42795, .T. ) ;
#11379 = CYLINDRICAL_SURFACE ( 'NONE', #9988, 59.00000000000000000 ) ;
#11380 = EDGE_CURVE ( 'NONE', #20659, #32376, #33604, .T. ) ;
#11381 = CARTESIAN_POINT ( 'NONE',  ( -44.11856065373272173, 31.00000000000000355, -25.46949057303769948 ) ) ;
#11382 = EDGE_LOOP ( 'NONE', ( #31143, #30136, #31823, #33171 ) ) ;
#11384 = DIRECTION ( 'NONE',  ( 1.000000000000000000, 0.000000000000000000, 0.000000000000000000 ) ) ;
#11383 = DIRECTION ( 'NONE',  ( -1.000000000000000000, 0.000000000000000000, 0.000000000000000000 ) ) ;
#11385 = CARTESIAN_POINT ( 'NONE',  ( 17.99999999999999645, 67.32409792376626001, -89.75376489259298296 ) ) ;
#11386 = ORIENTED_EDGE ( 'NONE', *, *, #40336, .F. ) ;
#11387 = CARTESIAN_POINT ( 'NONE',  ( 17.99999999999999645, -73.78980555658542073, -95.26571049922065981 ) ) ;
#11388 = CARTESIAN_POINT ( 'NONE',  ( 55.68207322487837274, 39.99999999999999289, -32.16283696846894458 ) ) ;
#11389 = CARTESIAN_POINT ( 'NONE',  ( 53.62204311759386854, 40.00000000000000000, -18.10832464707264577 ) ) ;
#11390 = ADVANCED_FACE ( 'NONE', ( #32781 ), #6375, .F. ) ;
#11391 = CIRCLE ( 'NONE', #26021, 1.000000000000000666 ) ;
#11392 = DIRECTION ( 'NONE',  ( 0.000000000000000000, -0.5963673585384915432, -0.8027116379309710004 ) ) ;
#11393 = DIRECTION ( 'NONE',  ( 0.000000000000000000, 0.000000000000000000, 1.000000000000000000 ) ) ;
#11394 = EDGE_CURVE ( 'NONE', #3798, #2973, #26041, .T. ) ;
#11395 = DIRECTION ( 'NONE',  ( 1.000000000000000000, -0.000000000000000000, -0.000000000000000000 ) ) ;
#11396 = DIRECTION ( 'NONE',  ( 0.000000000000000000, 0.000000000000000000, 1.000000000000000000 ) ) ;
#11397 = COLOUR_RGB ( '', 0.40784314, 0.44705882, 0.49803922) ;
#11398 = ORIENTED_EDGE ( 'NONE', *, *, #41983, .T. ) ;
#11399 = CARTESIAN_POINT ( 'NONE',  ( 28.66079171547214699, 40.00000000000000000, 21.97938003711830035 ) ) ;
#11400 = VERTEX_POINT ( 'NONE', #5944 ) ;
#11401 = CARTESIAN_POINT ( 'NONE',  ( -101.1532682021072134, 40.00000000000000000, -3.256983028635321187 ) ) ;
#11402 = MECHANICAL_DESIGN_GEOMETRIC_PRESENTATION_REPRESENTATION (  '', ( #40632 ), #5123 ) ;
#11403 = CARTESIAN_POINT ( 'NONE',  ( -0.5469614295416921346, 4.303013824936271270, -3.535263753543735454 ) ) ;
#11404 = ORIENTED_EDGE ( 'NONE', *, *, #19494, .F. ) ;
#11405 = ADVANCED_FACE ( 'NONE', ( #16229 ), #6583, .T. ) ;
#11406 = CARTESIAN_POINT ( 'NONE',  ( 17.99999999999999645, 110.3490479609632615, -20.28201389785435182 ) ) ;
#11407 = DIRECTION ( 'NONE',  ( -1.000000000000000000, 0.000000000000000000, -0.000000000000000000 ) ) ;
#11408 = EDGE_LOOP ( 'NONE', ( #33474, #38660, #29524, #28788 ) ) ;
#11409 = DIRECTION ( 'NONE',  ( 3.009274222672345096E-17, 1.000000000000000000, -2.455023325076454960E-18 ) ) ;
#11410 = EDGE_LOOP ( 'NONE', ( #33382, #2971, #21700, #29176 ) ) ;
#11411 = VERTEX_POINT ( 'NONE', #3070 ) ;
#11412 = CARTESIAN_POINT ( 'NONE',  ( 18.00000000000000355, 19.44205635905601781, -43.33776004284589334 ) ) ;
#11413 = EDGE_CURVE ( 'NONE', #22001, #719, #41948, .T. ) ;
#11414 = CARTESIAN_POINT ( 'NONE',  ( 19.52887458859586545, 31.00000000000000355, -72.48875405280207929 ) ) ;
#11415 = CIRCLE ( 'NONE', #205, 59.00000000000000000 ) ;
#11416 = VERTEX_POINT ( 'NONE', #14 ) ;
#11417 = LINE ( 'NONE', #8345, #32800 ) ;
#11418 = EDGE_CURVE ( 'NONE', #9595, #21320, #29315, .T. ) ;
#11419 = EDGE_CURVE ( 'NONE', #24522, #37184, #18314, .T. ) ;
#11420 = EDGE_CURVE ( 'NONE', #12532, #19198, #6813, .T. ) ;
#11421 = CARTESIAN_POINT ( 'NONE',  ( 0.000000000000000000, -5.919241748379815427, 31.39643714728454427 ) ) ;
#11422 = EDGE_LOOP ( 'NONE', ( #18439, #19575, #1869, #6958, #4533 ) ) ;
#11423 = DIRECTION ( 'NONE',  ( 3.009274222672345096E-17, 1.000000000000000000, -2.455023325076455345E-18 ) ) ;
#11424 = VERTEX_POINT ( 'NONE', #42381 ) ;
#11425 = AXIS2_PLACEMENT_3D ( 'NONE', #6113, #16175, #22736 ) ;
#11426 = CARTESIAN_POINT ( 'NONE',  ( 91.58570893733640617, 39.99999999999999289, -30.97307622143650718 ) ) ;
#11427 = CARTESIAN_POINT ( 'NONE',  ( -87.85203729262056527, 40.00000000000000711, 50.59313708112332364 ) ) ;
#11429 = DIRECTION ( 'NONE',  ( -1.000000000000000000, 0.000000000000000000, -0.000000000000000000 ) ) ;
#11428 = DIRECTION ( 'NONE',  ( 0.000000000000000000, 0.3612416661871471479, 0.9324722294043580328 ) ) ;
#11430 = CARTESIAN_POINT ( 'NONE',  ( 53.80287614962789178, -35.35525454449572180, 69.29271901957253021 ) ) ;
#11431 = LINE ( 'NONE', #11654, #36797 ) ;
#11432 = ORIENTED_EDGE ( 'NONE', *, *, #13360, .F. ) ;
#11433 = SURFACE_SIDE_STYLE ('',( #37593 ) ) ;
#11434 = CARTESIAN_POINT ( 'NONE',  ( 11.90854556226686789, -35.35525454449573601, -74.83297477053821467 ) ) ;
#11435 = CIRCLE ( 'NONE', #12830, 20.00000000000000711 ) ;
#11436 = ORIENTED_EDGE ( 'NONE', *, *, #35877, .T. ) ;
#11437 = DIRECTION ( 'NONE',  ( 0.000000000000000000, 0.000000000000000000, 1.000000000000000000 ) ) ;
#11438 = CARTESIAN_POINT ( 'NONE',  ( -100.0000000000000568, 31.00000000000000355, 2.687086664288074189E-12 ) ) ;
#11439 = CARTESIAN_POINT ( 'NONE',  ( 0.000000000000000000, 113.8630351447205697, 22.16324045874448601 ) ) ;
#11440 = ORIENTED_EDGE ( 'NONE', *, *, #12212, .F. ) ;
#11441 = AXIS2_PLACEMENT_3D ( 'NONE', #16459, #29762, #12330 ) ;
#11442 = CARTESIAN_POINT ( 'NONE',  ( -7.718844055051848230, 40.00000000000000000, -22.75659427661715384 ) ) ;
#11443 = ORIENTED_EDGE ( 'NONE', *, *, #27127, .F. ) ;
#11444 = VECTOR ( 'NONE', #7512, 1000.000000000000000 ) ;
#11445 = EDGE_LOOP ( 'NONE', ( #16588, #23974, #42539, #14232 ) ) ;
#11446 = CARTESIAN_POINT ( 'NONE',  ( 17.99999999999999645, 103.5682682299988500, -43.14958040911561454 ) ) ;
#11447 = DIRECTION ( 'NONE',  ( 0.000000000000000000, 0.9911528310040076395, -0.1327255272837190025 ) ) ;
#11448 = ADVANCED_FACE ( 'NONE', ( #37769 ), #463, .T. ) ;
#11449 = CARTESIAN_POINT ( 'NONE',  ( 18.00000000000000355, 41.20225022064636278, 23.63323037071415911 ) ) ;
#11450 = AXIS2_PLACEMENT_3D ( 'NONE', #20313, #3876, #10237 ) ;
#11451 = CARTESIAN_POINT ( 'NONE',  ( 8.999999999999998224, 108.8880088604276608, 39.99251838045997687 ) ) ;
#11452 = AXIS2_PLACEMENT_3D ( 'NONE', #7837, #41856, #11347 ) ;
#11453 = ORIENTED_EDGE ( 'NONE', *, *, #28624, .F. ) ;
#11454 = DIRECTION ( 'NONE',  ( 0.000000000000000000, 0.000000000000000000, -1.000000000000000000 ) ) ;
#11455 = ORIENTED_EDGE ( 'NONE', *, *, #8374, .T. ) ;
#11456 = CARTESIAN_POINT ( 'NONE',  ( 0.000000000000000000, 56.51398178981952469, -96.92493144647394843 ) ) ;
#11457 = DIRECTION ( 'NONE',  ( -1.000000000000000000, 0.000000000000000000, 0.000000000000000000 ) ) ;
#11458 = CARTESIAN_POINT ( 'NONE',  ( -8.920000000000003482, 0.000000000000000000, 14.99999999999999822 ) ) ;
#11459 = CARTESIAN_POINT ( 'NONE',  ( 0.000000000000000000, -97.89532456239460601, -54.81585448086294576 ) ) ;
#11460 = ORIENTED_EDGE ( 'NONE', *, *, #3396, .T. ) ;
#11461 = ORIENTED_EDGE ( 'NONE', *, *, #1299, .T. ) ;
#11462 = CARTESIAN_POINT ( 'NONE',  ( 0.000000000000000000, 0.000000000000000000, 0.000000000000000000 ) ) ;
#11463 = AXIS2_PLACEMENT_3D ( 'NONE', #34269, #37751, #31236 ) ;
#11464 = CARTESIAN_POINT ( 'NONE',  ( 3.413765605486547727, -14.29811891091961229, 0.000000000000000000 ) ) ;
#11465 = ADVANCED_BREP_SHAPE_REPRESENTATION ( '', ( #13444, #13552 ), #41322 ) ;
#11466 = VERTEX_POINT ( 'NONE', #17754 ) ;
#11468 = ORIENTED_EDGE ( 'NONE', *, *, #29294, .T. ) ;
#11467 = CYLINDRICAL_SURFACE ( 'NONE', #39639, 139.5000000000000000 ) ;
#11469 = CARTESIAN_POINT ( 'NONE',  ( -38.37160831357631707, 31.00000000000000355, -19.00137192356237392 ) ) ;
#11470 = DIRECTION ( 'NONE',  ( -1.000000000000000000, 0.000000000000000000, 0.000000000000000000 ) ) ;
#11471 = EDGE_CURVE ( 'NONE', #6492, #10188, #30608, .T. ) ;
#11472 = EDGE_CURVE ( 'NONE', #24485, #25931, #12033, .T. ) ;
#11473 = CLOSED_SHELL ( 'NONE', ( #38210, #14138, #42970, #2839, #3678, #12689, #40438, #387, #41407, #1200, #13973, #30064, #32588, #25581, #27848, #34654, #35018, #27652, #9768, #33082, #7896, #17774, #15634, #17603, #16218, #7029, #20470, #41346, #18710, #6619 ) ) ;
#11474 = CIRCLE ( 'NONE', #1666, 64.99999999999997158 ) ;
#11476 = DIRECTION ( 'NONE',  ( 0.000000000000000000, 0.6783118362696172188, -0.7347741508630661889 ) ) ;
#11475 = CARTESIAN_POINT ( 'NONE',  ( 17.99999999999999645, 0.6168405712491924486, -35.99471499692226217 ) ) ;
#11477 = EDGE_CURVE ( 'NONE', #31641, #18421, #27336, .T. ) ;
#11478 = ORIENTED_EDGE ( 'NONE', *, *, #22280, .F. ) ;
#11479 = DIRECTION ( 'NONE',  ( -1.000000000000000000, 0.000000000000000000, 0.000000000000000000 ) ) ;
#11480 = CARTESIAN_POINT ( 'NONE',  ( -58.36801134196149832, 40.00000000000000711, 19.71467013091580256 ) ) ;
#11481 = CIRCLE ( 'NONE', #7968, 20.00000000000000000 ) ;
#11482 = DIRECTION ( 'NONE',  ( 3.996523416598993920E-16, 2.658563593772947074E-15, 1.000000000000000000 ) ) ;
#11483 = CIRCLE ( 'NONE', #19838, 59.00000000000000000 ) ;
#11484 = DIRECTION ( 'NONE',  ( 0.000000000000000000, 1.000000000000000000, 0.000000000000000000 ) ) ;
#11485 = ORIENTED_EDGE ( 'NONE', *, *, #12039, .T. ) ;
#11486 = DIRECTION ( 'NONE',  ( -1.000000000000000000, 0.000000000000000000, 0.000000000000000000 ) ) ;
#11487 = ORIENTED_EDGE ( 'NONE', *, *, #40914, .T. ) ;
#11488 = AXIS2_PLACEMENT_3D ( 'NONE', #27022, #33337, #13934 ) ;
#11489 = DIRECTION ( 'NONE',  ( -1.000000000000000000, -0.000000000000000000, 0.000000000000000000 ) ) ;
#11490 = DIRECTION ( 'NONE',  ( 0.000000000000000000, 0.000000000000000000, -1.000000000000000000 ) ) ;
#11491 = ADVANCED_FACE ( 'NONE', ( #37341 ), #4168, .T. ) ;
#11492 = CARTESIAN_POINT ( 'NONE',  ( -65.92798595308768483, 31.00000000000000711, 22.39357416381200849 ) ) ;
#11493 = CARTESIAN_POINT ( 'NONE',  ( 0.000000000000000000, 46.87740477351718482, -3.172455868805370560 ) ) ;
#11494 = EDGE_LOOP ( 'NONE', ( #37141, #23866, #37773, #31073 ) ) ;
#11495 = AXIS2_PLACEMENT_3D ( 'NONE', #6204, #42834, #5987 ) ;
#11496 = CARTESIAN_POINT ( 'NONE',  ( 8.999999999999998224, -101.1403355683150096, 56.80345518653452785 ) ) ;
#11497 = ORIENTED_EDGE ( 'NONE', *, *, #12443, .T. ) ;
#11498 = CARTESIAN_POINT ( 'NONE',  ( 17.99999999999999645, 31.48608500567870294, 0.9019157472705636724 ) ) ;
#11499 = LINE ( 'NONE', #4719, #10878 ) ;
#11500 = CARTESIAN_POINT ( 'NONE',  ( -77.35014290652780744, 31.00000000000000711, 26.14598721591455543 ) ) ;
#11501 = CARTESIAN_POINT ( 'NONE',  ( -91.90012763196534706, 40.00000000000000711, 5.898218105444796855 ) ) ;
#11502 = DIRECTION ( 'NONE',  ( -1.000000000000000000, -0.000000000000000000, -0.000000000000000000 ) ) ;
#11503 = ADVANCED_FACE ( 'NONE', ( #33860 ), #14805, .F. ) ;
#11504 = ORIENTED_EDGE ( 'NONE', *, *, #12937, .T. ) ;
#11505 = CARTESIAN_POINT ( 'NONE',  ( 8.999999999999998224, 86.84764344323065188, -76.89919913989662348 ) ) ;
#11506 = ORIENTED_EDGE ( 'NONE', *, *, #30981, .T. ) ;
#11507 = CARTESIAN_POINT ( 'NONE',  ( 18.00000000000000355, -47.22458491092815791, -5.098390039074710778 ) ) ;
#11508 = AXIS2_PLACEMENT_3D ( 'NONE', #26254, #9436, #39530 ) ;
#11509 = CYLINDRICAL_SURFACE ( 'NONE', #5259, 2.649999999999979039 ) ;
#11510 = AXIS2_PLACEMENT_3D ( 'NONE', #42425, #32619, #5996 ) ;
#11512 = ORIENTED_EDGE ( 'NONE', *, *, #14083, .T. ) ;
#11511 = CYLINDRICAL_SURFACE ( 'NONE', #32526, 51.99999999999999289 ) ;
#11513 = DIRECTION ( 'NONE',  ( 1.000000000000000000, -0.000000000000000000, -0.000000000000000000 ) ) ;
#11514 = ORIENTED_EDGE ( 'NONE', *, *, #21258, .F. ) ;
#11515 = CARTESIAN_POINT ( 'NONE',  ( 0.000000000000000000, 11.46872990052381880, 45.56340405422447049 ) ) ;
#11516 = CIRCLE ( 'NONE', #26829, 2.500000000000000444 ) ;
#11517 = CARTESIAN_POINT ( 'NONE',  ( 72.43982367323130234, 39.99999999999999289, 63.53091779346544143 ) ) ;
#11518 = CARTESIAN_POINT ( 'NONE',  ( -6.599999999999997868, -19.59999999999999076, 2.400307726328811901E-15 ) ) ;
#11519 = ORIENTED_EDGE ( 'NONE', *, *, #4813, .T. ) ;
#11520 = DIRECTION ( 'NONE',  ( 0.000000000000000000, 0.000000000000000000, 1.000000000000000000 ) ) ;
#11521 = DIRECTION ( 'NONE',  ( -1.000000000000000000, -0.000000000000000000, -0.000000000000000000 ) ) ;
#11522 = EDGE_CURVE ( 'NONE', #2343, #25188, #26896, .T. ) ;
#11524 = DIRECTION ( 'NONE',  ( 0.000000000000000000, 0.000000000000000000, 1.000000000000000000 ) ) ;
#11523 = FACE_OUTER_BOUND ( 'NONE', #11688, .T. ) ;
#11525 = PRODUCT_RELATED_PRODUCT_CATEGORY ( 'part', '', ( #29412 ) ) ;
#11526 = ORIENTED_EDGE ( 'NONE', *, *, #37170, .F. ) ;
#11527 = DIRECTION ( 'NONE',  ( -1.000000000000000000, -0.000000000000000000, -0.000000000000000000 ) ) ;
#11528 = VERTEX_POINT ( 'NONE', #10738 ) ;
#11529 = DIRECTION ( 'NONE',  ( -3.009274222672345096E-17, -1.000000000000000000, 2.455023325076455345E-18 ) ) ;
#11530 = CARTESIAN_POINT ( 'NONE',  ( 34.63398384099732397, 40.00000000000000000, -11.69655689657770559 ) ) ;
#11531 = DIRECTION ( 'NONE',  ( 0.000000000000000000, 0.000000000000000000, 1.000000000000000000 ) ) ;
#11532 = EDGE_CURVE ( 'NONE', #1451, #4089, #14116, .T. ) ;
#11533 = DIRECTION ( 'NONE',  ( 0.000000000000000000, 0.000000000000000000, 1.000000000000000000 ) ) ;
#11534 = CIRCLE ( 'NONE', #10803, 11.00000000000023803 ) ;
#11535 = DIRECTION ( 'NONE',  ( -1.000000000000000000, -0.000000000000000000, -0.000000000000000000 ) ) ;
#11537 = ORIENTED_EDGE ( 'NONE', *, *, #28780, .T. ) ;
#11536 = AXIS2_PLACEMENT_3D ( 'NONE', #16093, #29392, #42662 ) ;
#11538 = CARTESIAN_POINT ( 'NONE',  ( 0.000000000000000000, 0.000000000000000000, 0.000000000000000000 ) ) ;
#11539 = ADVANCED_FACE ( 'NONE', ( #30387 ), #24075, .F. ) ;
#11540 = ORIENTED_EDGE ( 'NONE', *, *, #14435, .T. ) ;
#11541 = AXIS2_PLACEMENT_3D ( 'NONE', #13284, #26152, #29426 ) ;
#11542 = FACE_OUTER_BOUND ( 'NONE', #2689, .T. ) ;
#11543 = DIRECTION ( 'NONE',  ( -1.000000000000000000, -0.000000000000000000, 0.000000000000000000 ) ) ;
#11544 = EDGE_CURVE ( 'NONE', #27409, #30365, #37562, .T. ) ;
#11545 = CARTESIAN_POINT ( 'NONE',  ( 14.35450763783260797, 31.00000000000000355, -18.72194639494853874 ) ) ;
#11546 = ORIENTED_EDGE ( 'NONE', *, *, #23616, .F. ) ;
#11547 = CARTESIAN_POINT ( 'NONE',  ( 17.99999999999999645, -5.919241748379376666, -31.39643714728462953 ) ) ;
#11548 = CIRCLE ( 'NONE', #24810, 47.49900000000000233 ) ;
#11550 = AXIS2_PLACEMENT_3D ( 'NONE', #36475, #6593, #33230 ) ;
#11549 = CARTESIAN_POINT ( 'NONE',  ( 158.4999999999992042, -1.911776714485916438E-13, 9.999999999999937828 ) ) ;
#11551 = CARTESIAN_POINT ( 'NONE',  ( -5.399612364985466151, 31.00000000000000355, -82.39583333413678190 ) ) ;
#11552 = ORIENTED_EDGE ( 'NONE', *, *, #25694, .T. ) ;
#11553 = CARTESIAN_POINT ( 'NONE',  ( 42.13926417418816328, 31.00000000000000355, -36.83769365847010846 ) ) ;
#11554 = CARTESIAN_POINT ( 'NONE',  ( 29.96647033545507455, 40.00000000000000000, -88.27250603610892199 ) ) ;
#11555 = ORIENTED_EDGE ( 'NONE', *, *, #34321, .T. ) ;
#11556 = EDGE_CURVE ( 'NONE', #32995, #21160, #25943, .T. ) ;
#11557 = CIRCLE ( 'NONE', #10124, 58.99999999999999289 ) ;
#11558 = DIRECTION ( 'NONE',  ( 0.000000000000000000, 0.000000000000000000, 1.000000000000000000 ) ) ;
#11559 = CARTESIAN_POINT ( 'NONE',  ( -22.99999999999986855, -3.752293059970304436E-14, -25.99999999999999289 ) ) ;
#11560 = CYLINDRICAL_SURFACE ( 'NONE', #22708, 13.59999999999999787 ) ;
#11561 = CIRCLE ( 'NONE', #17149, 2.649999999999985700 ) ;
#11563 = ORIENTED_EDGE ( 'NONE', *, *, #588, .F. ) ;
#11562 = DIRECTION ( 'NONE',  ( -1.000000000000000000, 0.000000000000000000, -0.000000000000000000 ) ) ;
#11564 = CIRCLE ( 'NONE', #22728, 11.00000000000023448 ) ;
#11565 = LINE ( 'NONE', #24908, #38577 ) ;
#11566 = AXIS2_PLACEMENT_3D ( 'NONE', #1082, #14436, #31227 ) ;
#11567 = DIRECTION ( 'NONE',  ( -1.000000000000000000, -0.000000000000000000, -0.000000000000000000 ) ) ;
#11568 = AXIS2_PLACEMENT_3D ( 'NONE', #27768, #41027, #29628 ) ;
#11569 = VERTEX_POINT ( 'NONE', #27780 ) ;
#11570 = CARTESIAN_POINT ( 'NONE',  ( -54.58798567973315841, 40.00000000000000000, -26.90590473539369754 ) ) ;
#11571 = DIRECTION ( 'NONE',  ( -1.000000000000000000, 0.000000000000000000, 0.000000000000000000 ) ) ;
#11572 = VERTEX_POINT ( 'NONE', #33636 ) ;
#11573 = AXIS2_PLACEMENT_3D ( 'NONE', #32872, #41120, #14332 ) ;
#11574 = DIRECTION ( 'NONE',  ( 0.000000000000000000, 0.000000000000000000, 1.000000000000000000 ) ) ;
#11575 = FACE_BOUND ( 'NONE', #34503, .T. ) ;
#11576 = AXIS2_PLACEMENT_3D ( 'NONE', #32353, #42153, #16620 ) ;
#11577 = CIRCLE ( 'NONE', #35923, 13.59999999999999787 ) ;
#11578 = EDGE_LOOP ( 'NONE', ( #19413, #24882, #6596, #18060 ) ) ;
#11579 = CARTESIAN_POINT ( 'NONE',  ( 18.00000000000000355, -44.47301969247456555, 16.68249143361894582 ) ) ;
#11580 = VERTEX_POINT ( 'NONE', #14467 ) ;
#11581 = CARTESIAN_POINT ( 'NONE',  ( 17.99999999999999645, 103.4151313792870610, 61.85306461934443689 ) ) ;
#11582 = VERTEX_POINT ( 'NONE', #228 ) ;
#11583 = CARTESIAN_POINT ( 'NONE',  ( 0.000000000000000000, -115.5737863835461496, -9.934782381634859050 ) ) ;
#11584 = DIRECTION ( 'NONE',  ( 1.000000000000000000, 0.000000000000000000, 0.000000000000000000 ) ) ;
#11585 = ORIENTED_EDGE ( 'NONE', *, *, #31646, .F. ) ;
#11586 = DIRECTION ( 'NONE',  ( 0.000000000000000000, 1.541976423090494844E-15, 1.000000000000000000 ) ) ;
#11587 = DIRECTION ( 'NONE',  ( -1.000000000000000000, -0.000000000000000000, 0.000000000000000000 ) ) ;
#11588 = ORIENTED_EDGE ( 'NONE', *, *, #38643, .F. ) ;
#11589 = DIRECTION ( 'NONE',  ( 0.000000000000000000, 0.000000000000000000, 1.000000000000000000 ) ) ;
#11590 = EDGE_CURVE ( 'NONE', #41981, #7783, #3717, .T. ) ;
#11591 = CARTESIAN_POINT ( 'NONE',  ( -22.99999999999998224, -5.613287575611343012E-14, -40.00000000000000711 ) ) ;
#11593 = EDGE_LOOP ( 'NONE', ( #1773, #18094, #18896, #5340 ) ) ;
#11592 = VECTOR ( 'NONE', #42693, 1000.000000000000000 ) ;
#11594 = FACE_OUTER_BOUND ( 'NONE', #860, .T. ) ;
#11595 = EDGE_CURVE ( 'NONE', #39961, #39644, #16888, .T. ) ;
#11596 = AXIS2_PLACEMENT_3D ( 'NONE', #371, #33126, #7370 ) ;
#11597 = CYLINDRICAL_SURFACE ( 'NONE', #11011, 1.399999999999998579 ) ;
#11598 = AXIS2_PLACEMENT_3D ( 'NONE', #379, #6503, #19863 ) ;
#11599 = CIRCLE ( 'NONE', #40798, 59.00000000000001421 ) ;
#11600 = DIRECTION ( 'NONE',  ( 1.000000000000000000, -6.123233995736766036E-17, -6.123233995736764803E-17 ) ) ;
#11601 = DIRECTION ( 'NONE',  ( -1.000000000000000000, 0.000000000000000000, 0.000000000000000000 ) ) ;
#11602 = CARTESIAN_POINT ( 'NONE',  ( -3.108867721649295035, 31.00000000000000355, 47.60416666525765095 ) ) ;
#11603 = VERTEX_POINT ( 'NONE', #10522 ) ;
#11604 = AXIS2_PLACEMENT_3D ( 'NONE', #21925, #35177, #40222 ) ;
#11606 = CYLINDRICAL_SURFACE ( 'NONE', #431, 31.49899999999999878 ) ;
#11605 = CARTESIAN_POINT ( 'NONE',  ( 0.000000000000000000, 0.000000000000000000, 0.000000000000000000 ) ) ;
#11607 = EDGE_LOOP ( 'NONE', ( #42248, #784 ) ) ;
#11608 = AXIS2_PLACEMENT_3D ( 'NONE', #18997, #25319, #8692 ) ;
#11609 = CIRCLE ( 'NONE', #40114, 13.59999999999999964 ) ;
#11610 = CARTESIAN_POINT ( 'NONE',  ( 1.598609366639573350E-14, -1.063425437509180407E-13, -40.00000000000000000 ) ) ;
#11611 = CARTESIAN_POINT ( 'NONE',  ( -57.43240763726046794, 40.00000000000000000, -19.49446143887317717 ) ) ;
#11612 = CARTESIAN_POINT ( 'NONE',  ( 51.84393115708665079, 40.00000000000000000, 25.66707601012906537 ) ) ;
#11613 = CIRCLE ( 'NONE', #4605, 120.5010000000000190 ) ;
#11614 = ADVANCED_FACE ( 'NONE', ( #23856 ), #7230, .F. ) ;
#11615 = CARTESIAN_POINT ( 'NONE',  ( 17.99999999999999645, 28.62203781743003717, -14.19692359621465094 ) ) ;
#11616 = DIRECTION ( 'NONE',  ( 0.000000000000000000, 0.000000000000000000, 1.000000000000000000 ) ) ;
#11617 = EDGE_CURVE ( 'NONE', #10758, #976, #23865, .T. ) ;
#11618 = DIRECTION ( 'NONE',  ( -1.000000000000000000, -0.000000000000000000, -0.000000000000000000 ) ) ;
#11619 = CARTESIAN_POINT ( 'NONE',  ( 11.68784703496123711, 31.00000000000000355, -20.25319168173327355 ) ) ;
#11620 = EDGE_LOOP ( 'NONE', ( #37087, #5984, #5767, #12160 ) ) ;
#11621 = CARTESIAN_POINT ( 'NONE',  ( 14.71924655979513297, 40.00000000000000000, -29.87007926703815741 ) ) ;
#11622 = ORIENTED_EDGE ( 'NONE', *, *, #17913, .T. ) ;
#11623 = CYLINDRICAL_SURFACE ( 'NONE', #23665, 13.60000000000000142 ) ;
#11624 = CARTESIAN_POINT ( 'NONE',  ( 22.90854556226710415, -12.05525454449572997, -74.83297477053821467 ) ) ;
#11625 = ORIENTED_EDGE ( 'NONE', *, *, #11650, .T. ) ;
#11626 = CIRCLE ( 'NONE', #11661, 36.00000000000000000 ) ;
#11627 = CYLINDRICAL_SURFACE ( 'NONE', #38196, 47.49900000000000233 ) ;
#11628 = DIRECTION ( 'NONE',  ( -3.009274222672345096E-17, -1.000000000000000000, 2.455023325076454960E-18 ) ) ;
#11629 = ORIENTED_EDGE ( 'NONE', *, *, #2257, .F. ) ;
#11630 = CARTESIAN_POINT ( 'NONE',  ( 2.805705207896068476, -3.226868319750173075, -3.503898532754370354 ) ) ;
#11631 = AXIS2_PLACEMENT_3D ( 'NONE', #38195, #21672, #14888 ) ;
#11632 = EDGE_LOOP ( 'NONE', ( #37577, #23987, #23984, #8671 ) ) ;
#11633 = AXIS2_PLACEMENT_3D ( 'NONE', #8895, #15273, #28349 ) ;
#11634 = AXIS2_PLACEMENT_3D ( 'NONE', #12147, #15439, #15635 ) ;
#11635 = EDGE_CURVE ( 'NONE', #18706, #17459, #10601, .T. ) ;
#11636 = ORIENTED_EDGE ( 'NONE', *, *, #16623, .F. ) ;
#11637 = CARTESIAN_POINT ( 'NONE',  ( 18.00000000000000355, -3.840921266750155993, 47.34345070675168188 ) ) ;
#11638 = CARTESIAN_POINT ( 'NONE',  ( -4.660665814385270167, 31.00000000000000355, 69.59371722956201722 ) ) ;
#11639 = ORIENTED_EDGE ( 'NONE', *, *, #4580, .F. ) ;
#11640 = LINE ( 'NONE', #24538, #34206 ) ;
#11641 = AXIS2_PLACEMENT_3D ( 'NONE', #11084, #14355, #14580 ) ;
#11642 = CARTESIAN_POINT ( 'NONE',  ( 18.00000000000000355, 0.000000000000000000, 0.000000000000000000 ) ) ;
#11643 = ORIENTED_EDGE ( 'NONE', *, *, #38408, .F. ) ;
#11644 = CARTESIAN_POINT ( 'NONE',  ( 4.204015924366189871, -1.626724848190933548, -3.610627190413393084 ) ) ;
#11645 = EDGE_CURVE ( 'NONE', #38954, #20249, #6414, .T. ) ;
#11646 = VERTEX_POINT ( 'NONE', #27994 ) ;
#11647 = CARTESIAN_POINT ( 'NONE',  ( 59.96221986557397088, 40.00000000000000000, 78.35452998770438171 ) ) ;
#11648 = CIRCLE ( 'NONE', #24915, 58.99999999999999289 ) ;
#11649 = CARTESIAN_POINT ( 'NONE',  ( 25.13348990051749254, 31.00000000000000355, -8.510361017572021680 ) ) ;
#11650 = EDGE_CURVE ( 'NONE', #1507, #10739, #1337, .T. ) ;
#11652 = CYLINDRICAL_SURFACE ( 'NONE', #31885, 13.60000000000000142 ) ;
#11651 = DIRECTION ( 'NONE',  ( 0.000000000000000000, 0.6382441836448211614, -0.7698339834299053885 ) ) ;
#11653 = DIRECTION ( 'NONE',  ( 1.000000000000000000, 0.000000000000000000, 0.000000000000000000 ) ) ;
#11654 = CARTESIAN_POINT ( 'NONE',  ( 17.99999999999999645, -53.40478689619801145, 108.0204598100363711 ) ) ;
#11655 = VERTEX_POINT ( 'NONE', #15338 ) ;
#11656 = DIRECTION ( 'NONE',  ( 1.000000000000000000, 0.000000000000000000, 0.000000000000000000 ) ) ;
#11657 = EDGE_LOOP ( 'NONE', ( #21549, #10490, #26552, #13838 ) ) ;
#11658 = DIRECTION ( 'NONE',  ( 0.000000000000000000, -0.1590634960190789038, 0.9872683547213435551 ) ) ;
#11659 = CARTESIAN_POINT ( 'NONE',  ( -60.10374203099167545, 31.00000000000000711, 78.35501831527777483 ) ) ;
#11660 = DIRECTION ( 'NONE',  ( 0.000000000000000000, 0.9996456111234524045, 0.02662052143777834251 ) ) ;
#11661 = AXIS2_PLACEMENT_3D ( 'NONE', #34835, #24850, #40940 ) ;
#11662 = ORIENTED_EDGE ( 'NONE', *, *, #9934, .T. ) ;
#11663 = CIRCLE ( 'NONE', #17954, 11.00000000000000000 ) ;
#11664 = CARTESIAN_POINT ( 'NONE',  ( 16.96065435355295392, 40.00000000000000000, -19.31014141889295743 ) ) ;
#11665 = CIRCLE ( 'NONE', #5389, 120.5010000000000190 ) ;
#11666 = VECTOR ( 'NONE', #12253, 1000.000000000000000 ) ;
#11667 = ORIENTED_EDGE ( 'NONE', *, *, #22378, .T. ) ;
#11668 = CIRCLE ( 'NONE', #15842, 20.00000000000001066 ) ;
#11669 = ADVANCED_FACE ( 'NONE', ( #28201 ), #35364, .F. ) ;
#11670 = VERTEX_POINT ( 'NONE', #41698 ) ;
#11671 = DIRECTION ( 'NONE',  ( -0.000000000000000000, -0.000000000000000000, 1.000000000000000000 ) ) ;
#11672 = DIRECTION ( 'NONE',  ( -0.000000000000000000, -0.000000000000000000, 1.000000000000000000 ) ) ;
#11673 = EDGE_CURVE ( 'NONE', #30654, #17334, #38415, .T. ) ;
#11674 = CYLINDRICAL_SURFACE ( 'NONE', #1800, 47.49900000000000233 ) ;
#11675 = CIRCLE ( 'NONE', #22162, 47.49900000000000233 ) ;
#11676 = EDGE_CURVE ( 'NONE', #19109, #5383, #10635, .T. ) ;
#11677 = ADVANCED_FACE ( 'NONE', ( #15542 ), #12051, .F. ) ;
#11678 = FACE_OUTER_BOUND ( 'NONE', #41878, .T. ) ;
#11679 = AXIS2_PLACEMENT_3D ( 'NONE', #42993, #13148, #42764 ) ;
#11680 = EDGE_LOOP ( 'NONE', ( #39097, #16467 ) ) ;
#11681 = DIRECTION ( 'NONE',  ( 0.000000000000000000, -0.9407002666710297945, -0.3392388661180402165 ) ) ;
#11682 = EDGE_LOOP ( 'NONE', ( #35735, #2533, #41529, #15918 ) ) ;
#11683 = CARTESIAN_POINT ( 'NONE',  ( 18.00000000000000355, 42.60732521687572927, 19.80331771201673519 ) ) ;
#11684 = PLANE ( 'NONE',  #13759 ) ;
#11685 = VECTOR ( 'NONE', #24993, 1000.000000000000000 ) ;
#11686 = LINE ( 'NONE', #30872, #20092 ) ;
#11687 = CARTESIAN_POINT ( 'NONE',  ( 0.000000000000000000, 107.2885202478266251, 54.86040852957352598 ) ) ;
#11688 = EDGE_LOOP ( 'NONE', ( #22294, #5114, #36680, #28744 ) ) ;
#11689 = ORIENTED_EDGE ( 'NONE', *, *, #34406, .T. ) ;
#11690 = CARTESIAN_POINT ( 'NONE',  ( 0.000000000000000000, -78.18175027177375114, -85.69488855493077040 ) ) ;
#11691 = DIRECTION ( 'NONE',  ( -0.000000000000000000, -0.000000000000000000, 1.000000000000000000 ) ) ;
#11692 = ORIENTED_EDGE ( 'NONE', *, *, #10667, .T. ) ;
#11694 = ORIENTED_EDGE ( 'NONE', *, *, #13591, .F. ) ;
#11693 = CARTESIAN_POINT ( 'NONE',  ( 18.00000000000000355, -47.22458491092815791, -5.098390039074710778 ) ) ;
#11695 = CARTESIAN_POINT ( 'NONE',  ( -21.81649963859176822, 31.00000000000000355, -37.93159502954523532 ) ) ;
#11696 = ORIENTED_EDGE ( 'NONE', *, *, #11057, .F. ) ;
#11697 = CYLINDRICAL_SURFACE ( 'NONE', #5618, 120.5010000000000190 ) ;
#11698 = AXIS2_PLACEMENT_3D ( 'NONE', #12792, #26106, #13660 ) ;
#11699 = AXIS2_PLACEMENT_3D ( 'NONE', #37766, #3944, #11393 ) ;
#11700 = AXIS2_PLACEMENT_3D ( 'NONE', #14647, #41868, #12016 ) ;
#11702 = DIRECTION ( 'NONE',  ( 1.000000000000000000, 0.000000000000000000, -6.546126324440847704E-16 ) ) ;
#11701 = DIRECTION ( 'NONE',  ( 1.000000000000000000, 0.000000000000000000, 0.000000000000000000 ) ) ;
#11703 = EDGE_CURVE ( 'NONE', #23971, #36837, #39168, .T. ) ;
#11704 = ORIENTED_EDGE ( 'NONE', *, *, #6318, .F. ) ;
#11705 = CARTESIAN_POINT ( 'NONE',  ( 17.99999999999999645, 73.78980555658732499, -95.26571049921918188 ) ) ;
#11706 = CIRCLE ( 'NONE', #13785, 14.99999999999999822 ) ;
#11707 = CARTESIAN_POINT ( 'NONE',  ( 43.45541166192411708, 40.00000000000000000, -49.38773770141698805 ) ) ;
#11708 = CIRCLE ( 'NONE', #507, 59.00000000000000711 ) ;
#11709 = CIRCLE ( 'NONE', #16570, 36.00000000000000000 ) ;
#11710 = EDGE_CURVE ( 'NONE', #20287, #3093, #14146, .T. ) ;
#11711 = CIRCLE ( 'NONE', #13796, 20.00000000000000711 ) ;
#11712 = DIRECTION ( 'NONE',  ( -1.000000000000000000, 0.000000000000000000, -0.000000000000000000 ) ) ;
#11713 = DIRECTION ( 'NONE',  ( 0.000000000000000000, 0.000000000000000000, 1.000000000000000000 ) ) ;
#11714 = ORIENTED_EDGE ( 'NONE', *, *, #38569, .F. ) ;
#11715 = CARTESIAN_POINT ( 'NONE',  ( 22.90854556226730310, -35.35525454449573601, -74.83297477053802993 ) ) ;
#11716 = EDGE_LOOP ( 'NONE', ( #39707, #1165, #23073, #20775 ) ) ;
#11717 =( NAMED_UNIT ( * ) SI_UNIT ( $, .STERADIAN. ) SOLID_ANGLE_UNIT ( ) );
#11718 =( REPRESENTATION_RELATIONSHIP ('NONE','NONE', #330, #37437 ) REPRESENTATION_RELATIONSHIP_WITH_TRANSFORMATION ( #17912 )SHAPE_REPRESENTATION_RELATIONSHIP( ) );
#11719 = DIRECTION ( 'NONE',  ( 1.000000000000000000, 0.000000000000000000, 0.000000000000000000 ) ) ;
#11720 = DIRECTION ( 'NONE',  ( -1.000000000000000000, 0.000000000000000000, 0.000000000000000000 ) ) ;
#11721 = AXIS2_PLACEMENT_3D ( 'NONE', #29839, #6250, #19805 ) ;
#11722 = CARTESIAN_POINT ( 'NONE',  ( 28.01378275134445772, 31.00000000000000355, -56.83506808085938644 ) ) ;
#11723 = FACE_OUTER_BOUND ( 'NONE', #2793, .T. ) ;
#11724 = EDGE_LOOP ( 'NONE', ( #33178, #42800, #41619, #10631 ) ) ;
#11725 = LINE ( 'NONE', #18083, #30316 ) ;
#11726 = ORIENTED_EDGE ( 'NONE', *, *, #23093, .T. ) ;
#11727 = CARTESIAN_POINT ( 'NONE',  ( 17.99999999999999645, 0.04937522221168735848, -31.94951095880158576 ) ) ;
#11728 = DIRECTION ( 'NONE',  ( -1.000000000000000000, 0.000000000000000000, -0.000000000000000000 ) ) ;
#11729 = AXIS2_PLACEMENT_3D ( 'NONE', #30178, #39744, #3960 ) ;
#11730 = CARTESIAN_POINT ( 'NONE',  ( -49.21613380539480431, 31.00000000000000355, 63.96793098899347996 ) ) ;
#11731 = CARTESIAN_POINT ( 'NONE',  ( 76.16439905403352384, 39.99999999999999289, 44.11546174421767574 ) ) ;
#11732 = ADVANCED_FACE ( 'NONE', ( #12260 ), #36718, .F. ) ;
#11733 = EDGE_CURVE ( 'NONE', #6621, #39372, #9556, .T. ) ;
#11734 = DIRECTION ( 'NONE',  ( 0.000000000000000000, -0.7164567402983066380, -0.6976315211349934930 ) ) ;
#11735 = CIRCLE ( 'NONE', #20096, 120.5010000000000190 ) ;
#11736 = VECTOR ( 'NONE', #42631, 1000.000000000000000 ) ;
#11737 = ADVANCED_FACE ( 'NONE', ( #22471 ), #22911, .F. ) ;
#11738 = ORIENTED_EDGE ( 'NONE', *, *, #33064, .F. ) ;
#11739 = CARTESIAN_POINT ( 'NONE',  ( 18.00000000000000355, 0.000000000000000000, 0.000000000000000000 ) ) ;
#11740 = AXIS2_PLACEMENT_3D ( 'NONE', #4867, #14501, #21510 ) ;
#11741 = ORIENTED_EDGE ( 'NONE', *, *, #40550, .T. ) ;
#11742 = VECTOR ( 'NONE', #14523, 1000.000000000000000 ) ;
#11743 = DIRECTION ( 'NONE',  ( 0.000000000000000000, 0.000000000000000000, 1.000000000000000000 ) ) ;
#11744 = DIRECTION ( 'NONE',  ( 0.000000000000000000, 0.000000000000000000, 1.000000000000000000 ) ) ;
#11745 = CONICAL_SURFACE ( 'NONE', #20822, 4.000000000000000000, 0.8911886515913786111 ) ;
#11747 = VERTEX_POINT ( 'NONE', #22681 ) ;
#11746 = CARTESIAN_POINT ( 'NONE',  ( 18.00000000000000355, -17.50309955389580452, -43.60271849949383949 ) ) ;
#11748 = DIRECTION ( 'NONE',  ( 0.000000000000000000, 0.9574220383620042352, 0.2886919473396248881 ) ) ;
#11749 = ORIENTED_EDGE ( 'NONE', *, *, #30910, .F. ) ;
#11750 = CARTESIAN_POINT ( 'NONE',  ( 153.1500000000000057, 1.576403824487674918E-12, 9.999999999999998224 ) ) ;
#11751 = DIRECTION ( 'NONE',  ( 0.000000000000000000, 0.000000000000000000, 1.000000000000000000 ) ) ;
#11752 = EDGE_LOOP ( 'NONE', ( #19586, #28428, #18441, #664 ) ) ;
#11753 = EDGE_CURVE ( 'NONE', #2648, #36025, #12627, .T. ) ;
#11754 = DIRECTION ( 'NONE',  ( 0.000000000000000000, 0.000000000000000000, 1.000000000000000000 ) ) ;
#11755 = CARTESIAN_POINT ( 'NONE',  ( -30.61154013076161107, 31.00000000000001776, 25.77968906985393716 ) ) ;
#11756 = AXIS2_PLACEMENT_3D ( 'NONE', #2890, #6406, #43054 ) ;
#11758 = CARTESIAN_POINT ( 'NONE',  ( -0.2142857142857142738, -10.49781318335647917, -1.199999999999999956 ) ) ;
#11757 = LINE ( 'NONE', #25087, #4198 ) ;
#11759 = ORIENTED_EDGE ( 'NONE', *, *, #9218, .F. ) ;
#11760 = FACE_OUTER_BOUND ( 'NONE', #2563, .T. ) ;
#11761 = VERTEX_POINT ( 'NONE', #35713 ) ;
#11762 = CYLINDRICAL_SURFACE ( 'NONE', #23836, 15.99999999999999289 ) ;
#11763 = CARTESIAN_POINT ( 'NONE',  ( -28.46928290085317670, 40.00000000000000000, -16.49637127829624106 ) ) ;
#11764 = CARTESIAN_POINT ( 'NONE',  ( 0.000000000000000000, 35.72777019205808813, -106.3569410558013715 ) ) ;
#11765 = AXIS2_PLACEMENT_3D ( 'NONE', #2190, #22116, #39258 ) ;
#11766 = VECTOR ( 'NONE', #9571, 1000.000000000000000 ) ;
#11767 = DIRECTION ( 'NONE',  ( -1.000000000000000000, 0.000000000000000000, 0.000000000000000000 ) ) ;
#11768 = EDGE_CURVE ( 'NONE', #30521, #39546, #20414, .T. ) ;
#11769 = CARTESIAN_POINT ( 'NONE',  ( 17.99999999999999645, 111.9370513079669394, 44.61600100275212100 ) ) ;
#11770 = ORIENTED_EDGE ( 'NONE', *, *, #39650, .F. ) ;
#11771 = VECTOR ( 'NONE', #13075, 1000.000000000000000 ) ;
#11772 = CARTESIAN_POINT ( 'NONE',  ( 0.000000000000000000, -16.77566611177856615, 119.3275660838941832 ) ) ;
#11773 = ORIENTED_EDGE ( 'NONE', *, *, #28224, .T. ) ;
#11774 = AXIS2_PLACEMENT_3D ( 'NONE', #26018, #35795, #9414 ) ;
#11775 = AXIS2_PLACEMENT_3D ( 'NONE', #689, #3730, #31265 ) ;
#11776 = CARTESIAN_POINT ( 'NONE',  ( 17.99999999999999645, -92.25992191227442163, 77.51514567967366531 ) ) ;
#11777 = CARTESIAN_POINT ( 'NONE',  ( 0.000000000000000000, 53.40478689619728669, 108.0204598100367548 ) ) ;
#11778 = CARTESIAN_POINT ( 'NONE',  ( 2.781618486875130358, 31.00000000000000355, -42.60416666509636485 ) ) ;
#11779 = ORIENTED_EDGE ( 'NONE', *, *, #16441, .F. ) ;
#11780 = DIRECTION ( 'NONE',  ( 1.000000000000000000, 0.000000000000000000, 0.000000000000000000 ) ) ;
#11781 = DIRECTION ( 'NONE',  ( -1.000000000000000000, -0.000000000000000000, -0.000000000000000000 ) ) ;
#11782 = CARTESIAN_POINT ( 'NONE',  ( -62.77658523491555798, 31.00000000000000711, 48.16944601536268777 ) ) ;
#11783 = ORIENTED_EDGE ( 'NONE', *, *, #32018, .T. ) ;
#11784 = CARTESIAN_POINT ( 'NONE',  ( 53.62204311759385433, 31.00000000000000355, -18.10832464707264577 ) ) ;
#11785 = ADVANCED_FACE ( 'NONE', ( #13279 ), #35514, .T. ) ;
#11786 = CARTESIAN_POINT ( 'NONE',  ( 81.87674480462379734, 39.99999999999999289, -21.93767060400471891 ) ) ;
#11787 = ORIENTED_EDGE ( 'NONE', *, *, #34261, .T. ) ;
#11788 = FACE_OUTER_BOUND ( 'NONE', #25133, .T. ) ;
#11789 = CARTESIAN_POINT ( 'NONE',  ( 9.000000000000001776, -0.6819280456836842585, 115.9979955608738607 ) ) ;
#11790 = DIRECTION ( 'NONE',  ( 1.000000000000000000, 0.000000000000000000, 0.000000000000000000 ) ) ;
#11791 = AXIS2_PLACEMENT_3D ( 'NONE', #29482, #6978, #17056 ) ;
#11792 = AXIS2_PLACEMENT_3D ( 'NONE', #38323, #35050, #42648 ) ;
#11794 = VERTEX_POINT ( 'NONE', #5630 ) ;
#11793 = DIRECTION ( 'NONE',  ( -1.000000000000000000, -0.000000000000000000, -0.000000000000000000 ) ) ;
#11795 = DIRECTION ( 'NONE',  ( 1.000000000000000000, 0.000000000000000000, 0.000000000000000000 ) ) ;
#11796 = CARTESIAN_POINT ( 'NONE',  ( 0.000000000000000000, 0.000000000000000000, 0.000000000000000000 ) ) ;
#11797 = AXIS2_PLACEMENT_3D ( 'NONE', #11683, #24572, #11894 ) ;
#11798 = EDGE_CURVE ( 'NONE', #31610, #10863, #25970, .T. ) ;
#11799 = ORIENTED_EDGE ( 'NONE', *, *, #15106, .T. ) ;
#11800 = CARTESIAN_POINT ( 'NONE',  ( 48.10206620145878276, 40.00000000000000000, -42.20136231105875879 ) ) ;
#11801 = CARTESIAN_POINT ( 'NONE',  ( 18.00000000000000355, -19.44205635905570873, 43.33776004284602124 ) ) ;
#11802 = ORIENTED_EDGE ( 'NONE', *, *, #22373, .T. ) ;
#11803 = ADVANCED_FACE ( 'NONE', ( #15695 ), #19412, .F. ) ;
#11804 = DIRECTION ( 'NONE',  ( -1.000000000000000000, -0.000000000000000000, 0.000000000000000000 ) ) ;
#11805 = DIRECTION ( 'NONE',  ( 0.000000000000000000, 0.000000000000000000, 1.000000000000000000 ) ) ;
#11806 = EDGE_CURVE ( 'NONE', #23971, #27819, #10853, .T. ) ;
#11807 = LINE ( 'NONE', #25131, #20098 ) ;
#11808 = ORIENTED_EDGE ( 'NONE', *, *, #3636, .T. ) ;
#11809 = ORIENTED_EDGE ( 'NONE', *, *, #1790, .T. ) ;
#11810 = FACE_OUTER_BOUND ( 'NONE', #12945, .T. ) ;
#11811 = ORIENTED_EDGE ( 'NONE', *, *, #37501, .F. ) ;
#11812 = PLANE ( 'NONE',  #13273 ) ;
#11813 = LINE ( 'NONE', #5455, #40153 ) ;
#11814 = CYLINDRICAL_SURFACE ( 'NONE', #13561, 116.0000000000000000 ) ;
#11815 = FACE_OUTER_BOUND ( 'NONE', #13401, .T. ) ;
#11816 = ORIENTED_EDGE ( 'NONE', *, *, #8906, .F. ) ;
#11817 = CYLINDRICAL_SURFACE ( 'NONE', #41222, 31.49899999999999878 ) ;
#11818 = ADVANCED_FACE ( 'NONE', ( #10187 ), #23750, .F. ) ;
#11819 = FACE_OUTER_BOUND ( 'NONE', #20495, .T. ) ;
#11820 = CIRCLE ( 'NONE', #14593, 36.00000000000000000 ) ;
#11821 = ORIENTED_EDGE ( 'NONE', *, *, #28389, .F. ) ;
#11822 = AXIS2_PLACEMENT_3D ( 'NONE', #2929, #33056, #3147 ) ;
#11823 = CARTESIAN_POINT ( 'NONE',  ( -9.000000000000005329, 0.000000000000000000, 0.000000000000000000 ) ) ;
#11824 = CARTESIAN_POINT ( 'NONE',  ( 0.000000000000000000, 0.000000000000000000, 0.000000000000000000 ) ) ;
#11825 = CARTESIAN_POINT ( 'NONE',  ( -150.5000000000000284, 17.99999999999998934, 5.291301926514011517E-13 ) ) ;
#11826 = CARTESIAN_POINT ( 'NONE',  ( 17.99999999999999645, 0.000000000000000000, 0.000000000000000000 ) ) ;
#11827 = CARTESIAN_POINT ( 'NONE',  ( 34.77048308403384169, 31.00000000000000355, 30.48958026498159768 ) ) ;
#11828 = ORIENTED_EDGE ( 'NONE', *, *, #15925, .F. ) ;
#11830 = DIRECTION ( 'NONE',  ( 0.000000000000000000, 0.000000000000000000, 1.000000000000000000 ) ) ;
#11829 = CARTESIAN_POINT ( 'NONE',  ( -91.96080130434580724, -14.05525454449570866, 14.45886780445738218 ) ) ;
#11831 = ORIENTED_EDGE ( 'NONE', *, *, #41699, .T. ) ;
#11832 = CARTESIAN_POINT ( 'NONE',  ( -48.53848235557606472, 40.00000000000000000, -37.22912483484027035 ) ) ;
#11833 = EDGE_CURVE ( 'NONE', #24221, #3449, #23036, .T. ) ;
#11834 = AXIS2_PLACEMENT_3D ( 'NONE', #40973, #4536, #7388 ) ;
#11835 = LINE ( 'NONE', #25161, #15171 ) ;
#11836 = CARTESIAN_POINT ( 'NONE',  ( 17.99999999999999645, 98.69720329641039314, -60.94966826379810243 ) ) ;
#11837 = DIRECTION ( 'NONE',  ( 0.000000000000000000, 0.000000000000000000, -1.000000000000000000 ) ) ;
#11838 = CARTESIAN_POINT ( 'NONE',  ( -20.07939870814534089, 31.00000000000000355, -2.638545259751242877 ) ) ;
#11839 = ADVANCED_FACE ( 'NONE', ( #36575 ), #30068, .F. ) ;
#11840 = ORIENTED_EDGE ( 'NONE', *, *, #25464, .F. ) ;
#11841 = CARTESIAN_POINT ( 'NONE',  ( 32.11716166826300167, 40.00000000000000000, 15.82712457579038912 ) ) ;
#11842 = ORIENTED_EDGE ( 'NONE', *, *, #36697, .T. ) ;
#11843 = DIRECTION ( 'NONE',  ( -1.000000000000000000, 0.000000000000000000, -0.000000000000000000 ) ) ;
#11845 = CARTESIAN_POINT ( 'NONE',  ( 0.1404048886732821022, 4.699864953788070565, -3.686887068327037387 ) ) ;
#11844 = VECTOR ( 'NONE', #9530, 1000.000000000000000 ) ;
#11846 = ORIENTED_EDGE ( 'NONE', *, *, #34446, .T. ) ;
#11847 = ADVANCED_FACE ( 'NONE', ( #40492 ), #10629, .T. ) ;
#11848 = CIRCLE ( 'NONE', #26435, 47.49900000000000233 ) ;
#11849 = DIRECTION ( 'NONE',  ( -1.000000000000000000, 0.000000000000000000, 0.000000000000000000 ) ) ;
#11850 = CARTESIAN_POINT ( 'NONE',  ( 17.99999999999999645, -84.77518783075143460, 73.49448960231327987 ) ) ;
#11851 = EDGE_CURVE ( 'NONE', #30436, #12372, #27189, .T. ) ;
#11852 = EDGE_LOOP ( 'NONE', ( #16035, #41873 ) ) ;
#11853 = DIRECTION ( 'NONE',  ( -1.000000000000000000, -0.000000000000000000, -0.000000000000000000 ) ) ;
#11854 = EDGE_LOOP ( 'NONE', ( #18635, #37168, #20247, #25269 ) ) ;
#11855 = CIRCLE ( 'NONE', #25777, 116.0000000000000000 ) ;
#11856 = ORIENTED_EDGE ( 'NONE', *, *, #5368, .F. ) ;
#11857 = DIRECTION ( 'NONE',  ( 0.000000000000000000, 0.000000000000000000, 1.000000000000000000 ) ) ;
#11858 = CARTESIAN_POINT ( 'NONE',  ( 5.085823974618866039, 31.00000000000000355, 79.40009828669005287 ) ) ;
#11859 = ORIENTED_EDGE ( 'NONE', *, *, #5517, .T. ) ;
#11860 = DIRECTION ( 'NONE',  ( 1.000000000000000000, 0.000000000000000000, 0.000000000000000000 ) ) ;
#11861 = DIRECTION ( 'NONE',  ( 1.000000000000000000, 0.000000000000000000, 0.000000000000000000 ) ) ;
#11862 = ORIENTED_EDGE ( 'NONE', *, *, #10317, .F. ) ;
#11863 = CARTESIAN_POINT ( 'NONE',  ( 4.197393957002303999, 7.772902908466098641E-14, -3.503767560748929810 ) ) ;
#11864 = CARTESIAN_POINT ( 'NONE',  ( 0.000000000000000000, -1.178949249685214307, 2.042000000000001592 ) ) ;
#11865 = EDGE_CURVE ( 'NONE', #12185, #15011, #12553, .T. ) ;
#11866 = CARTESIAN_POINT ( 'NONE',  ( 25.73918080462996372, 31.00000000000000355, -6.871072672212910959 ) ) ;
#11867 = EDGE_CURVE ( 'NONE', #35377, #5501, #26494, .T. ) ;
#11869 = DIRECTION ( 'NONE',  ( -1.000000000000000000, 0.000000000000000000, 0.000000000000000000 ) ) ;
#11868 = CARTESIAN_POINT ( 'NONE',  ( 17.99999999999999645, -2.418575551221673336, 120.4767259403368911 ) ) ;
#11870 = DIRECTION ( 'NONE',  ( -1.000000000000000000, -0.000000000000000000, -0.000000000000000000 ) ) ;
#11871 = CARTESIAN_POINT ( 'NONE',  ( 18.00000000000000355, -39.78933988720098114, -24.98727647985043276 ) ) ;
#11872 = EDGE_LOOP ( 'NONE', ( #6710, #26684, #9258, #13730 ) ) ;
#11873 = SURFACE_STYLE_FILL_AREA ( #42363 ) ;
#11874 = CARTESIAN_POINT ( 'NONE',  ( 0.000000000000000000, -31.81777574834303124, -2.898764365605651427 ) ) ;
#11875 = AXIS2_PLACEMENT_3D ( 'NONE', #41817, #8014, #21811 ) ;
#11876 = ORIENTED_EDGE ( 'NONE', *, *, #35610, .F. ) ;
#11877 = DIRECTION ( 'NONE',  ( 1.000000000000000000, 0.000000000000000000, -0.000000000000000000 ) ) ;
#11878 = CIRCLE ( 'NONE', #23717, 47.49900000000000233 ) ;
#11879 = CARTESIAN_POINT ( 'NONE',  ( -12.78314611188302052, 31.00000000000000355, 97.07982689498881257 ) ) ;
#11880 = FACE_OUTER_BOUND ( 'NONE', #26772, .T. ) ;
#11881 = ORIENTED_EDGE ( 'NONE', *, *, #8408, .F. ) ;
#11882 = CARTESIAN_POINT ( 'NONE',  ( 24.14050371820133023, 40.00000000000000000, 13.97356841391088444 ) ) ;
#11883 = ORIENTED_EDGE ( 'NONE', *, *, #20974, .F. ) ;
#11884 = EDGE_LOOP ( 'NONE', ( #10486, #41054, #2042, #11111 ) ) ;
#11885 = DIRECTION ( 'NONE',  ( 0.000000000000000000, 0.000000000000000000, 1.000000000000000000 ) ) ;
#11886 = CARTESIAN_POINT ( 'NONE',  ( -6.075999999999997847, 0.000000000000000000, 0.000000000000000000 ) ) ;
#11887 = DIRECTION ( 'NONE',  ( 0.000000000000000000, 0.000000000000000000, 1.000000000000000000 ) ) ;
#11888 = DIRECTION ( 'NONE',  ( 1.000000000000000000, -1.373900992973642263E-15, -3.996523416598957436E-16 ) ) ;
#11889 = EDGE_CURVE ( 'NONE', #21485, #27034, #4162, .T. ) ;
#11890 = CARTESIAN_POINT ( 'NONE',  ( 0.000000000000000000, -101.8011932243951634, 55.61040422519296555 ) ) ;
#11891 = ORIENTED_EDGE ( 'NONE', *, *, #3941, .F. ) ;
#11892 = CARTESIAN_POINT ( 'NONE',  ( 1.600000000000000089, -12.75000000000000000, -1.199999999999999956 ) ) ;
#11893 = ORIENTED_EDGE ( 'NONE', *, *, #16787, .T. ) ;
#11894 = DIRECTION ( 'NONE',  ( 0.000000000000000000, 0.7705132427757903635, -0.6374239897486881912 ) ) ;
#11895 = LINE ( 'NONE', #28264, #23513 ) ;
#11896 = CIRCLE ( 'NONE', #7690, 130.0000000000000000 ) ;
#11897 = EDGE_CURVE ( 'NONE', #15350, #23668, #11878, .T. ) ;
#11898 = CARTESIAN_POINT ( 'NONE',  ( 17.99999999999999645, 84.09610293794170843, -74.27057253242929846 ) ) ;
#11899 = DIRECTION ( 'NONE',  ( -1.000000000000000000, 0.000000000000000000, 0.000000000000000000 ) ) ;
#11900 = ORIENTED_EDGE ( 'NONE', *, *, #28593, .T. ) ;
#11901 = ORIENTED_EDGE ( 'NONE', *, *, #1846, .T. ) ;
#11902 = CARTESIAN_POINT ( 'NONE',  ( 17.99999999999999645, -117.9424311864587480, -24.69967462999156638 ) ) ;
#11903 = AXIS2_PLACEMENT_3D ( 'NONE', #6253, #28771, #42249 ) ;
#11904 = CARTESIAN_POINT ( 'NONE',  ( 0.000000000000000000, 5.822172717930716779, -31.41458249383134671 ) ) ;
#11905 = CIRCLE ( 'NONE', #11875, 52.00000000000000000 ) ;
#11906 = ORIENTED_EDGE ( 'NONE', *, *, #2285, .T. ) ;
#11908 = ORIENTED_EDGE ( 'NONE', *, *, #8214, .F. ) ;
#11907 = CARTESIAN_POINT ( 'NONE',  ( 0.000000000000000000, -108.8684555192048435, 27.12806418649580564 ) ) ;
#11909 = AXIS2_PLACEMENT_3D ( 'NONE', #38279, #38484, #14760 ) ;
#11910 = CARTESIAN_POINT ( 'NONE',  ( 56.43498182460272972, 31.00000000000000355, -7.339809665447901921 ) ) ;
#11912 = ORIENTED_EDGE ( 'NONE', *, *, #35671, .T. ) ;
#11911 = AXIS2_PLACEMENT_3D ( 'NONE', #4133, #34466, #21651 ) ;
#11913 = DIRECTION ( 'NONE',  ( -1.000000000000000000, -0.000000000000000000, -0.000000000000000000 ) ) ;
#11914 = AXIS2_PLACEMENT_3D ( 'NONE', #5685, #29265, #43179 ) ;
#11916 = CARTESIAN_POINT ( 'NONE',  ( 17.99999999999999645, -26.29521155129861398, 17.34211205339337880 ) ) ;
#11915 = CARTESIAN_POINT ( 'NONE',  ( 0.000000000000000000, 0.000000000000000000, 0.000000000000000000 ) ) ;
#11917 = VERTEX_POINT ( 'NONE', #14139 ) ;
#11918 = CARTESIAN_POINT ( 'NONE',  ( -56.48168293059611500, 40.00000000000000711, 43.19841958066528065 ) ) ;
#11919 = EDGE_CURVE ( 'NONE', #39753, #34203, #28603, .T. ) ;
#11920 = EDGE_CURVE ( 'NONE', #23147, #33779, #8362, .T. ) ;
#11921 = DIRECTION ( 'NONE',  ( -1.000000000000000000, 0.000000000000000000, -0.000000000000000000 ) ) ;
#11922 = EDGE_CURVE ( 'NONE', #17636, #16359, #7566, .T. ) ;
#11923 = ADVANCED_FACE ( 'NONE', ( #20924 ), #34179, .T. ) ;
#11924 = CIRCLE ( 'NONE', #41846, 58.99999999999999289 ) ;
#11925 = DIRECTION ( 'NONE',  ( 0.000000000000000000, -0.2631025642275284238, 0.9647678688145140402 ) ) ;
#11926 = EDGE_LOOP ( 'NONE', ( #7933, #17011, #36278, #5441 ) ) ;
#11927 = CARTESIAN_POINT ( 'NONE',  ( 8.999999999999998224, 29.09613215194482549, 21.19941258140333673 ) ) ;
#11928 = ORIENTED_EDGE ( 'NONE', *, *, #27934, .F. ) ;
#11929 = CARTESIAN_POINT ( 'NONE',  ( 0.000000000000000000, 0.000000000000000000, 0.000000000000000000 ) ) ;
#11930 = CYLINDRICAL_SURFACE ( 'NONE', #16466, 15.00000000000000000 ) ;
#11931 = CIRCLE ( 'NONE', #37676, 13.59999999999999964 ) ;
#11932 = CARTESIAN_POINT ( 'NONE',  ( -30.22953878324074495, 31.00000000000000355, 61.32923288305941867 ) ) ;
#11933 = CARTESIAN_POINT ( 'NONE',  ( 18.00000000000000355, 29.60891106212838508, -37.14118181634735549 ) ) ;
#11934 = VERTEX_POINT ( 'NONE', #23316 ) ;
#11935 = CIRCLE ( 'NONE', #27970, 59.00000000000000000 ) ;
#11936 = SURFACE_SIDE_STYLE ('',( #28083 ) ) ;
#11937 = VECTOR ( 'NONE', #36487, 1000.000000000000000 ) ;
#11938 = VERTEX_POINT ( 'NONE', #37227 ) ;
#11939 = CARTESIAN_POINT ( 'NONE',  ( 1.798435537469519230E-14, -1.196353617197826191E-13, -44.99999999999999289 ) ) ;
#11940 = CARTESIAN_POINT ( 'NONE',  ( 8.999999999999998224, 90.81729652456166946, 72.16798910853647442 ) ) ;
#11941 = CARTESIAN_POINT ( 'NONE',  ( -50.81742119984753714, 31.00000000000000355, -66.42451308377114572 ) ) ;
#11942 = CARTESIAN_POINT ( 'NONE',  ( 69.92891852059224789, 39.99999999999999289, 53.79372986807582180 ) ) ;
#11943 = VECTOR ( 'NONE', #2974, 1000.000000000000000 ) ;
#11944 = FACE_OUTER_BOUND ( 'NONE', #7463, .T. ) ;
#11945 = ADVANCED_FACE ( 'NONE', ( #33532 ), #4056, .T. ) ;
#11946 = ORIENTED_EDGE ( 'NONE', *, *, #26763, .F. ) ;
#11947 = FACE_OUTER_BOUND ( 'NONE', #11445, .T. ) ;
#11948 = EDGE_LOOP ( 'NONE', ( #40754, #4587, #4342, #15142 ) ) ;
#11949 = CIRCLE ( 'NONE', #3542, 59.00000000000000711 ) ;
#11950 = CARTESIAN_POINT ( 'NONE',  ( -6.999999999999995559, -19.59999999999999076, 2.424800662311759010E-15 ) ) ;
#11951 = CARTESIAN_POINT ( 'NONE',  ( 17.99999999999999645, 0.000000000000000000, 0.000000000000000000 ) ) ;
#11952 = ADVANCED_FACE ( 'NONE', ( #343 ), #13706, .F. ) ;
#11954 = EDGE_LOOP ( 'NONE', ( #4744, #35261, #24919, #29226 ) ) ;
#11953 = DIRECTION ( 'NONE',  ( 1.000000000000000000, 0.000000000000000000, -0.000000000000000000 ) ) ;
#11955 = CARTESIAN_POINT ( 'NONE',  ( 17.99999999999999645, 0.000000000000000000, 0.000000000000000000 ) ) ;
#11956 = ORIENTED_EDGE ( 'NONE', *, *, #34742, .T. ) ;
#11957 = CARTESIAN_POINT ( 'NONE',  ( 17.99999999999999645, 80.02407177072956301, 78.64108602299977235 ) ) ;
#11958 = DIRECTION ( 'NONE',  ( 1.000000000000000000, 0.000000000000000000, 0.000000000000000000 ) ) ;
#11959 = CARTESIAN_POINT ( 'NONE',  ( 21.00000000000000355, 0.000000000000000000, 0.000000000000000000 ) ) ;
#11960 = ORIENTED_EDGE ( 'NONE', *, *, #8473, .T. ) ;
#11961 = DIRECTION ( 'NONE',  ( 1.000000000000000000, 0.000000000000000000, 0.000000000000000000 ) ) ;
#11962 = CARTESIAN_POINT ( 'NONE',  ( 17.99999999999999645, 0.000000000000000000, 0.000000000000000000 ) ) ;
#11963 = CIRCLE ( 'NONE', #9808, 130.0000000000000000 ) ;
#11965 = DIRECTION ( 'NONE',  ( 1.000000000000000000, 0.000000000000000000, 0.000000000000000000 ) ) ;
#11964 = CARTESIAN_POINT ( 'NONE',  ( 17.99999999999999645, -18.35539002514457252, 110.6858262410709273 ) ) ;
#11966 = EDGE_LOOP ( 'NONE', ( #22564, #4437, #36860, #11357 ) ) ;
#11967 = DIRECTION ( 'NONE',  ( 0.000000000000000000, 0.000000000000000000, 1.000000000000000000 ) ) ;
#11969 = ORIENTED_EDGE ( 'NONE', *, *, #5494, .F. ) ;
#11968 = AXIS2_PLACEMENT_3D ( 'NONE', #11915, #25241, #22185 ) ;
#11970 = CARTESIAN_POINT ( 'NONE',  ( -10.00000000000000000, 0.000000000000000000, 0.000000000000000000 ) ) ;
#11971 = CARTESIAN_POINT ( 'NONE',  ( -3.925388345520635536, 40.00000000000000000, 29.51202942214662173 ) ) ;
#11972 = DIRECTION ( 'NONE',  ( 1.000000000000000000, 0.000000000000000000, 0.000000000000000000 ) ) ;
#11973 = AXIS2_PLACEMENT_3D ( 'NONE', #25811, #2628, #26007 ) ;
#11974 = EDGE_CURVE ( 'NONE', #36528, #15552, #34833, .T. ) ;
#11975 = ADVANCED_FACE ( 'NONE', ( #34609 ), #4723, .T. ) ;
#11976 = CARTESIAN_POINT ( 'NONE',  ( 17.99999999999999645, 0.000000000000000000, 0.000000000000000000 ) ) ;
#11977 = EDGE_CURVE ( 'NONE', #35437, #6343, #16046, .T. ) ;
#11978 = EDGE_CURVE ( 'NONE', #4308, #14223, #28316, .T. ) ;
#11979 = CIRCLE ( 'NONE', #19638, 20.00000000000000711 ) ;
#11980 = DIRECTION ( 'NONE',  ( -1.000000000000000000, 0.000000000000000000, -0.000000000000000000 ) ) ;
#11981 = ORIENTED_EDGE ( 'NONE', *, *, #23649, .T. ) ;
#11982 = DIRECTION ( 'NONE',  ( 0.000000000000000000, 0.000000000000000000, 1.000000000000000000 ) ) ;
#11983 = ADVANCED_FACE ( 'NONE', ( #11944 ), #34386, .T. ) ;
#11984 = ORIENTED_EDGE ( 'NONE', *, *, #30603, .F. ) ;
#11985 = CIRCLE ( 'NONE', #41898, 47.49900000000001654 ) ;
#11986 = DIRECTION ( 'NONE',  ( -1.000000000000000000, 0.000000000000000000, -0.000000000000000000 ) ) ;
#11987 = CARTESIAN_POINT ( 'NONE',  ( 0.000000000000000000, -119.8996782608629275, -12.02323392193478746 ) ) ;
#11988 = CARTESIAN_POINT ( 'NONE',  ( -10.91816144241376563, 31.00000000000000355, -40.73603723627661566 ) ) ;
#11989 = ORIENTED_EDGE ( 'NONE', *, *, #34297, .T. ) ;
#11990 = SURFACE_STYLE_FILL_AREA ( #6258 ) ;
#11991 = EDGE_CURVE ( 'NONE', #23414, #9794, #17466, .T. ) ;
#11992 = DIRECTION ( 'NONE',  ( -3.009274222672345096E-17, -1.000000000000000000, 2.455023325076454960E-18 ) ) ;
#11993 = CARTESIAN_POINT ( 'NONE',  ( 21.49215960483416410, 31.00000000000000355, -80.26604385357094884 ) ) ;
#11994 = ORIENTED_EDGE ( 'NONE', *, *, #6365, .F. ) ;
#11995 = CARTESIAN_POINT ( 'NONE',  ( 27.80911911935152503, 31.00000000000000355, -47.97225535896787108 ) ) ;
#11996 = CARTESIAN_POINT ( 'NONE',  ( 43.43872713698582544, 40.00000000000000000, 75.20828420317944563 ) ) ;
#11997 = ORIENTED_EDGE ( 'NONE', *, *, #39060, .F. ) ;
#11998 = AXIS2_PLACEMENT_3D ( 'NONE', #15563, #5709, #19489 ) ;
#11999 = FACE_BOUND ( 'NONE', #2326, .T. ) ;
#12000 = AXIS2_PLACEMENT_3D ( 'NONE', #10156, #37200, #17181 ) ;
#12001 = LINE ( 'NONE', #11789, #12444 ) ;
#12002 = FACE_OUTER_BOUND ( 'NONE', #35703, .T. ) ;
#12003 = CIRCLE ( 'NONE', #8483, 47.49899999999999523 ) ;
#12005 = VERTEX_POINT ( 'NONE', #38097 ) ;
#12004 = CARTESIAN_POINT ( 'NONE',  ( 0.000000000000000000, 0.000000000000000000, 0.000000000000000000 ) ) ;
#12006 = FACE_OUTER_BOUND ( 'NONE', #7257, .T. ) ;
#12008 = ADVANCED_FACE ( 'NONE', ( #18299 ), #1438, .T. ) ;
#12007 = DIRECTION ( 'NONE',  ( -1.000000000000000000, 0.000000000000000000, 0.000000000000000000 ) ) ;
#12009 = ORIENTED_EDGE ( 'NONE', *, *, #30013, .T. ) ;
#12010 = CARTESIAN_POINT ( 'NONE',  ( -69.34045338167970840, 40.00000000000000711, 9.142281554609933636 ) ) ;
#12011 = DIRECTION ( 'NONE',  ( -0.000000000000000000, -0.000000000000000000, 1.000000000000000000 ) ) ;
#12012 = AXIS2_PLACEMENT_3D ( 'NONE', #19069, #16418, #2411 ) ;
#12013 = VERTEX_POINT ( 'NONE', #41137 ) ;
#12014 = DIRECTION ( 'NONE',  ( -1.000000000000000000, 0.000000000000000000, 0.000000000000000000 ) ) ;
#12015 = CARTESIAN_POINT ( 'NONE',  ( -31.37281731866679024, 17.11489954122029289, 27.62913683693880174 ) ) ;
#12016 = DIRECTION ( 'NONE',  ( 0.000000000000000000, 0.5076658003388352380, 0.8615540813938089570 ) ) ;
#12017 = ORIENTED_EDGE ( 'NONE', *, *, #11806, .F. ) ;
#12018 = ORIENTED_EDGE ( 'NONE', *, *, #30914, .F. ) ;
#12019 = DIRECTION ( 'NONE',  ( 0.000000000000000000, 0.000000000000000000, 1.000000000000000000 ) ) ;
#12020 = ORIENTED_EDGE ( 'NONE', *, *, #6752, .F. ) ;
#12021 = DIRECTION ( 'NONE',  ( -1.000000000000000000, 0.000000000000000000, -0.000000000000000000 ) ) ;
#12022 = DIRECTION ( 'NONE',  ( -1.000000000000000000, -0.000000000000000000, 0.000000000000000000 ) ) ;
#12023 = CARTESIAN_POINT ( 'NONE',  ( 0.000000000000000000, 31.80866420683990725, 2.997093558041416195 ) ) ;
#12024 = ADVANCED_FACE ( 'NONE', ( #8633 ), #31352, .F. ) ;
#12025 = ADVANCED_FACE ( 'NONE', ( #1653 ), #31996, .T. ) ;
#12026 = CARTESIAN_POINT ( 'NONE',  ( 126.0000000000000284, -2.077321393419931030E-13, 2.000000000000050626 ) ) ;
#12027 = ORIENTED_EDGE ( 'NONE', *, *, #72, .T. ) ;
#12028 = LINE ( 'NONE', #35964, #34907 ) ;
#12029 = UNCERTAINTY_MEASURE_WITH_UNIT (LENGTH_MEASURE( 1.000000000000000082E-05 ), #3755, 'distance_accuracy_value', 'NONE');
#12030 = EDGE_CURVE ( 'NONE', #27228, #41800, #41582, .T. ) ;
#12031 = AXIS2_PLACEMENT_3D ( 'NONE', #10662, #24003, #39878 ) ;
#12032 = VECTOR ( 'NONE', #14439, 1000.000000000000000 ) ;
#12033 = CIRCLE ( 'NONE', #15521, 58.99999999999999289 ) ;
#12034 = FACE_OUTER_BOUND ( 'NONE', #23989, .T. ) ;
#12035 = ORIENTED_EDGE ( 'NONE', *, *, #10290, .F. ) ;
#12036 = DIRECTION ( 'NONE',  ( -1.000000000000000000, -0.000000000000000000, 0.000000000000000000 ) ) ;
#12037 = AXIS2_PLACEMENT_3D ( 'NONE', #41655, #11804, #38377 ) ;
#12038 = CARTESIAN_POINT ( 'NONE',  ( -6.259644161404860030E-16, -4.618802153517027165, -5.000000000000000000 ) ) ;
#12039 = EDGE_CURVE ( 'NONE', #19203, #31163, #38315, .T. ) ;
#12040 = APPLICATION_PROTOCOL_DEFINITION ( 'draft international standard', 'automotive_design', 1998, #40910 ) ;
#12041 = DIRECTION ( 'NONE',  ( -1.000000000000000000, 0.000000000000000000, -0.000000000000000000 ) ) ;
#12042 = CARTESIAN_POINT ( 'NONE',  ( 36.61186797162192619, 31.00000000000000355, 28.07927795628900469 ) ) ;
#12043 = AXIS2_PLACEMENT_3D ( 'NONE', #29249, #15732, #38825 ) ;
#12044 = ORIENTED_EDGE ( 'NONE', *, *, #33329, .F. ) ;
#12045 = CARTESIAN_POINT ( 'NONE',  ( 17.99999999999999645, 0.000000000000000000, 0.000000000000000000 ) ) ;
#12046 = EDGE_CURVE ( 'NONE', #4304, #22351, #30673, .T. ) ;
#12047 = ORIENTED_EDGE ( 'NONE', *, *, #38337, .F. ) ;
#12048 = CARTESIAN_POINT ( 'NONE',  ( -53.27196957865878346, 40.00000000000000711, 26.27224001323269320 ) ) ;
#12049 = CARTESIAN_POINT ( 'NONE',  ( 109.0695705685756565, -106.4195705685758213, 9.999999999999669598 ) ) ;
#12050 = CARTESIAN_POINT ( 'NONE',  ( 8.999999999999998224, -91.65951123222436081, -71.09524597798180423 ) ) ;
#12051 = CYLINDRICAL_SURFACE ( 'NONE', #16221, 58.99999999999998579 ) ;
#12052 = CIRCLE ( 'NONE', #28782, 13.60000000000000142 ) ;
#12053 = EDGE_LOOP ( 'NONE', ( #21162, #9432, #7377, #16241 ) ) ;
#12054 = CARTESIAN_POINT ( 'NONE',  ( -24.68525358734468611, 40.00000000000000000, -18.92943107747915832 ) ) ;
#12055 = ORIENTED_EDGE ( 'NONE', *, *, #33121, .F. ) ;
#12056 = CARTESIAN_POINT ( 'NONE',  ( 0.000000000000000000, -19.44205635905511897, -43.33776004284629124 ) ) ;
#12057 = CARTESIAN_POINT ( 'NONE',  ( 0.000000000000000000, 28.57802095670106723, -14.28532136906642691 ) ) ;
#12058 = ORIENTED_EDGE ( 'NONE', *, *, #30962, .F. ) ;
#12059 = DIRECTION ( 'NONE',  ( -1.000000000000000000, -0.000000000000000000, 0.000000000000000000 ) ) ;
#12060 = CIRCLE ( 'NONE', #26678, 52.00000000000000000 ) ;
#12061 = ORIENTED_EDGE ( 'NONE', *, *, #8861, .T. ) ;
#12062 = DIRECTION ( 'NONE',  ( 1.000000000000000000, 0.000000000000000000, 0.000000000000000000 ) ) ;
#12063 = VERTEX_POINT ( 'NONE', #7991 ) ;
#12064 = AXIS2_PLACEMENT_3D ( 'NONE', #27470, #1273, #18340 ) ;
#12065 = ORIENTED_EDGE ( 'NONE', *, *, #21246, .F. ) ;
#12066 = DIRECTION ( 'NONE',  ( 0.000000000000000000, 0.000000000000000000, -1.000000000000000000 ) ) ;
#12067 = CARTESIAN_POINT ( 'NONE',  ( 52.26791824981292223, 31.00000000000000355, -67.94187691988643962 ) ) ;
#12068 = VERTEX_POINT ( 'NONE', #41797 ) ;
#12069 = DIRECTION ( 'NONE',  ( -1.000000000000000000, -0.000000000000000000, -0.000000000000000000 ) ) ;
#12070 = EDGE_CURVE ( 'NONE', #2989, #8080, #35509, .T. ) ;
#12071 = FACE_OUTER_BOUND ( 'NONE', #41911, .T. ) ;
#12072 = EDGE_CURVE ( 'NONE', #8432, #38324, #21359, .T. ) ;
#12073 = VERTEX_POINT ( 'NONE', #8429 ) ;
#12074 = CARTESIAN_POINT ( 'NONE',  ( 17.99999999999999645, 0.000000000000000000, 0.000000000000000000 ) ) ;
#12075 = PRODUCT_DEFINITION_SHAPE ( 'NONE', 'NONE',  #43214 ) ;
#12076 = CARTESIAN_POINT ( 'NONE',  ( 0.000000000000000000, -110.0562500189195561, -49.07252625220222342 ) ) ;
#12077 = CARTESIAN_POINT ( 'NONE',  ( 15.59370980024835696, 31.00000000000000355, -20.29731371384564653 ) ) ;
#12079 = CARTESIAN_POINT ( 'NONE',  ( 9.999999999999998224, 12.59999999999999964, 0.000000000000000000 ) ) ;
#12078 = CARTESIAN_POINT ( 'NONE',  ( 17.99999999999999645, 0.000000000000000000, 0.000000000000000000 ) ) ;
#12080 = EDGE_CURVE ( 'NONE', #22453, #18907, #7667, .T. ) ;
#12081 = FACE_OUTER_BOUND ( 'NONE', #123, .T. ) ;
#12082 = DIRECTION ( 'NONE',  ( 0.000000000000000000, -0.8993121301712230231, 0.4373073204588476259 ) ) ;
#12083 = ORIENTED_EDGE ( 'NONE', *, *, #32837, .F. ) ;
#12084 = EDGE_CURVE ( 'NONE', #37344, #19147, #29992, .T. ) ;
#12085 = ORIENTED_EDGE ( 'NONE', *, *, #1358, .T. ) ;
#12086 = DIRECTION ( 'NONE',  ( 1.000000000000000000, 0.000000000000000000, 0.000000000000000000 ) ) ;
#12087 = EDGE_CURVE ( 'NONE', #20302, #30905, #41072, .T. ) ;
#12088 = CARTESIAN_POINT ( 'NONE',  ( 72.43982367323130234, 31.00000000000000000, 63.53091779346544143 ) ) ;
#12089 = DIRECTION ( 'NONE',  ( -1.000000000000000000, -0.000000000000000000, -0.000000000000000000 ) ) ;
#12090 = VERTEX_POINT ( 'NONE', #15638 ) ;
#12091 = ADVANCED_FACE ( 'NONE', ( #9715 ), #28736, .T. ) ;
#12092 = CARTESIAN_POINT ( 'NONE',  ( -7.231618336280544845, 40.00000000000000000, 27.02512817425793656 ) ) ;
#12093 = CARTESIAN_POINT ( 'NONE',  ( 12.49611804805956439, 40.00000000000000000, 37.00809541493615740 ) ) ;
#12094 = EDGE_LOOP ( 'NONE', ( #6277, #37035, #29960, #35486 ) ) ;
#12095 = VERTEX_POINT ( 'NONE', #32410 ) ;
#12096 = CARTESIAN_POINT ( 'NONE',  ( 18.00000000000000355, 39.64889472655779201, -33.64468972902464117 ) ) ;
#12097 = DIRECTION ( 'NONE',  ( 1.000000000000000000, 1.836909530733573776E-16, 0.000000000000000000 ) ) ;
#12098 = DIRECTION ( 'NONE',  ( 0.000000000000000000, 0.3612416661871538093, -0.9324722294043554793 ) ) ;
#12099 = DIRECTION ( 'NONE',  ( -1.000000000000000000, -0.000000000000000000, -0.000000000000000000 ) ) ;
#12100 = EDGE_CURVE ( 'NONE', #39291, #24752, #22323, .T. ) ;
#12101 = FACE_OUTER_BOUND ( 'NONE', #29841, .T. ) ;
#12102 = ORIENTED_EDGE ( 'NONE', *, *, #5997, .F. ) ;
#12103 = DIRECTION ( 'NONE',  ( 1.000000000000000000, 0.000000000000000000, 0.000000000000000000 ) ) ;
#12104 = ORIENTED_EDGE ( 'NONE', *, *, #37550, .F. ) ;
#12105 = FACE_OUTER_BOUND ( 'NONE', #3999, .T. ) ;
#12106 = EDGE_CURVE ( 'NONE', #40378, #4807, #26079, .T. ) ;
#12107 = DIRECTION ( 'NONE',  ( 1.000000000000000000, 0.000000000000000000, -0.000000000000000000 ) ) ;
#12108 = EDGE_CURVE ( 'NONE', #28770, #22696, #3127, .T. ) ;
#12109 = DIRECTION ( 'NONE',  ( -1.000000000000000000, 0.000000000000000000, 0.000000000000000000 ) ) ;
#12110 = AXIS2_PLACEMENT_3D ( 'NONE', #12355, #5358, #35860 ) ;
#12111 = CYLINDRICAL_SURFACE ( 'NONE', #33137, 20.00000000000000355 ) ;
#12112 = ORIENTED_EDGE ( 'NONE', *, *, #14841, .T. ) ;
#12113 = ORIENTED_EDGE ( 'NONE', *, *, #11919, .F. ) ;
#12114 = DIRECTION ( 'NONE',  ( 1.000000000000000000, 0.000000000000000000, 0.000000000000000000 ) ) ;
#12115 = CIRCLE ( 'NONE', #36449, 58.99999999999999289 ) ;
#12116 = ORIENTED_EDGE ( 'NONE', *, *, #35010, .F. ) ;
#12118 = VERTEX_POINT ( 'NONE', #39586 ) ;
#12117 = CARTESIAN_POINT ( 'NONE',  ( 18.00000000000000355, -51.93417535146739539, -2.615612846549722370 ) ) ;
#12119 = CARTESIAN_POINT ( 'NONE',  ( -33.53193138075044999, 31.00000000000000355, 38.09769221459629307 ) ) ;
#12120 = ORIENTED_EDGE ( 'NONE', *, *, #29246, .T. ) ;
#12121 = DIRECTION ( 'NONE',  ( 0.000000000000000000, 0.000000000000000000, 1.000000000000000000 ) ) ;
#12122 =( GEOMETRIC_REPRESENTATION_CONTEXT ( 3 ) GLOBAL_UNCERTAINTY_ASSIGNED_CONTEXT ( ( #18604 ) ) GLOBAL_UNIT_ASSIGNED_CONTEXT ( ( #12510, #14936, #38883 ) ) REPRESENTATION_CONTEXT ( 'NONE', 'WORKASPACE' ) );
#12123 = ADVANCED_FACE ( 'NONE', ( #2706 ), #19778, .F. ) ;
#12124 = CARTESIAN_POINT ( 'NONE',  ( -10.00000000000000000, 0.000000000000000000, 0.000000000000000000 ) ) ;
#12125 = VERTEX_POINT ( 'NONE', #2917 ) ;
#12126 = CARTESIAN_POINT ( 'NONE',  ( 72.60479858918233731, 39.99999999999999289, -24.53750584076950858 ) ) ;
#12127 = DIRECTION ( 'NONE',  ( -1.000000000000000000, -0.000000000000000000, -0.000000000000000000 ) ) ;
#12128 = DIRECTION ( 'NONE',  ( 1.000000000000000000, 0.000000000000000000, 0.000000000000000000 ) ) ;
#12129 = EDGE_LOOP ( 'NONE', ( #12438, #41077, #7244, #18555 ) ) ;
#12130 = DIRECTION ( 'NONE',  ( 0.000000000000000000, 0.000000000000000000, 1.000000000000000000 ) ) ;
#12131 = AXIS2_PLACEMENT_3D ( 'NONE', #20388, #17346, #30184 ) ;
#12132 = ORIENTED_EDGE ( 'NONE', *, *, #891, .T. ) ;
#12133 = EDGE_CURVE ( 'NONE', #17236, #22453, #2496, .T. ) ;
#12134 = FILL_AREA_STYLE ('',( #35858 ) ) ;
#12135 = CARTESIAN_POINT ( 'NONE',  ( 17.99999999999999645, 108.8684555192046872, 27.12806418649654105 ) ) ;
#12136 = DIRECTION ( 'NONE',  ( 0.000000000000000000, 0.000000000000000000, 1.000000000000000000 ) ) ;
#12137 = EDGE_CURVE ( 'NONE', #300, #10648, #7237, .T. ) ;
#12138 = CARTESIAN_POINT ( 'NONE',  ( 17.40022565512299479, 31.00000000000000355, 64.93645345284011228 ) ) ;
#12140 = FACE_OUTER_BOUND ( 'NONE', #43036, .T. ) ;
#12139 = CARTESIAN_POINT ( 'NONE',  ( 17.99999999999999645, 9.484061862023926537, 30.03730300138984433 ) ) ;
#12141 = ORIENTED_EDGE ( 'NONE', *, *, #6550, .T. ) ;
#12142 = CIRCLE ( 'NONE', #17731, 58.99999999999999289 ) ;
#12143 = EDGE_CURVE ( 'NONE', #20227, #40931, #42635, .T. ) ;
#12144 = CARTESIAN_POINT ( 'NONE',  ( -10.00000000000000000, 0.000000000000000000, 0.000000000000000000 ) ) ;
#12145 = ORIENTED_EDGE ( 'NONE', *, *, #20444, .F. ) ;
#12146 = FACE_OUTER_BOUND ( 'NONE', #36646, .T. ) ;
#12147 = CARTESIAN_POINT ( 'NONE',  ( 17.99999999999999645, 0.000000000000000000, 0.000000000000000000 ) ) ;
#12148 = CARTESIAN_POINT ( 'NONE',  ( 5.650912336215120568, 31.00000000000000355, -84.59266001507907617 ) ) ;
#12149 = CARTESIAN_POINT ( 'NONE',  ( -21.69137426901471954, 40.00000000000000000, -81.42030341110599068 ) ) ;
#12150 = CARTESIAN_POINT ( 'NONE',  ( 42.80287614962790599, -40.05525454449572464, 69.29271901957253021 ) ) ;
#12151 = PRODUCT_DEFINITION_FORMATION_WITH_SPECIFIED_SOURCE ( 'ANY', '', #29058, .NOT_KNOWN. ) ;
#12152 = ORIENTED_EDGE ( 'NONE', *, *, #18759, .T. ) ;
#12153 = CARTESIAN_POINT ( 'NONE',  ( 17.99999999999999645, 104.2166695095720854, -60.49278301857700768 ) ) ;
#12154 = VERTEX_POINT ( 'NONE', #42432 ) ;
#12155 = AXIS2_PLACEMENT_3D ( 'NONE', #17668, #40950, #23559 ) ;
#12156 = EDGE_CURVE ( 'NONE', #16072, #40285, #22419, .T. ) ;
#12157 = CARTESIAN_POINT ( 'NONE',  ( 18.00000000000000355, -47.32430374665916162, -21.55018039121577189 ) ) ;
#12158 = EDGE_CURVE ( 'NONE', #16458, #17796, #19157, .T. ) ;
#12160 = ORIENTED_EDGE ( 'NONE', *, *, #28656, .F. ) ;
#12159 = CYLINDRICAL_SURFACE ( 'NONE', #8189, 47.49900000000000233 ) ;
#12161 = CARTESIAN_POINT ( 'NONE',  ( 17.99999999999999645, 0.000000000000000000, 0.000000000000000000 ) ) ;
#12162 = VERTEX_POINT ( 'NONE', #12785 ) ;
#12163 = DIRECTION ( 'NONE',  ( 1.000000000000000000, 0.000000000000000000, -0.000000000000000000 ) ) ;
#12164 = AXIS2_PLACEMENT_3D ( 'NONE', #39866, #9993, #26170 ) ;
#12165 = DIRECTION ( 'NONE',  ( -3.009274222672345096E-17, -1.000000000000000000, 2.455023325076454960E-18 ) ) ;
#12166 = AXIS2_PLACEMENT_3D ( 'NONE', #15515, #21655, #9146 ) ;
#12167 = DIRECTION ( 'NONE',  ( -3.996523416598930318E-16, 2.658563593772947863E-15, 1.000000000000000000 ) ) ;
#12168 = AXIS2_PLACEMENT_3D ( 'NONE', #10362, #29807, #30441 ) ;
#12169 = ORIENTED_EDGE ( 'NONE', *, *, #17366, .F. ) ;
#12170 = CARTESIAN_POINT ( 'NONE',  ( -1.240299975428134203E-15, -4.736529461165891242, -3.681130640444276292 ) ) ;
#12171 = CARTESIAN_POINT ( 'NONE',  ( 17.99999999999999645, 23.10276247328101817, 118.2656051737070726 ) ) ;
#12172 = VECTOR ( 'NONE', #6260, 1000.000000000000000 ) ;
#12173 = EDGE_CURVE ( 'NONE', #27156, #8183, #35670, .T. ) ;
#12175 = LINE ( 'NONE', #35274, #20645 ) ;
#12174 = FACE_OUTER_BOUND ( 'NONE', #35184, .T. ) ;
#12176 = AXIS2_PLACEMENT_3D ( 'NONE', #28325, #21148, #11748 ) ;
#12177 = VERTEX_POINT ( 'NONE', #6221 ) ;
#12178 = DIRECTION ( 'NONE',  ( -1.000000000000000000, -0.000000000000000000, 0.000000000000000000 ) ) ;
#12179 = CARTESIAN_POINT ( 'NONE',  ( -3.680118525130244400, 2.494084732383327285, -0.3507732604232449702 ) ) ;
#12180 = CARTESIAN_POINT ( 'NONE',  ( -11.35616125661516307, 40.00000000000000000, -42.69191301636733726 ) ) ;
#12181 = CARTESIAN_POINT ( 'NONE',  ( 0.000000000000000000, 115.6826031496113529, -8.575274253896266075 ) ) ;
#12182 = DIRECTION ( 'NONE',  ( -1.000000000000000000, 0.000000000000000000, 0.000000000000000000 ) ) ;
#12183 = FACE_OUTER_BOUND ( 'NONE', #28295, .T. ) ;
#12184 = ORIENTED_EDGE ( 'NONE', *, *, #34556, .T. ) ;
#12185 = VERTEX_POINT ( 'NONE', #7366 ) ;
#12186 = DIRECTION ( 'NONE',  ( 0.000000000000000000, -0.4999999999999993339, 0.8660254037844390407 ) ) ;
#12187 = VERTEX_POINT ( 'NONE', #12576 ) ;
#12188 = EDGE_CURVE ( 'NONE', #31468, #12550, #31643, .T. ) ;
#12189 = DIRECTION ( 'NONE',  ( -1.058513553088275437E-16, -1.000000000000000000, 8.813324511995299047E-17 ) ) ;
#12190 = CARTESIAN_POINT ( 'NONE',  ( 9.000000000000001776, -25.61928775981013118, -45.25098998563503727 ) ) ;
#12191 = EDGE_CURVE ( 'NONE', #17669, #16188, #20526, .T. ) ;
#12192 = CARTESIAN_POINT ( 'NONE',  ( 34.56606645648713538, 31.00000000000000355, -4.560848911255810378 ) ) ;
#12193 = ORIENTED_EDGE ( 'NONE', *, *, #24578, .F. ) ;
#12194 = DIRECTION ( 'NONE',  ( -1.000000000000000000, 0.000000000000000000, -0.000000000000000000 ) ) ;
#12195 = ORIENTED_EDGE ( 'NONE', *, *, #34762, .T. ) ;
#12196 = AXIS2_PLACEMENT_3D ( 'NONE', #24870, #35487, #21814 ) ;
#12197 = CYLINDRICAL_SURFACE ( 'NONE', #21939, 25.00000000000000000 ) ;
#12198 = CARTESIAN_POINT ( 'NONE',  ( 64.90595555533579386, 31.00000000000000000, 56.92265028768127166 ) ) ;
#12199 = AXIS2_PLACEMENT_3D ( 'NONE', #37607, #1388, #21529 ) ;
#12200 = EDGE_CURVE ( 'NONE', #41108, #11023, #4462, .T. ) ;
#12201 = VERTEX_POINT ( 'NONE', #42213 ) ;
#12202 = CARTESIAN_POINT ( 'NONE',  ( -50.71442127988192539, 31.00000000000000355, -13.67646662467867991 ) ) ;
#12203 = AXIS2_PLACEMENT_3D ( 'NONE', #33732, #13916, #3608 ) ;
#12204 = CARTESIAN_POINT ( 'NONE',  ( 57.06996419936330511, 39.99999999999999289, 65.05326946697847745 ) ) ;
#12205 = VERTEX_POINT ( 'NONE', #12370 ) ;
#12206 = CYLINDRICAL_SURFACE ( 'NONE', #16504, 51.99999999999999289 ) ;
#12207 = ADVANCED_FACE ( 'NONE', ( #22631 ), #9499, .T. ) ;
#12208 = CARTESIAN_POINT ( 'NONE',  ( 17.99999999999999645, 0.000000000000000000, 0.000000000000000000 ) ) ;
#12209 = DIRECTION ( 'NONE',  ( -1.000000000000000000, -0.000000000000000000, -0.000000000000000000 ) ) ;
#12210 = ADVANCED_FACE ( 'NONE', ( #36744 ), #9917, .F. ) ;
#12211 = ADVANCED_FACE ( 'NONE', ( #13651 ), #36518, .F. ) ;
#12212 = EDGE_CURVE ( 'NONE', #7685, #9595, #12839, .T. ) ;
#12214 = EDGE_LOOP ( 'NONE', ( #21836, #40479, #18051, #31736 ) ) ;
#12213 = DIRECTION ( 'NONE',  ( 1.000000000000000000, -0.000000000000000000, -0.000000000000000000 ) ) ;
#12215 = DIRECTION ( 'NONE',  ( 1.000000000000000000, 0.000000000000000000, 0.000000000000000000 ) ) ;
#12216 = CARTESIAN_POINT ( 'NONE',  ( 18.00000000000000355, 0.000000000000000000, 0.000000000000000000 ) ) ;
#12217 = AXIS2_PLACEMENT_3D ( 'NONE', #39344, #6413, #33028 ) ;
#12218 = VERTEX_POINT ( 'NONE', #30017 ) ;
#12219 = CARTESIAN_POINT ( 'NONE',  ( -75.41724699911947027, 40.00000000000000711, 25.61573074746135248 ) ) ;
#12220 = DIRECTION ( 'NONE',  ( -1.000000000000000000, 0.000000000000000000, -0.000000000000000000 ) ) ;
#12221 = EDGE_LOOP ( 'NONE', ( #30276, #7093, #38213, #1598 ) ) ;
#12222 = DIRECTION ( 'NONE',  ( 0.000000000000000000, 0.1253332335642974860, 0.9921147013144787641 ) ) ;
#12223 = VERTEX_POINT ( 'NONE', #26951 ) ;
#12224 = AXIS2_PLACEMENT_3D ( 'NONE', #38647, #2202, #25187 ) ;
#12225 = ORIENTED_EDGE ( 'NONE', *, *, #18087, .F. ) ;
#12226 = CARTESIAN_POINT ( 'NONE',  ( 18.00000000000000355, -46.90537658765328644, -2.727856614654796452 ) ) ;
#12227 = ORIENTED_EDGE ( 'NONE', *, *, #33408, .T. ) ;
#12228 = DIRECTION ( 'NONE',  ( -1.000000000000000000, 0.000000000000000000, 0.000000000000000000 ) ) ;
#12229 = CARTESIAN_POINT ( 'NONE',  ( 0.000000000000000000, -150.5000000000000284, 10.00000000000000000 ) ) ;
#12230 = VECTOR ( 'NONE', #22033, 1000.000000000000000 ) ;
#12231 = DIRECTION ( 'NONE',  ( -1.000000000000000000, -0.000000000000000000, 0.000000000000000000 ) ) ;
#12232 = CYLINDRICAL_SURFACE ( 'NONE', #21380, 120.5010000000000190 ) ;
#12233 = ORIENTED_EDGE ( 'NONE', *, *, #24530, .T. ) ;
#12234 = CARTESIAN_POINT ( 'NONE',  ( 17.99999999999999645, 35.54274411428057334, 115.1399337407607959 ) ) ;
#12236 = EDGE_LOOP ( 'NONE', ( #31647, #41593, #26274, #42067 ) ) ;
#12235 = AXIS2_PLACEMENT_3D ( 'NONE', #17110, #9449, #3312 ) ;
#12237 = CYLINDRICAL_SURFACE ( 'NONE', #30814, 47.49900000000000233 ) ;
#12238 = EDGE_CURVE ( 'NONE', #30905, #22661, #5871, .T. ) ;
#12239 = ORIENTED_EDGE ( 'NONE', *, *, #37006, .F. ) ;
#12240 = CARTESIAN_POINT ( 'NONE',  ( 0.000000000000000000, -64.69195966009955612, 96.28577441832231898 ) ) ;
#12241 = CARTESIAN_POINT ( 'NONE',  ( 0.000000000000000000, 0.5156212287279957618, 112.1962860721878172 ) ) ;
#12242 = CARTESIAN_POINT ( 'NONE',  ( 150.5000000000000284, 17.99999999999998934, -1.580066075643184531E-12 ) ) ;
#12243 = DIRECTION ( 'NONE',  ( -1.000000000000000000, 0.000000000000000000, -0.000000000000000000 ) ) ;
#12244 = CARTESIAN_POINT ( 'NONE',  ( -44.28363997456384737, 31.00000000000000355, 21.84072794957603492 ) ) ;
#12245 = ORIENTED_EDGE ( 'NONE', *, *, #12993, .T. ) ;
#12246 = DIRECTION ( 'NONE',  ( 1.058513553088275437E-16, 1.000000000000000000, -8.813324511995299047E-17 ) ) ;
#12248 = VERTEX_POINT ( 'NONE', #3770 ) ;
#12247 = AXIS2_PLACEMENT_3D ( 'NONE', #41980, #2259, #42188 ) ;
#12249 = AXIS2_PLACEMENT_3D ( 'NONE', #10492, #1310, #37096 ) ;
#12250 = CARTESIAN_POINT ( 'NONE',  ( -46.07128526072433772, 40.00000000000000000, -40.40198152342698990 ) ) ;
#12251 = VECTOR ( 'NONE', #3691, 1000.000000000000000 ) ;
#12252 = AXIS2_PLACEMENT_3D ( 'NONE', #24951, #6265, #32880 ) ;
#12253 = DIRECTION ( 'NONE',  ( 1.000000000000000000, -0.000000000000000000, -0.000000000000000000 ) ) ;
#12254 = VECTOR ( 'NONE', #27644, 1000.000000000000000 ) ;
#12255 = DIRECTION ( 'NONE',  ( 0.000000000000000000, 0.9968120070307497915, 0.07978610555308651708 ) ) ;
#12256 = MECHANICAL_DESIGN_GEOMETRIC_PRESENTATION_REPRESENTATION (  '', ( #25519 ), #39405 ) ;
#12257 = EDGE_CURVE ( 'NONE', #1606, #36282, #5163, .T. ) ;
#12258 = EDGE_CURVE ( 'NONE', #12380, #25306, #30278, .T. ) ;
#12259 = DIRECTION ( 'NONE',  ( 0.000000000000000000, 0.000000000000000000, -1.000000000000000000 ) ) ;
#12260 = FACE_OUTER_BOUND ( 'NONE', #13491, .T. ) ;
#12261 = EDGE_CURVE ( 'NONE', #255, #1619, #11481, .T. ) ;
#12262 = CIRCLE ( 'NONE', #24141, 120.5010000000000332 ) ;
#12263 = ORIENTED_EDGE ( 'NONE', *, *, #2465, .T. ) ;
#12264 = CARTESIAN_POINT ( 'NONE',  ( -19.19493090124598922, 40.00000000000000000, -25.00897302100653263 ) ) ;
#12265 = ORIENTED_EDGE ( 'NONE', *, *, #18558, .T. ) ;
#12266 = DIRECTION ( 'NONE',  ( -1.000000000000000000, 0.000000000000000000, 0.000000000000000000 ) ) ;
#12267 = DIRECTION ( 'NONE',  ( -1.000000000000000000, -0.000000000000000000, -0.000000000000000000 ) ) ;
#12268 = ORIENTED_EDGE ( 'NONE', *, *, #33800, .T. ) ;
#12269 = DIRECTION ( 'NONE',  ( 1.000000000000000000, 0.000000000000000000, 0.000000000000000000 ) ) ;
#12270 = VERTEX_POINT ( 'NONE', #3566 ) ;
#12271 = CARTESIAN_POINT ( 'NONE',  ( 1.567478505476134606E-15, 4.618802153517012066, -3.433295621305382905 ) ) ;
#12272 = VERTEX_POINT ( 'NONE', #20428 ) ;
#12273 = ORIENTED_EDGE ( 'NONE', *, *, #16870, .T. ) ;
#12274 =( REPRESENTATION_RELATIONSHIP ('NONE','NONE', #330, #40225 ) REPRESENTATION_RELATIONSHIP_WITH_TRANSFORMATION ( #9599 )SHAPE_REPRESENTATION_RELATIONSHIP( ) );
#12275 = DIRECTION ( 'NONE',  ( -1.000000000000000000, 0.000000000000000000, 0.000000000000000000 ) ) ;
#12276 = ADVANCED_FACE ( 'NONE', ( #33275 ), #10796, .F. ) ;
#12277 = CARTESIAN_POINT ( 'NONE',  ( 87.09251733236551729, 31.00000000000000000, 5.815661930448015937 ) ) ;
#12278 = VERTEX_POINT ( 'NONE', #16937 ) ;
#12279 = CARTESIAN_POINT ( 'NONE',  ( 0.000000000000000000, 0.000000000000000000, -20.00000000000000000 ) ) ;
#12280 = AXIS2_PLACEMENT_3D ( 'NONE', #29350, #9897, #22828 ) ;
#12282 = DIRECTION ( 'NONE',  ( 3.009274222672345096E-17, 1.000000000000000000, -2.455023325076454960E-18 ) ) ;
#12281 = AXIS2_PLACEMENT_3D ( 'NONE', #35541, #12454, #5020 ) ;
#12283 = ORIENTED_EDGE ( 'NONE', *, *, #23161, .T. ) ;
#12284 = AXIS2_PLACEMENT_3D ( 'NONE', #6858, #20216, #2490 ) ;
#12285 = FACE_OUTER_BOUND ( 'NONE', #5554, .T. ) ;
#12286 = DIRECTION ( 'NONE',  ( 0.000000000000000000, 1.224646799147353207E-16, 1.000000000000000000 ) ) ;
#12287 = CARTESIAN_POINT ( 'NONE',  ( 1.888402776346428835, 31.00000000000000355, 29.39821258742166066 ) ) ;
#12288 = AXIS2_PLACEMENT_3D ( 'NONE', #10836, #17843, #27866 ) ;
#12290 = CARTESIAN_POINT ( 'NONE',  ( -10.00000000000000000, 0.000000000000000000, 0.000000000000000000 ) ) ;
#12289 = CARTESIAN_POINT ( 'NONE',  ( 17.99999999999999645, -111.1352304691228596, 15.40237066878559524 ) ) ;
#12291 = AXIS2_PLACEMENT_3D ( 'NONE', #20975, #13974, #27272 ) ;
#12292 = AXIS2_PLACEMENT_3D ( 'NONE', #34264, #27521, #27306 ) ;
#12293 = CARTESIAN_POINT ( 'NONE',  ( 0.000000000000000000, 0.000000000000000000, 0.000000000000000000 ) ) ;
#12294 = EDGE_CURVE ( 'NONE', #20361, #21959, #30221, .T. ) ;
#12295 = CARTESIAN_POINT ( 'NONE',  ( -10.00000000000000000, 0.000000000000000000, 0.000000000000000000 ) ) ;
#12296 = ORIENTED_EDGE ( 'NONE', *, *, #10535, .F. ) ;
#12297 = FILL_AREA_STYLE ('',( #42138 ) ) ;
#12298 = VECTOR ( 'NONE', #17005, 1000.000000000000000 ) ;
#12299 = ORIENTED_EDGE ( 'NONE', *, *, #15891, .T. ) ;
#12300 = CYLINDRICAL_SURFACE ( 'NONE', #16414, 59.00000000000000000 ) ;
#12301 = LINE ( 'NONE', #39513, #21036 ) ;
#12302 = ORIENTED_EDGE ( 'NONE', *, *, #3748, .T. ) ;
#12303 = CARTESIAN_POINT ( 'NONE',  ( 20.70971545910534672, 40.00000000000000000, 15.87948211774388518 ) ) ;
#12304 = CARTESIAN_POINT ( 'NONE',  ( -20.36888183406675168, 40.00000000000000000, -26.63352584488937325 ) ) ;
#12305 = VERTEX_POINT ( 'NONE', #39999 ) ;
#12306 = VERTEX_POINT ( 'NONE', #10130 ) ;
#12307 = CYLINDRICAL_SURFACE ( 'NONE', #28372, 51.99999999999999289 ) ;
#12308 = LINE ( 'NONE', #25215, #3948 ) ;
#12310 = CARTESIAN_POINT ( 'NONE',  ( 17.99999999999999645, -45.89132998248120288, 102.3829004574628385 ) ) ;
#12309 = AXIS2_PLACEMENT_3D ( 'NONE', #16334, #3191, #19421 ) ;
#12311 = EDGE_CURVE ( 'NONE', #18098, #39874, #13226, .T. ) ;
#12312 = DIRECTION ( 'NONE',  ( -1.000000000000000000, 0.000000000000000000, 0.000000000000000000 ) ) ;
#12313 = AXIS2_PLACEMENT_3D ( 'NONE', #18433, #41724, #28862 ) ;
#12314 = AXIS2_PLACEMENT_3D ( 'NONE', #12817, #42463, #29840 ) ;
#12315 = AXIS2_PLACEMENT_3D ( 'NONE', #15857, #22415, #5579 ) ;
#12316 = CARTESIAN_POINT ( 'NONE',  ( 17.99999999999999645, 0.000000000000000000, 0.000000000000000000 ) ) ;
#12317 = EDGE_LOOP ( 'NONE', ( #2195, #33837, #12431, #5338 ) ) ;
#12318 = DIRECTION ( 'NONE',  ( 0.000000000000000000, 0.000000000000000000, 1.000000000000000000 ) ) ;
#12319 = VERTEX_POINT ( 'NONE', #20874 ) ;
#12320 = FACE_OUTER_BOUND ( 'NONE', #14060, .T. ) ;
#12321 = CARTESIAN_POINT ( 'NONE',  ( 18.00000000000000355, -8.053585752062225822, 46.81126742072019908 ) ) ;
#12322 = AXIS2_PLACEMENT_3D ( 'NONE', #36043, #14031, #30605 ) ;
#12323 = AXIS2_PLACEMENT_3D ( 'NONE', #2082, #28539, #8639 ) ;
#12324 = EDGE_CURVE ( 'NONE', #31747, #19127, #9329, .T. ) ;
#12325 = DIRECTION ( 'NONE',  ( 0.000000000000000000, 0.3681245526846720906, 0.9297764858882537897 ) ) ;
#12326 = DIRECTION ( 'NONE',  ( -1.000000000000000000, 0.000000000000000000, -0.000000000000000000 ) ) ;
#12327 = ORIENTED_EDGE ( 'NONE', *, *, #41149, .F. ) ;
#12328 = CARTESIAN_POINT ( 'NONE',  ( -49.27414759474276451, 40.00000000000000711, 85.34056160678568403 ) ) ;
#12329 = ORIENTED_EDGE ( 'NONE', *, *, #37504, .T. ) ;
#12330 = DIRECTION ( 'NONE',  ( 0.000000000000000000, 0.000000000000000000, 1.000000000000000000 ) ) ;
#12331 = EDGE_CURVE ( 'NONE', #4861, #12270, #970, .T. ) ;
#12332 = AXIS2_PLACEMENT_3D ( 'NONE', #40081, #6500, #6295 ) ;
#12333 = VERTEX_POINT ( 'NONE', #6865 ) ;
#12335 = ORIENTED_EDGE ( 'NONE', *, *, #40108, .T. ) ;
#12334 = CARTESIAN_POINT ( 'NONE',  ( 17.99999999999999645, 0.000000000000000000, 0.000000000000000000 ) ) ;
#12336 = CARTESIAN_POINT ( 'NONE',  ( 50.14038141241295676, 31.00000000000000355, 29.06424286984032435 ) ) ;
#12337 = ORIENTED_EDGE ( 'NONE', *, *, #3824, .T. ) ;
#12338 = DIRECTION ( 'NONE',  ( 0.000000000000000000, 0.8747630845319591675, 0.4845508703326539823 ) ) ;
#12339 = CIRCLE ( 'NONE', #5344, 59.00000000000000000 ) ;
#12340 = FACE_BOUND ( 'NONE', #37292, .T. ) ;
#12341 = PRODUCT_DEFINITION_SHAPE ( 'NONE', 'NONE',  #43195 ) ;
#12342 = EDGE_LOOP ( 'NONE', ( #16646, #5728, #33541, #41158 ) ) ;
#12343 = CARTESIAN_POINT ( 'NONE',  ( 19.52887458859586900, 40.00000000000000000, -72.48875405283516216 ) ) ;
#12344 = VECTOR ( 'NONE', #14584, 1000.000000000000000 ) ;
#12346 = DIRECTION ( 'NONE',  ( 0.000000000000000000, 0.000000000000000000, 1.000000000000000000 ) ) ;
#12345 = DIRECTION ( 'NONE',  ( -1.000000000000000000, 0.000000000000000000, 0.000000000000000000 ) ) ;
#12347 = CARTESIAN_POINT ( 'NONE',  ( 17.99999999999999645, -7.749090474611724844, 30.53094492177211094 ) ) ;
#12348 = ORIENTED_EDGE ( 'NONE', *, *, #29913, .T. ) ;
#12349 = CARTESIAN_POINT ( 'NONE',  ( 56.05503971749756431, -2.055254544495723756, 8.006123197671259462 ) ) ;
#12350 = CIRCLE ( 'NONE', #21448, 116.0000000000000000 ) ;
#12351 = ORIENTED_EDGE ( 'NONE', *, *, #23032, .T. ) ;
#12352 =( LENGTH_UNIT ( ) NAMED_UNIT ( * ) SI_UNIT ( .MILLI., .METRE. ) );
#12353 = EDGE_CURVE ( 'NONE', #10174, #41147, #42752, .T. ) ;
#12354 = CIRCLE ( 'NONE', #37389, 20.00000000000000711 ) ;
#12355 = CARTESIAN_POINT ( 'NONE',  ( 0.000000000000000000, 0.000000000000000000, 0.000000000000000000 ) ) ;
#12356 = FACE_OUTER_BOUND ( 'NONE', #31592, .T. ) ;
#12357 = CIRCLE ( 'NONE', #24935, 10.49999999999998934 ) ;
#12358 = CARTESIAN_POINT ( 'NONE',  ( 63.32575250126041055, 31.00000000000000000, 16.95471465585521997 ) ) ;
#12360 = CARTESIAN_POINT ( 'NONE',  ( 22.90854556226730310, -35.35525454449573601, -74.83297477053802993 ) ) ;
#12359 = CARTESIAN_POINT ( 'NONE',  ( 18.00000000000000355, 39.64889472655730884, 33.64468972902522381 ) ) ;
#12362 = ORIENTED_EDGE ( 'NONE', *, *, #10999, .F. ) ;
#12361 = CIRCLE ( 'NONE', #13077, 36.00000000000000000 ) ;
#12364 = AXIS2_PLACEMENT_3D ( 'NONE', #4167, #17752, #39588 ) ;
#12363 = CARTESIAN_POINT ( 'NONE',  ( 0.000000000000000000, 18.25486108452660972, -25.66996392254254644 ) ) ;
#12365 = EDGE_LOOP ( 'NONE', ( #20839, #36710, #27320, #35731 ) ) ;
#12366 = CARTESIAN_POINT ( 'NONE',  ( 18.00000000000000355, -40.47821179127690527, -32.64221760512803172 ) ) ;
#12367 = DIRECTION ( 'NONE',  ( -1.000000000000000000, -0.000000000000000000, -0.000000000000000000 ) ) ;
#12368 = CARTESIAN_POINT ( 'NONE',  ( -89.42636861580037078, 31.00000000000000711, -24.07434901466544730 ) ) ;
#12369 = CARTESIAN_POINT ( 'NONE',  ( -56.91377077966711084, 40.00000000000000000, -74.37798324515208037 ) ) ;
#12370 = CARTESIAN_POINT ( 'NONE',  ( 17.99999999999999645, 90.81729652456166946, 72.16798910853647442 ) ) ;
#12371 = ADVANCED_FACE ( 'NONE', ( #13875 ), #27171, .F. ) ;
#12372 = VERTEX_POINT ( 'NONE', #30657 ) ;
#12373 = CARTESIAN_POINT ( 'NONE',  ( 17.99999999999999645, 35.54274411428215075, -115.1399337407602701 ) ) ;
#12374 = VERTEX_POINT ( 'NONE', #727 ) ;
#12375 = DIRECTION ( 'NONE',  ( -1.000000000000000000, -0.000000000000000000, -0.000000000000000000 ) ) ;
#12376 = AXIS2_PLACEMENT_3D ( 'NONE', #14961, #27612, #28051 ) ;
#12378 = ORIENTED_EDGE ( 'NONE', *, *, #24651, .F. ) ;
#12377 = DIRECTION ( 'NONE',  ( 0.000000000000000000, -0.7705132427757815927, -0.6374239897486989603 ) ) ;
#12379 = CARTESIAN_POINT ( 'NONE',  ( 5.000000000000000888, 4.250000000000000000, 0.000000000000000000 ) ) ;
#12380 = VERTEX_POINT ( 'NONE', #14092 ) ;
#12381 = FACE_OUTER_BOUND ( 'NONE', #16135, .T. ) ;
#12382 = AXIS2_PLACEMENT_3D ( 'NONE', #38841, #5261, #25366 ) ;
#12383 = CARTESIAN_POINT ( 'NONE',  ( 0.000000000000000000, 104.6166166098445416, 50.11350645393712000 ) ) ;
#12384 = EDGE_CURVE ( 'NONE', #18335, #20343, #17034, .T. ) ;
#12385 = AXIS2_PLACEMENT_3D ( 'NONE', #21490, #4849, #18209 ) ;
#12386 = CARTESIAN_POINT ( 'NONE',  ( 0.000000000000000000, -69.90696807222551001, 98.15042952503490881 ) ) ;
#12387 = CIRCLE ( 'NONE', #16568, 51.99999999999999289 ) ;
#12388 = CIRCLE ( 'NONE', #29103, 59.00000000000000000 ) ;
#12389 = ORIENTED_EDGE ( 'NONE', *, *, #21394, .F. ) ;
#12390 = CARTESIAN_POINT ( 'NONE',  ( -14.30682334061562067, 31.00000000000000355, -18.65445469299708492 ) ) ;
#12391 = DIRECTION ( 'NONE',  ( 1.000000000000000000, 0.000000000000000000, 0.000000000000000000 ) ) ;
#12393 = ORIENTED_EDGE ( 'NONE', *, *, #24195, .T. ) ;
#12392 = CARTESIAN_POINT ( 'NONE',  ( 17.99999999999999645, 100.8494052988179561, -65.95368414178808791 ) ) ;
#12394 = ORIENTED_EDGE ( 'NONE', *, *, #22375, .F. ) ;
#12395 = CARTESIAN_POINT ( 'NONE',  ( 17.99999999999999645, 47.58001226230536673, 110.7096808509485300 ) ) ;
#12396 = DIRECTION ( 'NONE',  ( 0.000000000000000000, -6.982962677686266711E-15, 1.000000000000000000 ) ) ;
#12397 = CARTESIAN_POINT ( 'NONE',  ( 5.076274692535532651, 40.00000000000000000, 39.04542013319162663 ) ) ;
#12398 = DIRECTION ( 'NONE',  ( -3.996523416598930318E-16, 2.658563593772947863E-15, 1.000000000000000000 ) ) ;
#12399 = AXIS2_PLACEMENT_3D ( 'NONE', #12815, #32865, #36131 ) ;
#12400 = CARTESIAN_POINT ( 'NONE',  ( 17.99999999999999645, -111.2721026680459602, -14.38025178762732104 ) ) ;
#12401 = CYLINDRICAL_SURFACE ( 'NONE', #19301, 59.00000000000000000 ) ;
#12402 = ORIENTED_EDGE ( 'NONE', *, *, #8793, .T. ) ;
#12403 = CARTESIAN_POINT ( 'NONE',  ( 0.000000000000000000, 0.000000000000000000, 36.00000000000000000 ) ) ;
#12404 = ORIENTED_EDGE ( 'NONE', *, *, #8187, .F. ) ;
#12405 = EDGE_CURVE ( 'NONE', #6807, #6792, #34338, .T. ) ;
#12406 = CARTESIAN_POINT ( 'NONE',  ( 17.99999999999999645, -120.2856157092986393, -7.201503623198056481 ) ) ;
#12407 = DIRECTION ( 'NONE',  ( -1.000000000000000000, 0.000000000000000000, 0.000000000000000000 ) ) ;
#12409 = ADVANCED_FACE ( 'NONE', ( #24568 ), #4887, .F. ) ;
#12408 = CARTESIAN_POINT ( 'NONE',  ( -32.63632984357925437, 31.00000000000000355, -25.02932899672474676 ) ) ;
#12411 = ORIENTED_EDGE ( 'NONE', *, *, #12212, .T. ) ;
#12410 = AXIS2_PLACEMENT_3D ( 'NONE', #25428, #25850, #41962 ) ;
#12412 = DIRECTION ( 'NONE',  ( -1.000000000000000000, 0.000000000000000000, 0.000000000000000000 ) ) ;
#12413 = ORIENTED_EDGE ( 'NONE', *, *, #21243, .T. ) ;
#12414 = CIRCLE ( 'NONE', #42328, 116.0000000000000000 ) ;
#12415 = AXIS2_PLACEMENT_3D ( 'NONE', #7562, #33963, #30491 ) ;
#12416 = DIRECTION ( 'NONE',  ( 0.000000000000000000, 0.9822872507286891652, -0.1873813145857216034 ) ) ;
#12417 = CARTESIAN_POINT ( 'NONE',  ( 89.65113856817994531, 31.00000000000000000, -30.44896562292877462 ) ) ;
#12418 = CIRCLE ( 'NONE', #23576, 51.99999999999999289 ) ;
#12419 = CARTESIAN_POINT ( 'NONE',  ( -31.75000000000000711, 19.99999999999999645, 0.000000000000000000 ) ) ;
#12420 = EDGE_LOOP ( 'NONE', ( #7787, #3892, #42558, #7054 ) ) ;
#12422 = CARTESIAN_POINT ( 'NONE',  ( 60.82800096162477388, 31.00000000000000000, 30.10617641798563682 ) ) ;
#12421 = CIRCLE ( 'NONE', #5456, 116.0000000000000000 ) ;
#12423 = CARTESIAN_POINT ( 'NONE',  ( -22.66037885604484359, 40.00000000000000000, 66.40833514169634100 ) ) ;
#12424 = CARTESIAN_POINT ( 'NONE',  ( -65.18298466990795248, 40.00000000000000711, 74.32329070269128124 ) ) ;
#12425 = EDGE_CURVE ( 'NONE', #20914, #27767, #18249, .T. ) ;
#12426 = ORIENTED_EDGE ( 'NONE', *, *, #11733, .T. ) ;
#12427 = DIRECTION ( 'NONE',  ( 1.000000000000000000, 0.000000000000000000, -0.000000000000000000 ) ) ;
#12428 = CARTESIAN_POINT ( 'NONE',  ( 0.000000000000000000, 0.000000000000000000, 0.000000000000000000 ) ) ;
#12429 = DIRECTION ( 'NONE',  ( -1.000000000000000000, 0.000000000000000000, -0.000000000000000000 ) ) ;
#12431 = ORIENTED_EDGE ( 'NONE', *, *, #20256, .T. ) ;
#12430 = LINE ( 'NONE', #6276, #39425 ) ;
#12432 = DIRECTION ( 'NONE',  ( -1.000000000000000000, 0.000000000000000000, 0.000000000000000000 ) ) ;
#12433 = DIRECTION ( 'NONE',  ( -1.000000000000000000, -0.000000000000000000, -0.000000000000000000 ) ) ;
#12434 = ADVANCED_FACE ( 'NONE', ( #31724, #11234, #18458, #15179, #4221, #25015, #31515, #21941, #28485, #11678 ), #14955, .F. ) ;
#12435 = ORIENTED_EDGE ( 'NONE', *, *, #10616, .F. ) ;
#12436 = CARTESIAN_POINT ( 'NONE',  ( -35.92146702467432817, 40.00000000000000000, -62.19081021767443218 ) ) ;
#12437 = CARTESIAN_POINT ( 'NONE',  ( 0.000000000000000000, 43.83938735307268075, 18.28286404005813637 ) ) ;
#12438 = ORIENTED_EDGE ( 'NONE', *, *, #712, .T. ) ;
#12439 = EDGE_CURVE ( 'NONE', #20683, #38278, #17593, .T. ) ;
#12440 = AXIS2_PLACEMENT_3D ( 'NONE', #21045, #24315, #5056 ) ;
#12441 = CARTESIAN_POINT ( 'NONE',  ( 20.55500000000001748, 0.000000000000000000, 0.000000000000000000 ) ) ;
#12442 = ORIENTED_EDGE ( 'NONE', *, *, #38151, .F. ) ;
#12443 = EDGE_CURVE ( 'NONE', #16643, #43048, #14290, .T. ) ;
#12444 = VECTOR ( 'NONE', #34882, 1000.000000000000000 ) ;
#12445 = AXIS2_PLACEMENT_3D ( 'NONE', #38944, #22210, #25686 ) ;
#12446 = ORIENTED_EDGE ( 'NONE', *, *, #10257, .F. ) ;
#12447 = DIRECTION ( 'NONE',  ( -1.000000000000000000, 0.000000000000000000, 0.000000000000000000 ) ) ;
#12448 = VERTEX_POINT ( 'NONE', #8375 ) ;
#12449 = CIRCLE ( 'NONE', #26392, 116.0000000000000000 ) ;
#12450 = CARTESIAN_POINT ( 'NONE',  ( 0.000000000000000000, 113.8630351447208824, -22.16324045874292636 ) ) ;
#12451 = CARTESIAN_POINT ( 'NONE',  ( 18.00000000000000355, 17.08890430202750110, 43.76671000081951490 ) ) ;
#12452 = CIRCLE ( 'NONE', #17331, 58.99999999999998579 ) ;
#12453 = FACE_OUTER_BOUND ( 'NONE', #272, .T. ) ;
#12454 = DIRECTION ( 'NONE',  ( -0.000000000000000000, -0.000000000000000000, -1.000000000000000000 ) ) ;
#12455 = ORIENTED_EDGE ( 'NONE', *, *, #19034, .T. ) ;
#12456 = DIRECTION ( 'NONE',  ( -1.000000000000000000, 0.000000000000000000, 0.000000000000000000 ) ) ;
#12457 = EDGE_LOOP ( 'NONE', ( #17125, #27128 ) ) ;
#12458 = DIRECTION ( 'NONE',  ( -1.000000000000000000, -0.000000000000000000, -0.000000000000000000 ) ) ;
#12459 = EDGE_CURVE ( 'NONE', #4386, #8463, #10744, .T. ) ;
#12460 = EDGE_CURVE ( 'NONE', #844, #13292, #28258, .T. ) ;
#12461 = VERTEX_POINT ( 'NONE', #25217 ) ;
#12462 = DIRECTION ( 'NONE',  ( 0.000000000000000000, 0.000000000000000000, 1.000000000000000000 ) ) ;
#12463 = EDGE_CURVE ( 'NONE', #41070, #41968, #28884, .T. ) ;
#12464 = EDGE_CURVE ( 'NONE', #35369, #37611, #15654, .T. ) ;
#12465 = LINE ( 'NONE', #12038, #32090 ) ;
#12466 = CARTESIAN_POINT ( 'NONE',  ( 0.000000000000000000, 0.000000000000000000, 0.000000000000000000 ) ) ;
#12467 = CARTESIAN_POINT ( 'NONE',  ( -52.79687664379660816, 31.00000000000000355, -30.48099731442381710 ) ) ;
#12468 = ORIENTED_EDGE ( 'NONE', *, *, #36826, .F. ) ;
#12469 = CARTESIAN_POINT ( 'NONE',  ( 17.99999999999999645, -101.1249659627852679, -48.60055280209521555 ) ) ;
#12470 = VERTEX_POINT ( 'NONE', #8581 ) ;
#12471 = CIRCLE ( 'NONE', #18768, 20.00000000000000711 ) ;
#12472 = CARTESIAN_POINT ( 'NONE',  ( -67.35649507452052376, 40.00000000000000711, 18.04843207638801772 ) ) ;
#12473 = AXIS2_PLACEMENT_3D ( 'NONE', #29320, #12956, #25847 ) ;
#12474 = DIRECTION ( 'NONE',  ( 0.000000000000000000, 0.000000000000000000, 1.000000000000000000 ) ) ;
#12475 = CARTESIAN_POINT ( 'NONE',  ( 3.239593890920906993, -13.56862304811759223, -1.199999999999999956 ) ) ;
#12476 = VECTOR ( 'NONE', #7220, 1000.000000000000000 ) ;
#12477 = DIRECTION ( 'NONE',  ( -1.000000000000000000, -0.000000000000000000, -0.000000000000000000 ) ) ;
#12478 = DIRECTION ( 'NONE',  ( -1.000000000000000000, -0.000000000000000000, 0.000000000000000000 ) ) ;
#12479 = EDGE_CURVE ( 'NONE', #36212, #5428, #21256, .T. ) ;
#12480 = ORIENTED_EDGE ( 'NONE', *, *, #13909, .F. ) ;
#12481 = CARTESIAN_POINT ( 'NONE',  ( -25.29482881991252086, 40.00000000000000000, -32.96004927633274662 ) ) ;
#12482 = CARTESIAN_POINT ( 'NONE',  ( 17.99999999999999645, 0.000000000000000000, 0.000000000000000000 ) ) ;
#12483 = CARTESIAN_POINT ( 'NONE',  ( 18.00000000000000355, 44.61570720899096898, -14.73072383765582671 ) ) ;
#12484 = ORIENTED_EDGE ( 'NONE', *, *, #33087, .F. ) ;
#12485 = EDGE_CURVE ( 'NONE', #38421, #1626, #24770, .T. ) ;
#12486 = LINE ( 'NONE', #25377, #559 ) ;
#12487 = VERTEX_POINT ( 'NONE', #14521 ) ;
#12488 = DIRECTION ( 'NONE',  ( -0.000000000000000000, -0.000000000000000000, -1.000000000000000000 ) ) ;
#12489 = ORIENTED_EDGE ( 'NONE', *, *, #27734, .T. ) ;
#12490 = VERTEX_POINT ( 'NONE', #21089 ) ;
#12491 = CARTESIAN_POINT ( 'NONE',  ( -21.03271207055027503, 17.11489954122026447, 3.044856699593507354 ) ) ;
#12492 = CARTESIAN_POINT ( 'NONE',  ( 74.83201185292551827, 31.00000000000000000, -43.08100868842220166 ) ) ;
#12493 = ORIENTED_EDGE ( 'NONE', *, *, #12608, .T. ) ;
#12494 = CARTESIAN_POINT ( 'NONE',  ( 42.80287614962790599, -14.05525454449571932, 69.29271901957253021 ) ) ;
#12495 = AXIS2_PLACEMENT_3D ( 'NONE', #13454, #17395, #37409 ) ;
#12496 = VECTOR ( 'NONE', #27027, 1000.000000000000000 ) ;
#12497 = CYLINDRICAL_SURFACE ( 'NONE', #18511, 116.0000000000000000 ) ;
#12498 = AXIS2_PLACEMENT_3D ( 'NONE', #19045, #12686, #35994 ) ;
#12499 = ORIENTED_EDGE ( 'NONE', *, *, #30016, .T. ) ;
#12500 = CYLINDRICAL_SURFACE ( 'NONE', #37710, 47.49900000000000233 ) ;
#12501 = DIRECTION ( 'NONE',  ( 0.000000000000000000, -0.4132121857683850874, 0.9106347728549100129 ) ) ;
#12502 = CARTESIAN_POINT ( 'NONE',  ( 17.99999999999999645, 0.04937522221168735848, -31.94951095880158576 ) ) ;
#12503 = EDGE_CURVE ( 'NONE', #267, #23227, #7269, .T. ) ;
#12505 = DIRECTION ( 'NONE',  ( 1.000000000000000000, 0.000000000000000000, 0.000000000000000000 ) ) ;
#12504 = DIRECTION ( 'NONE',  ( 0.000000000000000000, 0.000000000000000000, 1.000000000000000000 ) ) ;
#12506 = EDGE_CURVE ( 'NONE', #37859, #15611, #37950, .T. ) ;
#12507 = EDGE_CURVE ( 'NONE', #32964, #27433, #31304, .T. ) ;
#12508 = DIRECTION ( 'NONE',  ( -1.000000000000000000, 0.000000000000000000, 0.000000000000000000 ) ) ;
#12509 = ORIENTED_EDGE ( 'NONE', *, *, #3598, .F. ) ;
#12510 =( LENGTH_UNIT ( ) NAMED_UNIT ( * ) SI_UNIT ( .MILLI., .METRE. ) );
#12511 = ADVANCED_FACE ( 'NONE', ( #38678 ), #29520, .F. ) ;
#12512 = CARTESIAN_POINT ( 'NONE',  ( 13.36968668718156295, 31.00000000000000355, 23.13838826010315941 ) ) ;
#12513 = ORIENTED_EDGE ( 'NONE', *, *, #28624, .T. ) ;
#12514 = CARTESIAN_POINT ( 'NONE',  ( 0.000000000000000000, -116.4607004671430417, 30.94182036827165660 ) ) ;
#12515 = LINE ( 'NONE', #19289, #14918 ) ;
#12516 = ORIENTED_EDGE ( 'NONE', *, *, #1595, .F. ) ;
#12517 = ADVANCED_FACE ( 'NONE', ( #6166 ), #28890, .F. ) ;
#12518 = CARTESIAN_POINT ( 'NONE',  ( 8.699408683037360035, 40.00000000000000000, 25.59862650653646909 ) ) ;
#12519 = CARTESIAN_POINT ( 'NONE',  ( 2.319640971205140900, 40.00000000000000000, -34.59922639972668890 ) ) ;
#12520 = ORIENTED_EDGE ( 'NONE', *, *, #41967, .F. ) ;
#12521 = ORIENTED_EDGE ( 'NONE', *, *, #29656, .F. ) ;
#12522 = DIRECTION ( 'NONE',  ( -1.000000000000000000, -0.000000000000000000, 0.000000000000000000 ) ) ;
#12523 = CARTESIAN_POINT ( 'NONE',  ( 0.000000000000000000, -113.8630351447207119, 22.16324045874372572 ) ) ;
#12524 = CIRCLE ( 'NONE', #9732, 120.5010000000000190 ) ;
#12525 = FILL_AREA_STYLE_COLOUR ( '', #3862 ) ;
#12526 = FACE_OUTER_BOUND ( 'NONE', #21227, .T. ) ;
#12527 = AXIS2_PLACEMENT_3D ( 'NONE', #29477, #26207, #22965 ) ;
#12528 = LINE ( 'NONE', #39304, #9904 ) ;
#12529 = DIRECTION ( 'NONE',  ( -1.000000000000000000, 0.000000000000000000, -0.000000000000000000 ) ) ;
#12530 = ORIENTED_EDGE ( 'NONE', *, *, #41605, .F. ) ;
#12531 = CARTESIAN_POINT ( 'NONE',  ( 18.00000000000000355, -9.744342220503087404, -46.48873837489808380 ) ) ;
#12532 = VERTEX_POINT ( 'NONE', #2031 ) ;
#12533 = DIRECTION ( 'NONE',  ( 0.000000000000000000, -0.05322217484216513333, -0.9985826956767627216 ) ) ;
#12534 = CARTESIAN_POINT ( 'NONE',  ( 17.99999999999999645, 0.000000000000000000, 0.000000000000000000 ) ) ;
#12535 = CARTESIAN_POINT ( 'NONE',  ( 0.000000000000000000, -28.62203781742993414, -14.19692359621484989 ) ) ;
#12536 = DIRECTION ( 'NONE',  ( -1.000000000000000000, -0.000000000000000000, -0.000000000000000000 ) ) ;
#12537 = ORIENTED_EDGE ( 'NONE', *, *, #1976, .T. ) ;
#12538 = CARTESIAN_POINT ( 'NONE',  ( -72.39171112334068425, 40.00000000000000711, -55.52881859171880308 ) ) ;
#12539 = ADVANCED_FACE ( 'NONE', ( #29110 ), #15799, .F. ) ;
#12540 = ORIENTED_EDGE ( 'NONE', *, *, #32529, .F. ) ;
#12541 = EDGE_CURVE ( 'NONE', #10180, #4179, #16227, .T. ) ;
#12542 = DIRECTION ( 'NONE',  ( 0.000000000000000000, -0.6382441836448110584, -0.7698339834299138262 ) ) ;
#12543 = ORIENTED_EDGE ( 'NONE', *, *, #29791, .T. ) ;
#12545 = VERTEX_POINT ( 'NONE', #12949 ) ;
#12544 = CARTESIAN_POINT ( 'NONE',  ( 17.99999999999999645, -23.87611429743648017, -20.54551452399645939 ) ) ;
#12546 = CARTESIAN_POINT ( 'NONE',  ( -35.18788409414197815, 31.00000000000000355, -40.25400722681192178 ) ) ;
#12547 = VERTEX_POINT ( 'NONE', #22366 ) ;
#12548 = DIRECTION ( 'NONE',  ( 0.000000000000000000, -0.3140767120219362107, -0.9493976084683853900 ) ) ;
#12549 = CARTESIAN_POINT ( 'NONE',  ( -4.000000000000000000, 2.309401076758498483, -5.000000000000000000 ) ) ;
#12550 = VERTEX_POINT ( 'NONE', #32356 ) ;
#12551 = CARTESIAN_POINT ( 'NONE',  ( 47.76959191294547935, 40.00000000000000000, 62.44753968353898443 ) ) ;
#12552 = CIRCLE ( 'NONE', #20929, 36.00000000000000000 ) ;
#12553 = CIRCLE ( 'NONE', #42476, 116.0000000000000000 ) ;
#12554 = AXIS2_PLACEMENT_3D ( 'NONE', #25604, #35779, #19057 ) ;
#12556 = DIRECTION ( 'NONE',  ( -1.000000000000000000, 0.000000000000000000, 0.000000000000000000 ) ) ;
#12555 = DIRECTION ( 'NONE',  ( 3.009274222672345096E-17, 1.000000000000000000, -2.455023325076454960E-18 ) ) ;
#12557 = EDGE_CURVE ( 'NONE', #2034, #6009, #33747, .T. ) ;
#12558 = CYLINDRICAL_SURFACE ( 'NONE', #12280, 59.00000000000000000 ) ;
#12559 = ORIENTED_EDGE ( 'NONE', *, *, #34461, .F. ) ;
#12560 = DIRECTION ( 'NONE',  ( 0.000000000000000000, 1.000000000000000000, 0.000000000000000000 ) ) ;
#12561 = ORIENTED_EDGE ( 'NONE', *, *, #3461, .T. ) ;
#12562 = EDGE_CURVE ( 'NONE', #42396, #40004, #24040, .T. ) ;
#12563 = CARTESIAN_POINT ( 'NONE',  ( 17.99999999999999645, 29.03409033315599075, -12.21509719675360373 ) ) ;
#12564 = DIRECTION ( 'NONE',  ( -1.000000000000000000, 0.000000000000000000, -0.000000000000000000 ) ) ;
#12565 = CARTESIAN_POINT ( 'NONE',  ( -10.77850749866037816, 31.00000000000000355, -81.75987728344749428 ) ) ;
#12567 = DIRECTION ( 'NONE',  ( 0.000000000000000000, 0.000000000000000000, 1.000000000000000000 ) ) ;
#12566 = DIRECTION ( 'NONE',  ( 0.000000000000000000, 0.4610925014493267304, -0.8873520750565710991 ) ) ;
#12568 = ORIENTED_EDGE ( 'NONE', *, *, #1189, .T. ) ;
#12569 = ADVANCED_FACE ( 'NONE', ( #5943 ), #19090, .F. ) ;
#12570 = ADVANCED_FACE ( 'NONE', ( #12526 ), #35196, .F. ) ;
#12571 = ORIENTED_EDGE ( 'NONE', *, *, #37208, .T. ) ;
#12572 = DIRECTION ( 'NONE',  ( 1.000000000000000000, 0.000000000000000000, 0.000000000000000000 ) ) ;
#12573 = DIRECTION ( 'NONE',  ( -1.000000000000000000, 0.000000000000000000, 0.000000000000000000 ) ) ;
#12574 = CARTESIAN_POINT ( 'NONE',  ( -83.29221842953128885, 31.00000000000000711, -41.19657635674187190 ) ) ;
#12575 = CARTESIAN_POINT ( 'NONE',  ( -12.22491041697691294, 40.00000000000000000, -93.69500887688228374 ) ) ;
#12576 = CARTESIAN_POINT ( 'NONE',  ( 0.000000000000000000, 13.56094713063641599, -50.20060470671725739 ) ) ;
#12577 = ORIENTED_EDGE ( 'NONE', *, *, #28108, .T. ) ;
#12578 = DIRECTION ( 'NONE',  ( 0.000000000000000000, -0.5264321628773447337, -0.8502171357296209875 ) ) ;
#12579 = ORIENTED_EDGE ( 'NONE', *, *, #25580, .T. ) ;
#12580 = CIRCLE ( 'NONE', #22350, 52.00000000000000000 ) ;
#12581 = DIRECTION ( 'NONE',  ( 0.000000000000000000, -0.8993121301712141413, -0.4373073204588656671 ) ) ;
#12582 = AXIS2_PLACEMENT_3D ( 'NONE', #1190, #11913, #8398 ) ;
#12583 = VECTOR ( 'NONE', #14210, 1000.000000000000000 ) ;
#12584 = DIRECTION ( 'NONE',  ( -1.000000000000000000, -0.000000000000000000, 0.000000000000000000 ) ) ;
#12585 = VECTOR ( 'NONE', #22526, 1000.000000000000000 ) ;
#12586 = DIRECTION ( 'NONE',  ( -1.000000000000000000, -0.000000000000000000, -0.000000000000000000 ) ) ;
#12587 = EDGE_LOOP ( 'NONE', ( #32857, #41197, #40039, #24589 ) ) ;
#12588 = FACE_OUTER_BOUND ( 'NONE', #22029, .T. ) ;
#12589 = CARTESIAN_POINT ( 'NONE',  ( 0.000000000000000000, -2.418575551221678666, 120.4767259403368911 ) ) ;
#12590 = CARTESIAN_POINT ( 'NONE',  ( 17.99999999999999645, -3.996885678773838713, 120.4346956066681713 ) ) ;
#12591 = ORIENTED_EDGE ( 'NONE', *, *, #3555, .T. ) ;
#12592 = DIRECTION ( 'NONE',  ( 1.000000000000000000, 0.000000000000000000, 0.000000000000000000 ) ) ;
#12593 = DIRECTION ( 'NONE',  ( -1.000000000000000000, -0.000000000000000000, -0.000000000000000000 ) ) ;
#12595 = ORIENTED_EDGE ( 'NONE', *, *, #16094, .T. ) ;
#12594 = DIRECTION ( 'NONE',  ( 1.000000000000000000, 0.000000000000000000, 0.000000000000000000 ) ) ;
#12596 = ORIENTED_EDGE ( 'NONE', *, *, #3941, .T. ) ;
#12597 = FACE_OUTER_BOUND ( 'NONE', #1343, .T. ) ;
#12598 = CARTESIAN_POINT ( 'NONE',  ( 17.99999999999999645, 0.000000000000000000, 0.000000000000000000 ) ) ;
#12599 = CARTESIAN_POINT ( 'NONE',  ( 2.511863649308039736, 40.00000000000000000, 39.39933062585536305 ) ) ;
#12600 = DIRECTION ( 'NONE',  ( 0.000000000000000000, 0.000000000000000000, 1.000000000000000000 ) ) ;
#12601 = CIRCLE ( 'NONE', #36230, 116.0000000000000000 ) ;
#12602 = CARTESIAN_POINT ( 'NONE',  ( 8.999999999999998224, 0.000000000000000000, 0.000000000000000000 ) ) ;
#12603 = EDGE_CURVE ( 'NONE', #4007, #25961, #12873, .T. ) ;
#12604 = CARTESIAN_POINT ( 'NONE',  ( 0.000000000000000000, 12.43843445475471832, -111.5058645182328405 ) ) ;
#12605 = AXIS2_PLACEMENT_3D ( 'NONE', #23517, #3597, #16969 ) ;
#12606 = ORIENTED_EDGE ( 'NONE', *, *, #33327, .F. ) ;
#12607 = DIRECTION ( 'NONE',  ( 0.000000000000000000, 0.000000000000000000, 1.000000000000000000 ) ) ;
#12608 = EDGE_CURVE ( 'NONE', #42167, #24321, #9360, .T. ) ;
#12609 = ORIENTED_EDGE ( 'NONE', *, *, #9934, .F. ) ;
#12610 = AXIS2_PLACEMENT_3D ( 'NONE', #28337, #21382, #5168 ) ;
#12611 = DIRECTION ( 'NONE',  ( 1.000000000000000000, 0.000000000000000000, 0.000000000000000000 ) ) ;
#12612 = FACE_OUTER_BOUND ( 'NONE', #33682, .T. ) ;
#12613 = CIRCLE ( 'NONE', #18225, 11.00000000000000000 ) ;
#12615 = CARTESIAN_POINT ( 'NONE',  ( 10.63353083439206870, 31.00000000000000355, -31.33693976183458219 ) ) ;
#12614 = AXIS2_PLACEMENT_3D ( 'NONE', #30526, #1024, #33996 ) ;
#12616 = CARTESIAN_POINT ( 'NONE',  ( -4.000000000000000000, 2.309401076758498483, -3.433295621305379353 ) ) ;
#12617 = ORIENTED_EDGE ( 'NONE', *, *, #30840, .F. ) ;
#12618 = AXIS2_PLACEMENT_3D ( 'NONE', #24418, #1885, #27893 ) ;
#12619 = EDGE_CURVE ( 'NONE', #7155, #26591, #6226, .T. ) ;
#12620 = CARTESIAN_POINT ( 'NONE',  ( 12.55910585664918422, 0.7408941433508176022, -1.199999999999999956 ) ) ;
#12621 = CARTESIAN_POINT ( 'NONE',  ( 12.12865573427490062, 31.00000000000000355, -92.11205733446308841 ) ) ;
#12622 = EDGE_CURVE ( 'NONE', #34783, #1751, #8802, .T. ) ;
#12623 = DIRECTION ( 'NONE',  ( 1.000000000000000000, -1.373900992973642066E-15, -3.979293995072266947E-16 ) ) ;
#12624 = ORIENTED_EDGE ( 'NONE', *, *, #20500, .F. ) ;
#12625 = CARTESIAN_POINT ( 'NONE',  ( 57.47007747236072817, 31.00000000000000000, -33.06854485811727784 ) ) ;
#12626 = CARTESIAN_POINT ( 'NONE',  ( 49.67886955981430219, 40.00000000000000000, -43.43868092391004865 ) ) ;
#12627 = LINE ( 'NONE', #36150, #40566 ) ;
#12628 = ORIENTED_EDGE ( 'NONE', *, *, #38502, .T. ) ;
#12629 = CARTESIAN_POINT ( 'NONE',  ( -1.287237434361707233, -3.875615274277397937, -3.430618716626816500 ) ) ;
#12630 = FACE_OUTER_BOUND ( 'NONE', #22026, .T. ) ;
#12631 = CARTESIAN_POINT ( 'NONE',  ( 0.000000000000000000, -48.55277268144396174, 105.3500273609078306 ) ) ;
#12633 = ORIENTED_EDGE ( 'NONE', *, *, #5064, .F. ) ;
#12632 = FACE_OUTER_BOUND ( 'NONE', #20658, .T. ) ;
#12634 = FACE_OUTER_BOUND ( 'NONE', #16127, .T. ) ;
#12635 = CIRCLE ( 'NONE', #2832, 58.99999999999998579 ) ;
#12636 = DIRECTION ( 'NONE',  ( -1.000000000000000000, -0.000000000000000000, -0.000000000000000000 ) ) ;
#12637 = EDGE_CURVE ( 'NONE', #41527, #17401, #32574, .T. ) ;
#12638 = ORIENTED_EDGE ( 'NONE', *, *, #32299, .T. ) ;
#12639 = CARTESIAN_POINT ( 'NONE',  ( 44.85399723358655422, 40.00000000000000000, -58.47732767552992073 ) ) ;
#12640 = CARTESIAN_POINT ( 'NONE',  ( 0.000000000000000000, -41.20225022064620646, -23.63323037071445043 ) ) ;
#12641 = EDGE_CURVE ( 'NONE', #24346, #30476, #37234, .T. ) ;
#12642 = AXIS2_PLACEMENT_3D ( 'NONE', #41612, #31379, #38539 ) ;
#12643 = ORIENTED_EDGE ( 'NONE', *, *, #43009, .F. ) ;
#12644 = CARTESIAN_POINT ( 'NONE',  ( 17.99999999999999645, 11.49545354908979888, -29.80986809967247453 ) ) ;
#12645 = EDGE_CURVE ( 'NONE', #18492, #5647, #16019, .T. ) ;
#12646 = CARTESIAN_POINT ( 'NONE',  ( -10.00000000000000000, 0.000000000000000000, 0.000000000000000000 ) ) ;
#12647 = VECTOR ( 'NONE', #18101, 1000.000000000000114 ) ;
#12648 = ORIENTED_EDGE ( 'NONE', *, *, #16941, .T. ) ;
#12649 = ORIENTED_EDGE ( 'NONE', *, *, #25986, .T. ) ;
#12650 = DIRECTION ( 'NONE',  ( -1.000000000000000000, -0.000000000000000000, -0.000000000000000000 ) ) ;
#12651 = ORIENTED_EDGE ( 'NONE', *, *, #22498, .F. ) ;
#12652 = AXIS2_PLACEMENT_3D ( 'NONE', #2584, #42513, #25966 ) ;
#12653 = FACE_OUTER_BOUND ( 'NONE', #38252, .T. ) ;
#12654 = FACE_OUTER_BOUND ( 'NONE', #12719, .T. ) ;
#12655 = CARTESIAN_POINT ( 'NONE',  ( 0.000000000000000000, 0.000000000000000000, 0.000000000000000000 ) ) ;
#12656 = DIRECTION ( 'NONE',  ( 0.000000000000000000, 0.000000000000000000, -1.000000000000000000 ) ) ;
#12657 = EDGE_LOOP ( 'NONE', ( #41920, #30224 ) ) ;
#12658 = CARTESIAN_POINT ( 'NONE',  ( 6.600000000000008527, 6.938893903907228378E-15, 0.000000000000000000 ) ) ;
#12659 = EDGE_CURVE ( 'NONE', #32464, #42401, #35848, .T. ) ;
#12660 = VERTEX_POINT ( 'NONE', #14408 ) ;
#12661 = CARTESIAN_POINT ( 'NONE',  ( 8.999999999999998224, 48.55277268144470071, -105.3500273609075180 ) ) ;
#12662 = ORIENTED_EDGE ( 'NONE', *, *, #36778, .T. ) ;
#12663 = CARTESIAN_POINT ( 'NONE',  ( 9.000000000000001776, 5.492704054966705662, 115.8698847939556344 ) ) ;
#12664 = CARTESIAN_POINT ( 'NONE',  ( 17.99999999999999645, 66.49630760163724119, -90.36876423295917959 ) ) ;
#12665 = EDGE_CURVE ( 'NONE', #32420, #13665, #2391, .T. ) ;
#12666 = CONTEXT_DEPENDENT_SHAPE_REPRESENTATION ( #4994, #3247 ) ;
#12667 = EDGE_CURVE ( 'NONE', #22227, #36282, #10780, .T. ) ;
#12668 = CARTESIAN_POINT ( 'NONE',  ( 22.90854556226710415, -40.05525454449572464, -74.83297477053821467 ) ) ;
#12669 = CARTESIAN_POINT ( 'NONE',  ( 53.64558601427197004, 31.00000000000000355, 14.36188897069615500 ) ) ;
#12670 = CIRCLE ( 'NONE', #18283, 19.11697999999999809 ) ;
#12671 = CARTESIAN_POINT ( 'NONE',  ( 17.99999999999999645, -29.68570942776479527, 10.53307442156924267 ) ) ;
#12672 = AXIS2_PLACEMENT_3D ( 'NONE', #32023, #2101, #28559 ) ;
#12673 = ADVANCED_FACE ( 'NONE', ( #34443 ), #621, .T. ) ;
#12674 = ORIENTED_EDGE ( 'NONE', *, *, #39347, .F. ) ;
#12675 = CARTESIAN_POINT ( 'NONE',  ( -24.93870012978733541, 31.00000000000000355, -21.94074674037795702 ) ) ;
#12676 = AXIS2_PLACEMENT_3D ( 'NONE', #32947, #13133, #26425 ) ;
#12677 = CARTESIAN_POINT ( 'NONE',  ( 65.10416666562252885, 39.99999999999999289, 4.254240043327690124 ) ) ;
#12678 = VECTOR ( 'NONE', #16706, 1000.000000000000000 ) ;
#12679 = CARTESIAN_POINT ( 'NONE',  ( -10.00000000000000000, 0.000000000000000000, 0.000000000000000000 ) ) ;
#12680 = DIRECTION ( 'NONE',  ( 1.000000000000000000, 0.000000000000000000, 0.000000000000000000 ) ) ;
#12681 = CARTESIAN_POINT ( 'NONE',  ( 17.99999999999999645, -63.24564713401861837, 102.5693868539693341 ) ) ;
#12682 = CYLINDRICAL_SURFACE ( 'NONE', #20269, 120.5010000000000190 ) ;
#12683 = PRODUCT_DEFINITION_SHAPE ( 'NONE', 'NONE',  #10989 ) ;
#12684 = ORIENTED_EDGE ( 'NONE', *, *, #8849, .F. ) ;
#12685 = CARTESIAN_POINT ( 'NONE',  ( -49.89583333467011528, 40.00000000000000000, 3.272492339034415831 ) ) ;
#12686 = DIRECTION ( 'NONE',  ( -1.000000000000000000, -0.000000000000000000, -0.000000000000000000 ) ) ;
#12687 = CARTESIAN_POINT ( 'NONE',  ( 0.000000000000000000, 0.000000000000000000, 0.000000000000000000 ) ) ;
#12688 = ORIENTED_EDGE ( 'NONE', *, *, #4911, .F. ) ;
#12689 = ADVANCED_FACE ( 'NONE', ( #43019 ), #27489, .F. ) ;
#12690 = FACE_OUTER_BOUND ( 'NONE', #26569, .T. ) ;
#12691 = CARTESIAN_POINT ( 'NONE',  ( 0.000000000000000000, 46.90537658765331486, 2.727856614654470491 ) ) ;
#12692 = PRODUCT_RELATED_PRODUCT_CATEGORY ( 'part', '', ( #35641 ) ) ;
#12693 = ORIENTED_EDGE ( 'NONE', *, *, #42792, .F. ) ;
#12694 = DIRECTION ( 'NONE',  ( -3.009274222672345096E-17, -1.000000000000000000, 2.455023325076454960E-18 ) ) ;
#12695 = ORIENTED_EDGE ( 'NONE', *, *, #9272, .F. ) ;
#12696 = CIRCLE ( 'NONE', #14113, 31.49900000000000588 ) ;
#12697 = ORIENTED_EDGE ( 'NONE', *, *, #8131, .F. ) ;
#12698 = DIRECTION ( 'NONE',  ( 1.000000000000000000, -1.373900992973642263E-15, -4.095874873834148624E-16 ) ) ;
#12699 = AXIS2_PLACEMENT_3D ( 'NONE', #3947, #41035, #7886 ) ;
#12700 = CARTESIAN_POINT ( 'NONE',  ( -77.35014290652780744, 31.00000000000000711, 26.14598721591455543 ) ) ;
#12701 = ORIENTED_EDGE ( 'NONE', *, *, #12937, .F. ) ;
#12702 = CARTESIAN_POINT ( 'NONE',  ( 9.000000000000001776, -51.93417535146742381, 2.615612846549007831 ) ) ;
#12703 = CIRCLE ( 'NONE', #26651, 59.00000000000000000 ) ;
#12704 = CARTESIAN_POINT ( 'NONE',  ( 17.99999999999999645, -115.9387338813861987, 3.769613505535687636 ) ) ;
#12705 = DIRECTION ( 'NONE',  ( 1.000000000000000000, -0.000000000000000000, -0.000000000000000000 ) ) ;
#12706 = ORIENTED_EDGE ( 'NONE', *, *, #34165, .F. ) ;
#12707 = CYLINDRICAL_SURFACE ( 'NONE', #11998, 20.00000000000000711 ) ;
#12708 = EDGE_CURVE ( 'NONE', #23222, #9027, #4113, .T. ) ;
#12709 = ADVANCED_FACE ( 'NONE', ( #32987 ), #14631, .T. ) ;
#12710 = CARTESIAN_POINT ( 'NONE',  ( -44.52253807734693680, 40.00000000000000000, 90.03212995793734308 ) ) ;
#12711 = VECTOR ( 'NONE', #15567, 1000.000000000000000 ) ;
#12712 = CARTESIAN_POINT ( 'NONE',  ( 17.99999999999999645, 84.09610293794170843, -74.27057253242929846 ) ) ;
#12714 = DIRECTION ( 'NONE',  ( -1.000000000000000000, 0.000000000000000000, 0.000000000000000000 ) ) ;
#12713 = DIRECTION ( 'NONE',  ( -1.000000000000000000, 0.000000000000000000, 0.000000000000000000 ) ) ;
#12715 = DIRECTION ( 'NONE',  ( 3.009274222672345096E-17, 1.000000000000000000, -2.455023325076455345E-18 ) ) ;
#12716 = ORIENTED_EDGE ( 'NONE', *, *, #12463, .F. ) ;
#12717 = ADVANCED_FACE ( 'NONE', ( #7618 ), #27940, .F. ) ;
#12718 = CARTESIAN_POINT ( 'NONE',  ( -4.233603722440171246, 31.00000000000000355, -32.08218167604271542 ) ) ;
#12719 = EDGE_LOOP ( 'NONE', ( #18036, #36578, #4476, #21310 ) ) ;
#12720 = CARTESIAN_POINT ( 'NONE',  ( 17.99999999999999645, 45.89132998248050654, 102.3829004574631512 ) ) ;
#12721 = EDGE_CURVE ( 'NONE', #21131, #4060, #6374, .T. ) ;
#12722 = DIRECTION ( 'NONE',  ( -1.000000000000000000, -0.000000000000000000, -0.000000000000000000 ) ) ;
#12723 = ORIENTED_EDGE ( 'NONE', *, *, #16653, .F. ) ;
#12724 = LINE ( 'NONE', #26890, #18824 ) ;
#12725 = CARTESIAN_POINT ( 'NONE',  ( 28.66079171547214699, 40.00000000000000000, 21.97938003711830035 ) ) ;
#12726 = CARTESIAN_POINT ( 'NONE',  ( -28.46928290085317670, 40.00000000000000000, -16.49637127829624106 ) ) ;
#12727 = AXIS2_PLACEMENT_3D ( 'NONE', #32281, #22295, #2590 ) ;
#12728 = ORIENTED_EDGE ( 'NONE', *, *, #41786, .T. ) ;
#12729 = ORIENTED_EDGE ( 'NONE', *, *, #15991, .F. ) ;
#12730 = FACE_OUTER_BOUND ( 'NONE', #31693, .T. ) ;
#12731 = CARTESIAN_POINT ( 'NONE',  ( 0.000000000000000000, 0.000000000000000000, 0.000000000000000000 ) ) ;
#12732 = VECTOR ( 'NONE', #31371, 1000.000000000000114 ) ;
#12733 = CARTESIAN_POINT ( 'NONE',  ( 17.99999999999999645, 0.000000000000000000, 0.000000000000000000 ) ) ;
#12734 = DIRECTION ( 'NONE',  ( -1.000000000000000000, 0.000000000000000000, -0.000000000000000000 ) ) ;
#12735 = CYLINDRICAL_SURFACE ( 'NONE', #27186, 116.0000000000000000 ) ;
#12736 = ORIENTED_EDGE ( 'NONE', *, *, #1893, .F. ) ;
#12737 = DIRECTION ( 'NONE',  ( -1.000000000000000000, 0.000000000000000000, 0.000000000000000000 ) ) ;
#12738 = ORIENTED_EDGE ( 'NONE', *, *, #12799, .F. ) ;
#12739 = CARTESIAN_POINT ( 'NONE',  ( 17.99999999999999645, 91.51415974874679193, -64.91094698989203948 ) ) ;
#12740 = AXIS2_PLACEMENT_3D ( 'NONE', #18178, #14878, #41676 ) ;
#12741 = DIRECTION ( 'NONE',  ( 0.000000000000000000, 1.246648735278247733E-14, -1.000000000000000000 ) ) ;
#12742 = EDGE_CURVE ( 'NONE', #40198, #14608, #16364, .T. ) ;
#12743 = EDGE_CURVE ( 'NONE', #42396, #35643, #17481, .T. ) ;
#12744 = FACE_BOUND ( 'NONE', #3363, .T. ) ;
#12745 = EDGE_CURVE ( 'NONE', #27398, #29194, #33217, .T. ) ;
#12746 = EDGE_CURVE ( 'NONE', #42617, #4705, #40708, .T. ) ;
#12747 = CARTESIAN_POINT ( 'NONE',  ( 0.000000000000000000, -11.41303419184897017, -111.6154788735837116 ) ) ;
#12748 = ORIENTED_EDGE ( 'NONE', *, *, #13060, .F. ) ;
#12749 = CARTESIAN_POINT ( 'NONE',  ( 17.99999999999999645, 0.000000000000000000, 0.000000000000000000 ) ) ;
#12750 = VERTEX_POINT ( 'NONE', #37282 ) ;
#12751 = CARTESIAN_POINT ( 'NONE',  ( 0.000000000000000000, 150.5000000000000284, 9.999999999999998224 ) ) ;
#12752 = EDGE_LOOP ( 'NONE', ( #41506, #803, #25128, #25578 ) ) ;
#12754 = ORIENTED_EDGE ( 'NONE', *, *, #30179, .T. ) ;
#12753 = CARTESIAN_POINT ( 'NONE',  ( 0.000000000000000000, 0.000000000000000000, 0.000000000000000000 ) ) ;
#12755 = CARTESIAN_POINT ( 'NONE',  ( -13.93478910046839125, 31.00000000000000355, -52.37520058406987999 ) ) ;
#12756 = ORIENTED_EDGE ( 'NONE', *, *, #24944, .T. ) ;
#12757 = DIRECTION ( 'NONE',  ( -1.000000000000000000, -0.000000000000000000, -0.000000000000000000 ) ) ;
#12758 = ORIENTED_EDGE ( 'NONE', *, *, #10115, .F. ) ;
#12759 = FACE_OUTER_BOUND ( 'NONE', #12365, .T. ) ;
#12760 = ORIENTED_EDGE ( 'NONE', *, *, #42319, .F. ) ;
#12761 = CIRCLE ( 'NONE', #26672, 59.00000000000000000 ) ;
#12762 = CARTESIAN_POINT ( 'NONE',  ( -9.228224334387265415, 40.00000000000000000, 69.24269282083176336 ) ) ;
#12764 = DIRECTION ( 'NONE',  ( 1.000000000000000000, -1.373900992973642263E-15, -4.525365589504737954E-16 ) ) ;
#12763 = DIRECTION ( 'NONE',  ( 0.000000000000000000, 0.000000000000000000, 1.000000000000000000 ) ) ;
#12765 = CIRCLE ( 'NONE', #5086, 12.59999999999999964 ) ;
#12766 = CARTESIAN_POINT ( 'NONE',  ( 0.000000000000000000, -23.87611429743648017, -20.54551452399645939 ) ) ;
#12767 = VERTEX_POINT ( 'NONE', #36253 ) ;
#12768 = CARTESIAN_POINT ( 'NONE',  ( -79.93711883401132923, -2.055254544495720648, -145.8806300090334673 ) ) ;
#12769 = PRESENTATION_LAYER_ASSIGNMENT (  '', '', ( #30978 ) ) ;
#12770 = EDGE_LOOP ( 'NONE', ( #20260, #22256, #7872, #28700 ) ) ;
#12771 = SURFACE_SIDE_STYLE ('',( #42831 ) ) ;
#12772 = CIRCLE ( 'NONE', #9261, 51.99999999999999289 ) ;
#12773 = CARTESIAN_POINT ( 'NONE',  ( -5.560781378645573980, 0.000000000000000000, -4.000000000000000000 ) ) ;
#12774 = CARTESIAN_POINT ( 'NONE',  ( 18.00000000000000355, -0.6505223195686603566, 51.99593080916757515 ) ) ;
#12775 = CARTESIAN_POINT ( 'NONE',  ( -10.16518460146908787, 31.00000000000000355, 77.20874865269769316 ) ) ;
#12777 = DIRECTION ( 'NONE',  ( 3.009274222672345096E-17, 1.000000000000000000, -2.455023325076454960E-18 ) ) ;
#12776 = DIRECTION ( 'NONE',  ( -0.000000000000000000, 0.000000000000000000, 1.000000000000000000 ) ) ;
#12778 = ORIENTED_EDGE ( 'NONE', *, *, #16862, .F. ) ;
#12779 = DIRECTION ( 'NONE',  ( -1.000000000000000000, -0.000000000000000000, 0.000000000000000000 ) ) ;
#12780 = EDGE_LOOP ( 'NONE', ( #23191, #30773, #4738, #39717 ) ) ;
#12781 = LINE ( 'NONE', #39149, #26911 ) ;
#12782 = CARTESIAN_POINT ( 'NONE',  ( 0.000000000000000000, 47.58001226230686598, -110.7096808509478763 ) ) ;
#12783 = CARTESIAN_POINT ( 'NONE',  ( -68.52217190868857699, 31.00000000000000711, 59.94826526066079708 ) ) ;
#12784 = CARTESIAN_POINT ( 'NONE',  ( -61.42214656771047743, 40.00000000000000711, 79.86467493626639680 ) ) ;
#12785 = CARTESIAN_POINT ( 'NONE',  ( 17.99999999999999645, 23.87611429743662939, 20.54551452399628531 ) ) ;
#12786 = AXIS2_PLACEMENT_3D ( 'NONE', #27865, #41119, #21775 ) ;
#12787 = CARTESIAN_POINT ( 'NONE',  ( 0.000000000000000000, 0.000000000000000000, 0.000000000000000000 ) ) ;
#12788 = ORIENTED_EDGE ( 'NONE', *, *, #7719, .T. ) ;
#12789 = DIRECTION ( 'NONE',  ( 0.000000000000000000, -0.4610925014493142959, -0.8873520750565775383 ) ) ;
#12790 = ORIENTED_EDGE ( 'NONE', *, *, #22086, .F. ) ;
#12791 = CARTESIAN_POINT ( 'NONE',  ( 8.999999999999998224, 78.18175027177548486, -85.69488855492920720 ) ) ;
#12792 = CARTESIAN_POINT ( 'NONE',  ( 0.000000000000000000, 32.00046193115148441, 34.40241257139697950 ) ) ;
#12793 = EDGE_CURVE ( 'NONE', #34589, #18324, #24460, .T. ) ;
#12794 = EDGE_CURVE ( 'NONE', #11355, #10144, #40015, .T. ) ;
#12795 = CARTESIAN_POINT ( 'NONE',  ( 0.000000000000000000, -39.78933988720132220, 24.98727647984988920 ) ) ;
#12796 = ORIENTED_EDGE ( 'NONE', *, *, #37251, .T. ) ;
#12797 = DIRECTION ( 'NONE',  ( -1.058513553088275437E-16, -1.000000000000000000, 8.813324511995299047E-17 ) ) ;
#12798 = DIRECTION ( 'NONE',  ( -1.000000000000000000, 0.000000000000000000, 0.000000000000000000 ) ) ;
#12799 = EDGE_CURVE ( 'NONE', #6443, #22892, #3758, .T. ) ;
#12800 = DIRECTION ( 'NONE',  ( 0.000000000000000000, 0.000000000000000000, 1.000000000000000000 ) ) ;
#12802 = ORIENTED_EDGE ( 'NONE', *, *, #17041, .F. ) ;
#12801 = DIRECTION ( 'NONE',  ( 1.000000000000000000, 0.000000000000000000, 0.000000000000000000 ) ) ;
#12803 = CARTESIAN_POINT ( 'NONE',  ( -22.00000000000000000, 31.00000000000000355, 0.000000000000000000 ) ) ;
#12804 = LINE ( 'NONE', #35686, #33635 ) ;
#12805 = CIRCLE ( 'NONE', #6514, 120.5010000000000190 ) ;
#12807 = ORIENTED_EDGE ( 'NONE', *, *, #14034, .T. ) ;
#12806 = DIRECTION ( 'NONE',  ( -1.000000000000000000, 0.000000000000000000, 0.000000000000000000 ) ) ;
#12808 = ORIENTED_EDGE ( 'NONE', *, *, #12324, .T. ) ;
#12809 = DIRECTION ( 'NONE',  ( -1.000000000000000000, 0.000000000000000000, 0.000000000000000000 ) ) ;
#12810 = CARTESIAN_POINT ( 'NONE',  ( 17.99999999999999645, 94.83915810436401728, 59.94836581341619564 ) ) ;
#12811 = CARTESIAN_POINT ( 'NONE',  ( -19.32876798325328949, 40.00000000000000000, -39.37500834187648735 ) ) ;
#12812 = DIRECTION ( 'NONE',  ( -1.000000000000000000, 0.000000000000000000, 0.000000000000000000 ) ) ;
#12813 = EDGE_CURVE ( 'NONE', #31610, #26339, #25447, .T. ) ;
#12814 = AXIS2_PLACEMENT_3D ( 'NONE', #8571, #21930, #4211 ) ;
#12815 = CARTESIAN_POINT ( 'NONE',  ( 17.99999999999999645, 0.000000000000000000, 0.000000000000000000 ) ) ;
#12816 = AXIS2_PLACEMENT_3D ( 'NONE', #42192, #35451, #42415 ) ;
#12817 = CARTESIAN_POINT ( 'NONE',  ( 0.000000000000000000, 88.56657216608614647, 68.87840567545953263 ) ) ;
#12818 = ORIENTED_EDGE ( 'NONE', *, *, #19851, .T. ) ;
#12819 = CARTESIAN_POINT ( 'NONE',  ( 9.000000000000001776, -107.1354928292866759, -44.47455650398174498 ) ) ;
#12820 = ORIENTED_EDGE ( 'NONE', *, *, #41596, .T. ) ;
#12821 = VECTOR ( 'NONE', #37288, 1000.000000000000000 ) ;
#12822 = PLANE ( 'NONE',  #11358 ) ;
#12823 = CARTESIAN_POINT ( 'NONE',  ( 17.99999999999999645, -95.38615066513943930, -59.07414607872924250 ) ) ;
#12824 = CARTESIAN_POINT ( 'NONE',  ( 45.10416666515585860, 31.00000000000000355, 2.945243104263102651 ) ) ;
#12825 =( LENGTH_UNIT ( ) NAMED_UNIT ( * ) SI_UNIT ( .MILLI., .METRE. ) );
#12826 = ORIENTED_EDGE ( 'NONE', *, *, #12425, .F. ) ;
#12827 = COLOUR_RGB ( '', 0.09019608, 0.27058824, 0.51372549) ;
#12828 = LINE ( 'NONE', #42473, #41406 ) ;
#12829 = CARTESIAN_POINT ( 'NONE',  ( -72.39171112334068425, 31.00000000000000711, -55.52881859171880308 ) ) ;
#12830 = AXIS2_PLACEMENT_3D ( 'NONE', #6416, #7659, #23470 ) ;
#12831 = CARTESIAN_POINT ( 'NONE',  ( 17.99999999999999645, 25.46650492921924425, -19.29328419707757547 ) ) ;
#12832 = ORIENTED_EDGE ( 'NONE', *, *, #20695, .F. ) ;
#12833 = CARTESIAN_POINT ( 'NONE',  ( 4.437437895627577511, 31.00000000000000355, 69.40004907510417809 ) ) ;
#12834 = CARTESIAN_POINT ( 'NONE',  ( -72.09351246578157202, 40.00000000000000711, -4.825959690424619808 ) ) ;
#12835 = CARTESIAN_POINT ( 'NONE',  ( -89.22528799552154055, 40.00000000000000711, 43.99828826784794700 ) ) ;
#12836 = AXIS2_PLACEMENT_3D ( 'NONE', #25553, #38176, #21649 ) ;
#12837 = VERTEX_POINT ( 'NONE', #40983 ) ;
#12838 = PRESENTATION_STYLE_ASSIGNMENT (( #33102 ) ) ;
#12839 = CIRCLE ( 'NONE', #26785, 59.00000000000000000 ) ;
#12840 = DIRECTION ( 'NONE',  ( 0.000000000000000000, 0.000000000000000000, 1.000000000000000000 ) ) ;
#12841 = LINE ( 'NONE', #39424, #3103 ) ;
#12842 = CIRCLE ( 'NONE', #7240, 12.55910585664918422 ) ;
#12844 = ORIENTED_EDGE ( 'NONE', *, *, #18769, .T. ) ;
#12843 = LINE ( 'NONE', #26153, #15098 ) ;
#12845 = ADVANCED_FACE ( 'NONE', ( #4330 ), #11134, .T. ) ;
#12846 = DIRECTION ( 'NONE',  ( 0.000000000000000000, 0.000000000000000000, 1.000000000000000000 ) ) ;
#12847 = CARTESIAN_POINT ( 'NONE',  ( 9.000000000000001776, -50.95304419620816816, -10.38206564895716255 ) ) ;
#12848 = PRODUCT_RELATED_PRODUCT_CATEGORY ( 'part', '', ( #33245 ) ) ;
#12849 = AXIS2_PLACEMENT_3D ( 'NONE', #39208, #12215, #22919 ) ;
#12850 = CARTESIAN_POINT ( 'NONE',  ( 73.00591898829820536, 39.99999999999999289, 19.54754034098114701 ) ) ;
#12851 = CARTESIAN_POINT ( 'NONE',  ( 17.99999999999999645, -31.17727234463771424, 111.7317219465818852 ) ) ;
#12852 = ORIENTED_EDGE ( 'NONE', *, *, #35086, .F. ) ;
#12853 = DIRECTION ( 'NONE',  ( -1.000000000000000000, 0.000000000000000000, 0.000000000000000000 ) ) ;
#12854 = DIRECTION ( 'NONE',  ( -1.000000000000000000, -0.000000000000000000, -0.000000000000000000 ) ) ;
#12855 = EDGE_CURVE ( 'NONE', #22539, #25336, #38632, .T. ) ;
#12856 = ORIENTED_EDGE ( 'NONE', *, *, #7578, .F. ) ;
#12857 = DIRECTION ( 'NONE',  ( 0.000000000000000000, -0.05322217484218560307, 0.9985826956767616114 ) ) ;
#12858 = EDGE_CURVE ( 'NONE', #6740, #7094, #35882, .T. ) ;
#12859 = CIRCLE ( 'NONE', #39973, 59.00000000000000711 ) ;
#12860 = ORIENTED_EDGE ( 'NONE', *, *, #26210, .F. ) ;
#12861 = CARTESIAN_POINT ( 'NONE',  ( 8.999999999999998224, 94.52951811191651643, -67.23221107124801676 ) ) ;
#12862 =( GEOMETRIC_REPRESENTATION_CONTEXT ( 3 ) GLOBAL_UNCERTAINTY_ASSIGNED_CONTEXT ( ( #21763 ) ) GLOBAL_UNIT_ASSIGNED_CONTEXT ( ( #33766, #17238, #3444 ) ) REPRESENTATION_CONTEXT ( 'NONE', 'WORKASPACE' ) );
#12863 = ORIENTED_EDGE ( 'NONE', *, *, #2238, .F. ) ;
#12864 = CARTESIAN_POINT ( 'NONE',  ( -10.00000000000000000, 0.000000000000000000, 0.000000000000000000 ) ) ;
#12865 = DIRECTION ( 'NONE',  ( -1.000000000000000000, 0.000000000000000000, 0.000000000000000000 ) ) ;
#12866 = ADVANCED_FACE ( 'NONE', ( #21845 ), #35093, .T. ) ;
#12867 = CARTESIAN_POINT ( 'NONE',  ( 17.99999999999999645, 0.5156212287279957618, 112.1962860721878172 ) ) ;
#12868 = DIRECTION ( 'NONE',  ( 1.000000000000000000, 0.000000000000000000, 0.000000000000000000 ) ) ;
#12870 = ORIENTED_EDGE ( 'NONE', *, *, #2587, .T. ) ;
#12869 = AXIS2_PLACEMENT_3D ( 'NONE', #35276, #28112, #1459 ) ;
#12871 = DIRECTION ( 'NONE',  ( 0.000000000000000000, 0.000000000000000000, 1.000000000000000000 ) ) ;
#12872 = ORIENTED_EDGE ( 'NONE', *, *, #18939, .T. ) ;
#12873 = CIRCLE ( 'NONE', #14982, 120.5010000000000332 ) ;
#12874 = FACE_OUTER_BOUND ( 'NONE', #30093, .T. ) ;
#12875 = AXIS2_PLACEMENT_3D ( 'NONE', #9642, #39505, #22343 ) ;
#12876 = ORIENTED_EDGE ( 'NONE', *, *, #35849, .T. ) ;
#12877 = DIRECTION ( 'NONE',  ( 1.000000000000000000, 0.000000000000000000, 0.000000000000000000 ) ) ;
#12878 = CIRCLE ( 'NONE', #15663, 116.0000000000000000 ) ;
#12879 = CARTESIAN_POINT ( 'NONE',  ( 42.80287614962796994, -12.05525454449572464, 69.29271901957280022 ) ) ;
#12880 = CARTESIAN_POINT ( 'NONE',  ( 4.211140560182196957, -2.431303136016555122, -3.745885042887436622 ) ) ;
#12881 = CARTESIAN_POINT ( 'NONE',  ( -27.38011802910879311, 31.00000000000000355, -55.51905197969063011 ) ) ;
#12882 = ADVANCED_FACE ( 'NONE', ( #5206 ), #15065, .T. ) ;
#12883 = DIRECTION ( 'NONE',  ( 0.000000000000000000, -1.224646799147343346E-16, 1.000000000000000000 ) ) ;
#12884 = VERTEX_POINT ( 'NONE', #1497 ) ;
#12885 = CARTESIAN_POINT ( 'NONE',  ( 10.06970066534735331, 31.00000000000000355, 37.84957806120349488 ) ) ;
#12886 = CARTESIAN_POINT ( 'NONE',  ( 66.75446398494719347, 39.99999999999999289, -32.91950810868348043 ) ) ;
#12887 = B_SPLINE_CURVE_WITH_KNOTS ( 'NONE', 3,
 ( #40991, #31848, #1934, #25325, #11138, #31418 ),
 .UNSPECIFIED., .F., .F.,
 ( 4, 2, 4 ),
 ( 0.002365888236227967761, 0.003551327329835077609, 0.004736766423442186590 ),
 .UNSPECIFIED. ) ;
#12888 = CIRCLE ( 'NONE', #6598, 20.00000000000000355 ) ;
#12889 = DIRECTION ( 'NONE',  ( -1.000000000000000000, -0.000000000000000000, 0.000000000000000000 ) ) ;
#12890 = CARTESIAN_POINT ( 'NONE',  ( 0.000000000000000000, -9.744342220503083851, -46.48873837489806959 ) ) ;
#12891 = CIRCLE ( 'NONE', #18508, 31.49900000000000233 ) ;
#12892 = FACE_OUTER_BOUND ( 'NONE', #22229, .T. ) ;
#12893 = AXIS2_PLACEMENT_3D ( 'NONE', #42456, #25915, #9299 ) ;
#12894 = CARTESIAN_POINT ( 'NONE',  ( 0.000000000000000000, 0.000000000000000000, 0.000000000000000000 ) ) ;
#12895 = ADVANCED_FACE ( 'NONE', ( #12002 ), #38791, .F. ) ;
#12896 = VECTOR ( 'NONE', #19221, 1000.000000000000000 ) ;
#12897 = ORIENTED_EDGE ( 'NONE', *, *, #15831, .T. ) ;
#12898 = CARTESIAN_POINT ( 'NONE',  ( 38.32544124395173668, 40.00000000000000000, -22.13982348525413002 ) ) ;
#12899 = PLANE ( 'NONE',  #40362 ) ;
#12900 = CYLINDRICAL_SURFACE ( 'NONE', #18032, 1.999999999999988010 ) ;
#12901 = AXIS2_PLACEMENT_3D ( 'NONE', #26577, #19416, #36581 ) ;
#12902 = ORIENTED_EDGE ( 'NONE', *, *, #42000, .T. ) ;
#12903 = CIRCLE ( 'NONE', #338, 59.00000000000000000 ) ;
#12904 = CARTESIAN_POINT ( 'NONE',  ( 0.000000000000000000, 11.46872990052444408, -45.56340405422433548 ) ) ;
#12905 = CARTESIAN_POINT ( 'NONE',  ( 2.500000000000000000, -1.178949249685218748, -2.041999999999998039 ) ) ;
#12906 = COLOUR_RGB ( '', 0.08235294, 0.09019608, 0.10196078) ;
#12907 = VERTEX_POINT ( 'NONE', #18570 ) ;
#12908 = FACE_OUTER_BOUND ( 'NONE', #40572, .T. ) ;
#12909 = VERTEX_POINT ( 'NONE', #2333 ) ;
#12910 = EDGE_CURVE ( 'NONE', #17463, #24263, #30339, .T. ) ;
#12911 = AXIS2_PLACEMENT_3D ( 'NONE', #77, #290, #13446 ) ;
#12912 = ORIENTED_EDGE ( 'NONE', *, *, #33282, .F. ) ;
#12913 = FACE_OUTER_BOUND ( 'NONE', #41, .T. ) ;
#12914 = CARTESIAN_POINT ( 'NONE',  ( -12.22491041698737746, 31.00000000000000355, -93.69500887688226953 ) ) ;
#12915 = ORIENTED_EDGE ( 'NONE', *, *, #1711, .F. ) ;
#12916 = DIRECTION ( 'NONE',  ( -1.000000000000000000, 0.000000000000000000, -0.000000000000000000 ) ) ;
#12917 = DIRECTION ( 'NONE',  ( 0.000000000000000000, 0.000000000000000000, -1.000000000000000000 ) ) ;
#12918 = CARTESIAN_POINT ( 'NONE',  ( -105.9879088449591933, 40.00000000000000000, -0.3807199291576673361 ) ) ;
#12919 = ORIENTED_EDGE ( 'NONE', *, *, #25649, .F. ) ;
#12920 = DIRECTION ( 'NONE',  ( -1.000000000000000000, 0.000000000000000000, -0.000000000000000000 ) ) ;
#12921 = LINE ( 'NONE', #9408, #40086 ) ;
#12922 = CIRCLE ( 'NONE', #25502, 59.00000000000000711 ) ;
#12924 = DIRECTION ( 'NONE',  ( 1.000000000000000000, 0.000000000000000000, 0.000000000000000000 ) ) ;
#12923 = FACE_OUTER_BOUND ( 'NONE', #8708, .T. ) ;
#12925 = CIRCLE ( 'NONE', #37284, 116.0000000000000000 ) ;
#12926 = AXIS2_PLACEMENT_3D ( 'NONE', #35980, #9369, #22725 ) ;
#12927 = CARTESIAN_POINT ( 'NONE',  ( 17.99999999999999645, 34.74871106919619024, 106.6808302961373158 ) ) ;
#12928 = CIRCLE ( 'NONE', #38692, 2.500000000000002665 ) ;
#12929 = EDGE_LOOP ( 'NONE', ( #22386, #20886, #38682, #12169 ) ) ;
#12930 = AXIS2_PLACEMENT_3D ( 'NONE', #37768, #34936, #5046 ) ;
#12931 = CARTESIAN_POINT ( 'NONE',  ( -25.30796725786148826, 31.00000000000000355, 14.62256337265529815 ) ) ;
#12932 = EDGE_CURVE ( 'NONE', #16471, #27833, #15721, .T. ) ;
#12933 = ORIENTED_EDGE ( 'NONE', *, *, #36715, .T. ) ;
#12934 = CIRCLE ( 'NONE', #18550, 120.5010000000000190 ) ;
#12935 = FACE_OUTER_BOUND ( 'NONE', #22332, .T. ) ;
#12936 = VECTOR ( 'NONE', #26133, 1000.000000000000000 ) ;
#12937 = EDGE_CURVE ( 'NONE', #19812, #5593, #24070, .T. ) ;
#12938 = DIRECTION ( 'NONE',  ( 0.000000000000000000, 0.000000000000000000, 1.000000000000000000 ) ) ;
#12939 = VERTEX_POINT ( 'NONE', #22050 ) ;
#12940 = AXIS2_PLACEMENT_3D ( 'NONE', #20002, #20218, #279 ) ;
#12941 = DIRECTION ( 'NONE',  ( 0.000000000000000000, 0.000000000000000000, 1.000000000000000000 ) ) ;
#12942 = CARTESIAN_POINT ( 'NONE',  ( 27.23661496637203427, 40.00000000000000000, 23.88131275951389654 ) ) ;
#12943 = CARTESIAN_POINT ( 'NONE',  ( -2.659806967433698599, 40.00000000000000000, 39.59793253468611596 ) ) ;
#12944 = CIRCLE ( 'NONE', #29670, 51.99999999999999289 ) ;
#12945 = EDGE_LOOP ( 'NONE', ( #22197, #9627, #42341, #32984 ) ) ;
#12946 = EDGE_LOOP ( 'NONE', ( #11453, #14481, #17138, #33898 ) ) ;
#12947 = CARTESIAN_POINT ( 'NONE',  ( 0.000000000000000000, 13.85708833599968770, 45.43276465116669982 ) ) ;
#12948 = CARTESIAN_POINT ( 'NONE',  ( 17.99999999999999645, -30.01658535635190361, -108.1077105353201233 ) ) ;
#12949 = CARTESIAN_POINT ( 'NONE',  ( 0.000000000000000000, 64.58410930313523579, 101.7319213743684685 ) ) ;
#12950 = CARTESIAN_POINT ( 'NONE',  ( 0.000000000000000000, 0.000000000000000000, 0.000000000000000000 ) ) ;
#12951 = ADVANCED_FACE ( 'NONE', ( #41643 ), #8482, .T. ) ;
#12952 = DIRECTION ( 'NONE',  ( 1.000000000000000000, 0.000000000000000000, 0.000000000000000000 ) ) ;
#12953 = ORIENTED_EDGE ( 'NONE', *, *, #19772, .T. ) ;
#12954 = CYLINDRICAL_SURFACE ( 'NONE', #2644, 13.59999999999999787 ) ;
#12955 = ORIENTED_EDGE ( 'NONE', *, *, #758, .F. ) ;
#12956 = DIRECTION ( 'NONE',  ( -1.000000000000000000, 0.000000000000000000, -0.000000000000000000 ) ) ;
#12957 = CYLINDRICAL_SURFACE ( 'NONE', #42308, 116.0000000000000000 ) ;
#12958 = CIRCLE ( 'NONE', #18571, 2.500000000000000444 ) ;
#12959 = CARTESIAN_POINT ( 'NONE',  ( 0.000000000000000000, 83.58328028049660929, 80.43528614701352808 ) ) ;
#12960 = CARTESIAN_POINT ( 'NONE',  ( 17.99999999999999645, 109.4038418350910433, -50.51029986767441926 ) ) ;
#12961 = VERTEX_POINT ( 'NONE', #15496 ) ;
#12962 = LINE ( 'NONE', #16456, #25699 ) ;
#12963 = CIRCLE ( 'NONE', #17153, 1.000000000000000444 ) ;
#12964 = ORIENTED_EDGE ( 'NONE', *, *, #30286, .T. ) ;
#12965 = CIRCLE ( 'NONE', #20679, 120.5010000000000332 ) ;
#12966 = CARTESIAN_POINT ( 'NONE',  ( 17.99999999999999645, 78.75547124681369837, 91.20343606297029737 ) ) ;
#12967 = AXIS2_PLACEMENT_3D ( 'NONE', #10625, #30705, #20266 ) ;
#12968 = EDGE_CURVE ( 'NONE', #38008, #22806, #42052, .T. ) ;
#12969 = VERTEX_POINT ( 'NONE', #4786 ) ;
#12970 = AXIS2_PLACEMENT_3D ( 'NONE', #5080, #18672, #19075 ) ;
#12972 = EDGE_LOOP ( 'NONE', ( #23326, #32143, #10142, #8669 ) ) ;
#12971 = CYLINDRICAL_SURFACE ( 'NONE', #2025, 58.99999999999999289 ) ;
#12973 = CARTESIAN_POINT ( 'NONE',  ( 32.82854187708761629, 31.00000000000000355, -56.64543409046200395 ) ) ;
#12974 = VECTOR ( 'NONE', #3343, 1000.000000000000000 ) ;
#12975 = EDGE_CURVE ( 'NONE', #1383, #42412, #29627, .T. ) ;
#12976 = ORIENTED_EDGE ( 'NONE', *, *, #34228, .F. ) ;
#12977 = CARTESIAN_POINT ( 'NONE',  ( 18.00000000000000355, 44.75336757549799671, -14.30704879393557150 ) ) ;
#12978 = AXIS2_PLACEMENT_3D ( 'NONE', #34778, #39895, #39100 ) ;
#12979 = AXIS2_PLACEMENT_3D ( 'NONE', #13739, #11479, #25043 ) ;
#12980 = ORIENTED_EDGE ( 'NONE', *, *, #2820, .F. ) ;
#12981 = CYLINDRICAL_SURFACE ( 'NONE', #766, 59.00000000000000000 ) ;
#12982 = AXIS2_PLACEMENT_3D ( 'NONE', #40828, #14252, #34508 ) ;
#12983 = ORIENTED_EDGE ( 'NONE', *, *, #36129, .T. ) ;
#12984 = CARTESIAN_POINT ( 'NONE',  ( -5.321195512787074478, 40.00000000000000000, 79.59297073838583003 ) ) ;
#12986 = CARTESIAN_POINT ( 'NONE',  ( 17.99999999999999645, 103.4151313792879421, -61.85306461934305844 ) ) ;
#12985 = DIRECTION ( 'NONE',  ( 0.000000000000000000, 0.000000000000000000, 1.000000000000000000 ) ) ;
#12987 = CARTESIAN_POINT ( 'NONE',  ( 17.99999999999999645, -84.09610293794118263, 74.27057253242982426 ) ) ;
#12988 = ORIENTED_EDGE ( 'NONE', *, *, #10355, .T. ) ;
#12989 = DIRECTION ( 'NONE',  ( 1.000000000000000000, -0.000000000000000000, -0.000000000000000000 ) ) ;
#12990 = ORIENTED_EDGE ( 'NONE', *, *, #6027, .F. ) ;
#12991 = LINE ( 'NONE', #4365, #9305 ) ;
#12992 = CARTESIAN_POINT ( 'NONE',  ( 17.99999999999999645, -15.21076497709792008, 119.5371223922154797 ) ) ;
#12993 = EDGE_CURVE ( 'NONE', #39732, #41661, #36566, .T. ) ;
#12994 = CARTESIAN_POINT ( 'NONE',  ( -76.41092972884307244, 31.00000000000000711, -25.93877460596726436 ) ) ;
#12995 = EDGE_CURVE ( 'NONE', #28903, #31744, #42141, .T. ) ;
#12997 = DIRECTION ( 'NONE',  ( -1.000000000000000000, 0.000000000000000000, 0.000000000000000000 ) ) ;
#12996 = CARTESIAN_POINT ( 'NONE',  ( 18.00000000000000355, 39.78933988720115877, 24.98727647985016276 ) ) ;
#12998 = CIRCLE ( 'NONE', #29743, 59.00000000000000000 ) ;
#12999 = ORIENTED_EDGE ( 'NONE', *, *, #16121, .F. ) ;
#13000 = ADVANCED_FACE ( 'NONE', ( #34672 ), #11560, .T. ) ;
#13001 = EDGE_CURVE ( 'NONE', #9453, #15674, #34883, .T. ) ;
#13002 = AXIS2_PLACEMENT_3D ( 'NONE', #27047, #155, #40315 ) ;
#13003 = AXIS2_PLACEMENT_3D ( 'NONE', #10162, #25922, #6040 ) ;
#13004 = AXIS2_PLACEMENT_3D ( 'NONE', #9914, #29805, #30218 ) ;
#13005 = FILL_AREA_STYLE ('',( #38725 ) ) ;
#13006 = ORIENTED_EDGE ( 'NONE', *, *, #38335, .F. ) ;
#13007 = DIRECTION ( 'NONE',  ( 0.000000000000000000, -0.5264321628773627193, 0.8502171357296098853 ) ) ;
#13008 = LINE ( 'NONE', #27380, #34588 ) ;
#13009 = CARTESIAN_POINT ( 'NONE',  ( 91.58570893733639195, 31.00000000000000000, -30.97307622143650363 ) ) ;
#13011 = CARTESIAN_POINT ( 'NONE',  ( -24.28006566513952791, 40.00000000000000000, -91.10131089348455191 ) ) ;
#13010 = VECTOR ( 'NONE', #40055, 1000.000000000000000 ) ;
#13012 = DIRECTION ( 'NONE',  ( -1.000000000000000000, 0.000000000000000000, -0.000000000000000000 ) ) ;
#13013 = AXIS2_PLACEMENT_3D ( 'NONE', #33550, #33762, #16797 ) ;
#13014 = DIRECTION ( 'NONE',  ( 0.000000000000000000, 0.3681245526846786964, -0.9297764858882511252 ) ) ;
#13015 = ORIENTED_EDGE ( 'NONE', *, *, #42187, .F. ) ;
#13016 = CYLINDRICAL_SURFACE ( 'NONE', #20819, 116.0000000000000000 ) ;
#13017 = ORIENTED_EDGE ( 'NONE', *, *, #15042, .F. ) ;
#13018 = CARTESIAN_POINT ( 'NONE',  ( 6.199999999999997513, 6.971071669133949438E-15, 0.000000000000000000 ) ) ;
#13019 = CIRCLE ( 'NONE', #38776, 15.99999999999998934 ) ;
#13020 = CARTESIAN_POINT ( 'NONE',  ( 0.000000000000000000, 103.5682682299982673, 43.14958040911701431 ) ) ;
#13021 = DIRECTION ( 'NONE',  ( 0.000000000000000000, 0.000000000000000000, 1.000000000000000000 ) ) ;
#13022 = EDGE_LOOP ( 'NONE', ( #5357, #33640, #30252, #17903 ) ) ;
#13023 = CARTESIAN_POINT ( 'NONE',  ( 8.999999999999998224, -13.57797752207946829, 33.34124362422470256 ) ) ;
#13024 = DIRECTION ( 'NONE',  ( 0.000000000000000000, 0.000000000000000000, 1.000000000000000000 ) ) ;
#13025 = ADVANCED_FACE ( 'NONE', ( #33104 ), #43132, .T. ) ;
#13026 = CARTESIAN_POINT ( 'NONE',  ( 18.00000000000000355, 0.000000000000000000, 0.000000000000000000 ) ) ;
#13028 = EDGE_LOOP ( 'NONE', ( #6266, #21650, #42059, #16947 ) ) ;
#13027 = DIRECTION ( 'NONE',  ( 0.000000000000000000, 0.000000000000000000, 1.000000000000000000 ) ) ;
#13029 = CARTESIAN_POINT ( 'NONE',  ( 23.62253089228586234, 31.00000000000000355, -11.62353008834390167 ) ) ;
#13030 = EDGE_CURVE ( 'NONE', #31004, #21207, #8031, .T. ) ;
#13031 = DIRECTION ( 'NONE',  ( 0.000000000000000000, 0.000000000000000000, 1.000000000000000000 ) ) ;
#13032 = AXIS2_PLACEMENT_3D ( 'NONE', #19573, #42862, #35885 ) ;
#13033 = VECTOR ( 'NONE', #4761, 1000.000000000000000 ) ;
#13034 = VECTOR ( 'NONE', #18888, 1000.000000000000000 ) ;
#13036 = EDGE_LOOP ( 'NONE', ( #42920, #27363, #28515, #10383 ) ) ;
#13035 = CARTESIAN_POINT ( 'NONE',  ( 18.00000000000000355, 0.000000000000000000, 0.000000000000000000 ) ) ;
#13037 = VERTEX_POINT ( 'NONE', #29638 ) ;
#13038 = DIRECTION ( 'NONE',  ( -3.996523416598930318E-16, 2.658563593772947863E-15, 1.000000000000000000 ) ) ;
#13039 = DIRECTION ( 'NONE',  ( 1.000000000000000000, 0.000000000000000000, 0.000000000000000000 ) ) ;
#13040 = CARTESIAN_POINT ( 'NONE',  ( -25.29816761084670063, 40.00000000000000000, 43.63644233508315295 ) ) ;
#13041 = AXIS2_PLACEMENT_3D ( 'NONE', #16381, #7127, #2602 ) ;
#13042 = FACE_OUTER_BOUND ( 'NONE', #11752, .T. ) ;
#13043 = AXIS2_PLACEMENT_3D ( 'NONE', #11290, #37876, #25477 ) ;
#13044 = DIRECTION ( 'NONE',  ( 1.000000000000000000, 0.000000000000000000, 0.000000000000000000 ) ) ;
#13045 = CARTESIAN_POINT ( 'NONE',  ( 0.000000000000000000, 21.56073507908678977, -23.57770962728541875 ) ) ;
#13046 = EDGE_LOOP ( 'NONE', ( #217, #14477, #25209, #38857 ) ) ;
#13047 = CARTESIAN_POINT ( 'NONE',  ( 0.000000000000000000, -28.35267316522799419, 22.18391138608698299 ) ) ;
#13049 = EDGE_LOOP ( 'NONE', ( #9883, #34702, #13747, #10822 ) ) ;
#13048 = AXIS2_PLACEMENT_3D ( 'NONE', #2782, #13518, #26394 ) ;
#13050 = FACE_OUTER_BOUND ( 'NONE', #41764, .T. ) ;
#13051 = CARTESIAN_POINT ( 'NONE',  ( 17.99999999999999645, 0.000000000000000000, 0.000000000000000000 ) ) ;
#13052 = AXIS2_PLACEMENT_3D ( 'NONE', #14766, #14983, #17834 ) ;
#13053 = CARTESIAN_POINT ( 'NONE',  ( 13.85568741775851542, 31.00000000000000355, -40.82620080729295609 ) ) ;
#13054 = EDGE_CURVE ( 'NONE', #21840, #9577, #19896, .T. ) ;
#13055 = DIRECTION ( 'NONE',  ( -1.000000000000000000, -0.000000000000000000, -0.000000000000000000 ) ) ;
#13056 = ORIENTED_EDGE ( 'NONE', *, *, #29273, .F. ) ;
#13057 = EDGE_CURVE ( 'NONE', #16464, #13205, #40045, .T. ) ;
#13058 = EDGE_CURVE ( 'NONE', #8904, #8390, #26139, .T. ) ;
#13059 = PRODUCT_DEFINITION_SHAPE ( 'NONE', 'NONE',  #43183 ) ;
#13060 = EDGE_CURVE ( 'NONE', #1786, #39040, #41433, .T. ) ;
#13061 = DIRECTION ( 'NONE',  ( 1.000000000000000000, 0.000000000000000000, 0.000000000000000000 ) ) ;
#13062 = CARTESIAN_POINT ( 'NONE',  ( -68.67288961433401084, 31.00000000000000711, -60.22678404055071155 ) ) ;
#13063 = DIRECTION ( 'NONE',  ( 1.000000000000000000, 0.000000000000000000, 0.000000000000000000 ) ) ;
#13064 = VERTEX_POINT ( 'NONE', #3189 ) ;
#13065 = CARTESIAN_POINT ( 'NONE',  ( 30.38134496340387969, 31.00000000000000355, 61.85720693093856681 ) ) ;
#13066 = CARTESIAN_POINT ( 'NONE',  ( 63.11376326756305843, 39.99999999999999289, -21.32174659672108774 ) ) ;
#13067 = EDGE_CURVE ( 'NONE', #42608, #39242, #22675, .T. ) ;
#13068 = CARTESIAN_POINT ( 'NONE',  ( 95.10416666600561086, 39.99999999999999289, 6.217735451873073416 ) ) ;
#13069 = AXIS2_PLACEMENT_3D ( 'NONE', #32531, #35774, #9185 ) ;
#13070 = VERTEX_POINT ( 'NONE', #12631 ) ;
#13071 = CIRCLE ( 'NONE', #26330, 51.99999999999999289 ) ;
#13072 = CARTESIAN_POINT ( 'NONE',  ( 9.000000000000001776, -5.492704054967489924, 115.8698847939556202 ) ) ;
#13073 = AXIS2_PLACEMENT_3D ( 'NONE', #36867, #11142, #25708 ) ;
#13074 = EDGE_CURVE ( 'NONE', #5452, #2577, #15013, .T. ) ;
#13075 = DIRECTION ( 'NONE',  ( -1.000000000000000000, 0.000000000000000000, -0.000000000000000000 ) ) ;
#13076 = CARTESIAN_POINT ( 'NONE',  ( 17.99999999999999645, 0.000000000000000000, 0.000000000000000000 ) ) ;
#13077 = AXIS2_PLACEMENT_3D ( 'NONE', #18465, #1828, #38266 ) ;
#13079 = VERTEX_POINT ( 'NONE', #3416 ) ;
#13078 = CARTESIAN_POINT ( 'NONE',  ( 0.000000000000000000, 0.000000000000000000, 0.000000000000000000 ) ) ;
#13080 = DIRECTION ( 'NONE',  ( -1.000000000000000000, 0.000000000000000000, 0.000000000000000000 ) ) ;
#13081 = EDGE_LOOP ( 'NONE', ( #11018, #1309, #23240, #38075 ) ) ;
#13082 = CARTESIAN_POINT ( 'NONE',  ( 1.598609366639573350E-14, -1.063425437509180407E-13, -40.00000000000000000 ) ) ;
#13083 = CARTESIAN_POINT ( 'NONE',  ( -4.745113895469965648, 40.00000000000000000, -72.39583333427917466 ) ) ;
#13084 = CARTESIAN_POINT ( 'NONE',  ( 18.00000000000000355, -46.11014828289851408, 9.022736828080542892 ) ) ;
#13085 = ORIENTED_EDGE ( 'NONE', *, *, #31372, .F. ) ;
#13086 = CARTESIAN_POINT ( 'NONE',  ( 0.000000000000000000, 0.000000000000000000, 0.000000000000000000 ) ) ;
#13087 = DIRECTION ( 'NONE',  ( 0.000000000000000000, -0.9048270524660235736, 0.4257792915650641108 ) ) ;
#13088 = EDGE_LOOP ( 'NONE', ( #14142, #29102, #18898, #42818 ) ) ;
#13089 = VERTEX_POINT ( 'NONE', #16786 ) ;
#13090 = CARTESIAN_POINT ( 'NONE',  ( 0.000000000000000000, -3.996885678772176043, -120.4346956066682424 ) ) ;
#13091 = ORIENTED_EDGE ( 'NONE', *, *, #13893, .F. ) ;
#13092 = DIRECTION ( 'NONE',  ( 1.000000000000000000, 0.000000000000000000, 0.000000000000000000 ) ) ;
#13093 = CARTESIAN_POINT ( 'NONE',  ( 0.000000000000000000, 111.7974656912331426, -9.465682155094398809 ) ) ;
#13094 = AXIS2_PLACEMENT_3D ( 'NONE', #3081, #36473, #40180 ) ;
#13095 = DIRECTION ( 'NONE',  ( 0.000000000000000000, 0.8747630845319623871, -0.4845508703326482647 ) ) ;
#13096 = DIRECTION ( 'NONE',  ( 0.000000000000000000, 0.000000000000000000, 1.000000000000000000 ) ) ;
#13097 = ORIENTED_EDGE ( 'NONE', *, *, #8092, .T. ) ;
#13098 = AXIS2_PLACEMENT_3D ( 'NONE', #23804, #37929, #7833 ) ;
#13099 = LINE ( 'NONE', #26400, #2818 ) ;
#13100 = AXIS2_PLACEMENT_3D ( 'NONE', #4051, #14572, #20920 ) ;
#13101 = ORIENTED_EDGE ( 'NONE', *, *, #21305, .T. ) ;
#13102 = CIRCLE ( 'NONE', #43012, 13.60000000000000142 ) ;
#13103 = AXIS2_PLACEMENT_3D ( 'NONE', #35620, #15591, #38902 ) ;
#13104 = DIRECTION ( 'NONE',  ( 1.000000000000000000, 1.836909530733573776E-16, 0.000000000000000000 ) ) ;
#13105 = CARTESIAN_POINT ( 'NONE',  ( 17.99999999999999645, 0.000000000000000000, 0.000000000000000000 ) ) ;
#13106 = ORIENTED_EDGE ( 'NONE', *, *, #5706, .T. ) ;
#13107 = LINE ( 'NONE', #23151, #2966 ) ;
#13108 = AXIS2_PLACEMENT_3D ( 'NONE', #13179, #9236, #12741 ) ;
#13109 = ADVANCED_FACE ( 'NONE', ( #39001 ), #32467, .T. ) ;
#13110 = DIRECTION ( 'NONE',  ( -1.000000000000000000, -0.000000000000000000, 0.000000000000000000 ) ) ;
#13111 = CARTESIAN_POINT ( 'NONE',  ( 17.99999999999999645, 0.5156212287294736907, -112.1962860721878315 ) ) ;
#13112 = CARTESIAN_POINT ( 'NONE',  ( 28.01378275134445772, 31.00000000000000355, -56.83506808085938644 ) ) ;
#13113 =( REPRESENTATION_RELATIONSHIP ('NONE','NONE', #330, #40225 ) REPRESENTATION_RELATIONSHIP_WITH_TRANSFORMATION ( #26408 )SHAPE_REPRESENTATION_RELATIONSHIP( ) );
#13114 = AXIS2_PLACEMENT_3D ( 'NONE', #21609, #11767, #18972 ) ;
#13115 = VERTEX_POINT ( 'NONE', #22915 ) ;
#13116 = CARTESIAN_POINT ( 'NONE',  ( -24.64063138600606351, 31.00000000000000355, 18.85097431369995746 ) ) ;
#13117 = CARTESIAN_POINT ( 'NONE',  ( -31.81163009274181519, 40.00000000000000000, -64.50738158386226928 ) ) ;
#13118 = EDGE_CURVE ( 'NONE', #6230, #9181, #25945, .T. ) ;
#13119 = EDGE_CURVE ( 'NONE', #22718, #21350, #9124, .T. ) ;
#13120 = DIRECTION ( 'NONE',  ( -1.000000000000000000, 0.000000000000000000, -0.000000000000000000 ) ) ;
#13121 = AXIS2_PLACEMENT_3D ( 'NONE', #19474, #19049, #42338 ) ;
#13122 = EDGE_CURVE ( 'NONE', #7021, #17035, #29215, .T. ) ;
#13123 = FACE_OUTER_BOUND ( 'NONE', #42144, .T. ) ;
#13124 = LINE ( 'NONE', #16625, #12585 ) ;
#13125 = CIRCLE ( 'NONE', #31247, 18.77999999999999403 ) ;
#13126 = VECTOR ( 'NONE', #41132, 1000.000000000000000 ) ;
#13127 = EDGE_LOOP ( 'NONE', ( #24755, #29755, #26260, #28673 ) ) ;
#13128 = CARTESIAN_POINT ( 'NONE',  ( 44.91824650936478491, 40.00000000000000000, 5.910997147197376123 ) ) ;
#13129 = DIRECTION ( 'NONE',  ( 0.000000000000000000, 0.3140767120219494779, -0.9493976084683810601 ) ) ;
#13130 = DIRECTION ( 'NONE',  ( 1.000000000000000000, 1.836909530733573776E-16, 0.000000000000000000 ) ) ;
#13131 = CIRCLE ( 'NONE', #20100, 59.00000000000000711 ) ;
#13132 = ORIENTED_EDGE ( 'NONE', *, *, #21035, .T. ) ;
#13133 = DIRECTION ( 'NONE',  ( -1.000000000000000000, -0.000000000000000000, 0.000000000000000000 ) ) ;
#13134 = AXIS2_PLACEMENT_3D ( 'NONE', #7184, #20542, #6764 ) ;
#13135 = DIRECTION ( 'NONE',  ( -1.000000000000000000, 0.000000000000000000, 0.000000000000000000 ) ) ;
#13136 = ORIENTED_EDGE ( 'NONE', *, *, #21825, .F. ) ;
#13137 = FACE_OUTER_BOUND ( 'NONE', #7570, .T. ) ;
#13138 = ORIENTED_EDGE ( 'NONE', *, *, #14876, .T. ) ;
#13139 = ORIENTED_EDGE ( 'NONE', *, *, #34277, .T. ) ;
#13140 = DIRECTION ( 'NONE',  ( -0.000000000000000000, -0.000000000000000000, -1.000000000000000000 ) ) ;
#13141 = CARTESIAN_POINT ( 'NONE',  ( -82.08563009789774867, 31.00000000000000711, 40.34115885382633593 ) ) ;
#13142 = ORIENTED_EDGE ( 'NONE', *, *, #2625, .T. ) ;
#13143 = FACE_OUTER_BOUND ( 'NONE', #26535, .T. ) ;
#13144 = DIRECTION ( 'NONE',  ( 0.000000000000000000, 0.000000000000000000, 1.000000000000000000 ) ) ;
#13145 = PLANE ( 'NONE',  #41491 ) ;
#13146 = ORIENTED_EDGE ( 'NONE', *, *, #33609, .T. ) ;
#13147 = DIRECTION ( 'NONE',  ( -3.996523416598930318E-16, 2.658563593772947863E-15, 1.000000000000000000 ) ) ;
#13148 = DIRECTION ( 'NONE',  ( -1.000000000000000000, -0.000000000000000000, -0.000000000000000000 ) ) ;
#13149 = VECTOR ( 'NONE', #36215, 1000.000000000000000 ) ;
#13150 = VECTOR ( 'NONE', #9983, 1000.000000000000000 ) ;
#13152 = CARTESIAN_POINT ( 'NONE',  ( 18.00000000000000355, 2.123073309835184386, 47.45152853935334747 ) ) ;
#13151 = CARTESIAN_POINT ( 'NONE',  ( 18.00000000000000355, 46.87740477351712798, 3.172455868806036694 ) ) ;
#13153 = DIRECTION ( 'NONE',  ( -1.000000000000000000, -0.000000000000000000, -0.000000000000000000 ) ) ;
#13154 = VECTOR ( 'NONE', #32786, 1000.000000000000114 ) ;
#13155 = EDGE_CURVE ( 'NONE', #23465, #20981, #35179, .T. ) ;
#13156 = ORIENTED_EDGE ( 'NONE', *, *, #13850, .F. ) ;
#13157 = CARTESIAN_POINT ( 'NONE',  ( 25.50046184691807483, 31.00000000000000355, -22.37655979312362931 ) ) ;
#13158 = AXIS2_PLACEMENT_3D ( 'NONE', #23013, #17, #26261 ) ;
#13159 = EDGE_LOOP ( 'NONE', ( #10998, #41970, #23044, #24480 ) ) ;
#13160 = CARTESIAN_POINT ( 'NONE',  ( 17.99999999999999645, -45.89132998248120288, 102.3829004574628385 ) ) ;
#13161 = DIRECTION ( 'NONE',  ( -3.009274222672345096E-17, -1.000000000000000000, 2.455023325076455345E-18 ) ) ;
#13162 = VERTEX_POINT ( 'NONE', #42487 ) ;
#13163 = CARTESIAN_POINT ( 'NONE',  ( 2.500000000000000000, 2.357898499370431722, -2.818925648462311528E-15 ) ) ;
#13164 = CARTESIAN_POINT ( 'NONE',  ( 34.28525303991722240, 40.00000000000000000, 9.176237600273646322 ) ) ;
#13165 = CARTESIAN_POINT ( 'NONE',  ( 12.64472494877221997, 40.00000000000000000, 47.53373494968590762 ) ) ;
#13166 = ADVANCED_FACE ( 'NONE', ( #9331, #19622 ), #22687, .F. ) ;
#13167 = ORIENTED_EDGE ( 'NONE', *, *, #13118, .T. ) ;
#13168 = ORIENTED_EDGE ( 'NONE', *, *, #13246, .T. ) ;
#13169 = SURFACE_SIDE_STYLE ('',( #23214 ) ) ;
#13170 = EDGE_CURVE ( 'NONE', #16404, #26405, #12841, .T. ) ;
#13171 = DIRECTION ( 'NONE',  ( -1.000000000000000000, -0.000000000000000000, -0.000000000000000000 ) ) ;
#13172 = CARTESIAN_POINT ( 'NONE',  ( 18.00000000000000355, 0.000000000000000000, 0.000000000000000000 ) ) ;
#13173 = CARTESIAN_POINT ( 'NONE',  ( 50.00005079999999680, 0.000000000000000000, 0.000000000000000000 ) ) ;
#13174 = CARTESIAN_POINT ( 'NONE',  ( 17.99999999999999645, 115.6826031496112392, 8.575274253897841703 ) ) ;
#13175 = ORIENTED_EDGE ( 'NONE', *, *, #15891, .F. ) ;
#13176 = CARTESIAN_POINT ( 'NONE',  ( 17.99999999999999645, 0.000000000000000000, 0.000000000000000000 ) ) ;
#13177 = VERTEX_POINT ( 'NONE', #36155 ) ;
#13178 = CARTESIAN_POINT ( 'NONE',  ( -105.9879088449591933, 31.00000000000000355, -0.3807199291576673361 ) ) ;
#13179 = CARTESIAN_POINT ( 'NONE',  ( 0.000000000000000000, -57.40245293794601622, -96.40140491896693220 ) ) ;
#13180 = ORIENTED_EDGE ( 'NONE', *, *, #36768, .T. ) ;
#13181 = CIRCLE ( 'NONE', #25083, 120.5010000000000190 ) ;
#13182 = CIRCLE ( 'NONE', #15989, 51.99999999999999289 ) ;
#13183 = CARTESIAN_POINT ( 'NONE',  ( 0.000000000000000000, -35.78484819117709748, 110.3423972910431701 ) ) ;
#13184 = DIRECTION ( 'NONE',  ( 0.000000000000000000, 0.000000000000000000, 1.000000000000000000 ) ) ;
#13185 = ORIENTED_EDGE ( 'NONE', *, *, #24368, .T. ) ;
#13186 = CARTESIAN_POINT ( 'NONE',  ( 9.000000000000001776, -63.55543939553828636, 97.03971415477303708 ) ) ;
#13187 = ORIENTED_EDGE ( 'NONE', *, *, #23162, .T. ) ;
#13188 = AXIS2_PLACEMENT_3D ( 'NONE', #14959, #25222, #4440 ) ;
#13189 = CARTESIAN_POINT ( 'NONE',  ( 17.99999999999999645, 7.749090474611950441, -30.53094492177204700 ) ) ;
#13190 = EDGE_CURVE ( 'NONE', #17417, #5363, #32892, .T. ) ;
#13191 = ORIENTED_EDGE ( 'NONE', *, *, #25577, .T. ) ;
#13193 = ORIENTED_EDGE ( 'NONE', *, *, #27912, .F. ) ;
#13192 = FACE_OUTER_BOUND ( 'NONE', #25773, .T. ) ;
#13194 = CARTESIAN_POINT ( 'NONE',  ( 64.03668805592332092, 31.00000000000000000, 21.85318084035846198 ) ) ;
#13196 = EDGE_CURVE ( 'NONE', #17370, #19286, #1005, .T. ) ;
#13195 = VERTEX_POINT ( 'NONE', #36368 ) ;
#13197 = CARTESIAN_POINT ( 'NONE',  ( 17.99999999999999645, 78.18175027177430536, 85.69488855493025881 ) ) ;
#13198 = EDGE_LOOP ( 'NONE', ( #23027, #8409 ) ) ;
#13199 = DIRECTION ( 'NONE',  ( 2.731800627175558911E-17, 1.000000000000000000, -3.170996607629411740E-18 ) ) ;
#13200 = EDGE_LOOP ( 'NONE', ( #38517, #39982, #22967, #22113 ) ) ;
#13201 = CARTESIAN_POINT ( 'NONE',  ( 34.80713033128647993, 40.00000000000000000, 70.84796410819511436 ) ) ;
#13203 = DIRECTION ( 'NONE',  ( 3.009274222672345096E-17, 1.000000000000000000, -2.455023325076455345E-18 ) ) ;
#13202 = FACE_OUTER_BOUND ( 'NONE', #26953, .T. ) ;
#13204 = DIRECTION ( 'NONE',  ( -1.000000000000000000, 0.000000000000000000, 0.000000000000000000 ) ) ;
#13205 = VERTEX_POINT ( 'NONE', #4497 ) ;
#13206 = DIRECTION ( 'NONE',  ( 0.000000000000000000, -0.4132121857683668242, -0.9106347728549183396 ) ) ;
#13207 = EDGE_LOOP ( 'NONE', ( #10431, #32261, #5612, #41555 ) ) ;
#13208 = APPLICATION_PROTOCOL_DEFINITION ( 'draft international standard', 'automotive_design', 1998, #14185 ) ;
#13209 = CARTESIAN_POINT ( 'NONE',  ( 9.000000000000001776, -36.06787431788649911, -37.45808914225527531 ) ) ;
#13210 = CARTESIAN_POINT ( 'NONE',  ( -49.69442049507403425, 31.00000000000000355, -64.76435429890716478 ) ) ;
#13211 = AXIS2_PLACEMENT_3D ( 'NONE', #246, #27348, #23877 ) ;
#13213 = CARTESIAN_POINT ( 'NONE',  ( 4.235886605889389145, 2.417314728048528760, -3.751161874094018245 ) ) ;
#13212 = CARTESIAN_POINT ( 'NONE',  ( 0.000000000000000000, -13.56094713063606427, 50.20060470671735686 ) ) ;
#13214 = AXIS2_PLACEMENT_3D ( 'NONE', #10070, #23000, #20161 ) ;
#13215 = ORIENTED_EDGE ( 'NONE', *, *, #11040, .F. ) ;
#13216 = ADVANCED_FACE ( 'NONE', ( #37235 ), #23756, .T. ) ;
#13217 = VECTOR ( 'NONE', #36691, 999.9999999999998863 ) ;
#13218 = FACE_BOUND ( 'NONE', #35571, .T. ) ;
#13219 = EDGE_CURVE ( 'NONE', #2641, #14947, #33781, .T. ) ;
#13220 = B_SPLINE_CURVE_WITH_KNOTS ( 'NONE', 3,
 ( #6399, #20192, #20398, #19746, #33657 ),
 .UNSPECIFIED., .F., .F.,
 ( 4, 1, 4 ),
 ( 0.000000000000000000, 0.002309401076758505356, 0.004618802153517010713 ),
 .UNSPECIFIED. ) ;
#13221 = ORIENTED_EDGE ( 'NONE', *, *, #29461, .T. ) ;
#13222 = DIRECTION ( 'NONE',  ( -1.000000000000000000, -0.000000000000000000, -0.000000000000000000 ) ) ;
#13223 = EDGE_CURVE ( 'NONE', #40725, #25529, #27019, .T. ) ;
#13224 = CARTESIAN_POINT ( 'NONE',  ( 0.000000000000000000, -91.65951123222436081, -71.09524597798180423 ) ) ;
#13225 = CARTESIAN_POINT ( 'NONE',  ( 12.51314706078824912, 31.00000000000000355, -94.07914177284597201 ) ) ;
#13226 = LINE ( 'NONE', #281, #11444 ) ;
#13227 = DIRECTION ( 'NONE',  ( -3.009274222672345712E-17, -1.000000000000000000, 2.455023325076455345E-18 ) ) ;
#13228 = VERTEX_POINT ( 'NONE', #24191 ) ;
#13229 = CARTESIAN_POINT ( 'NONE',  ( 18.00000000000000355, -42.41764978026621691, 20.20639853260276197 ) ) ;
#13230 = ORIENTED_EDGE ( 'NONE', *, *, #4697, .T. ) ;
#13231 = CARTESIAN_POINT ( 'NONE',  ( 18.00000000000000355, 5.871425383721547320, 51.66745943012283249 ) ) ;
#13232 = DIRECTION ( 'NONE',  ( -1.000000000000000000, -0.000000000000000000, -0.000000000000000000 ) ) ;
#13233 = LINE ( 'NONE', #6872, #3797 ) ;
#13234 = EDGE_LOOP ( 'NONE', ( #40513, #13106, #32092, #20828 ) ) ;
#13235 = DIRECTION ( 'NONE',  ( 0.000000000000000000, -0.1253332335643113082, 0.9921147013144769877 ) ) ;
#13236 = DIRECTION ( 'NONE',  ( 0.000000000000000000, 0.000000000000000000, 1.000000000000000000 ) ) ;
#13237 = CARTESIAN_POINT ( 'NONE',  ( 0.000000000000000000, -103.4151313792866489, -61.85306461934516875 ) ) ;
#13238 = CIRCLE ( 'NONE', #26459, 20.00000000000000355 ) ;
#13240 = ORIENTED_EDGE ( 'NONE', *, *, #1645, .T. ) ;
#13239 = PLANE ( 'NONE',  #1998 ) ;
#13241 = EDGE_CURVE ( 'NONE', #19145, #33962, #23954, .T. ) ;
#13242 = CARTESIAN_POINT ( 'NONE',  ( 23.40755275317545880, 31.00000000000000355, 30.61714766194360138 ) ) ;
#13244 = EDGE_CURVE ( 'NONE', #32792, #36933, #34494, .T. ) ;
#13243 = CIRCLE ( 'NONE', #27191, 19.11697999999999809 ) ;
#13245 = CARTESIAN_POINT ( 'NONE',  ( 0.000000000000000000, 95.38615066513983720, 59.07414607872858170 ) ) ;
#13246 = EDGE_CURVE ( 'NONE', #7956, #40062, #33974, .T. ) ;
#13247 = ADVANCED_FACE ( 'NONE', ( #4280 ), #20486, .T. ) ;
#13249 = ORIENTED_EDGE ( 'NONE', *, *, #7384, .F. ) ;
#13248 = CYLINDRICAL_SURFACE ( 'NONE', #17522, 4.500000000000000888 ) ;
#13250 = ORIENTED_EDGE ( 'NONE', *, *, #17227, .T. ) ;
#13251 = DIRECTION ( 'NONE',  ( 1.000000000000000000, -3.035766082959412415E-17, 0.000000000000000000 ) ) ;
#13252 = DIRECTION ( 'NONE',  ( 0.000000000000000000, 0.6783118362696123338, 0.7347741508630707408 ) ) ;
#13253 = CARTESIAN_POINT ( 'NONE',  ( -3.331996295684063636, 40.00000000000000000, 49.59602437329134972 ) ) ;
#13254 = DIRECTION ( 'NONE',  ( -1.000000000000000000, 0.000000000000000000, -0.000000000000000000 ) ) ;
#13255 = CARTESIAN_POINT ( 'NONE',  ( 9.000000000000001776, 47.32430374665962347, -21.55018039121477003 ) ) ;
#13256 = LINE ( 'NONE', #29401, #29041 ) ;
#13257 = ORIENTED_EDGE ( 'NONE', *, *, #21563, .T. ) ;
#13258 = CARTESIAN_POINT ( 'NONE',  ( 0.000000000000000000, -105.3681574666261298, -38.54638589714993202 ) ) ;
#13259 = ORIENTED_EDGE ( 'NONE', *, *, #18776, .T. ) ;
#13260 = DIRECTION ( 'NONE',  ( -1.000000000000000000, -0.000000000000000000, -0.000000000000000000 ) ) ;
#13261 = DIRECTION ( 'NONE',  ( -1.000000000000000000, 0.000000000000000000, 0.000000000000000000 ) ) ;
#13262 = CARTESIAN_POINT ( 'NONE',  ( -40.58740609958903889, 31.00000000000000355, -31.12922691583434798 ) ) ;
#13263 = CARTESIAN_POINT ( 'NONE',  ( 0.000000000000000000, 69.90696807222487053, 98.15042952503540619 ) ) ;
#13264 = ORIENTED_EDGE ( 'NONE', *, *, #8389, .F. ) ;
#13265 = DIRECTION ( 'NONE',  ( -1.000000000000000000, 0.000000000000000000, -0.000000000000000000 ) ) ;
#13266 = EDGE_LOOP ( 'NONE', ( #38159, #12628, #6831, #11277 ) ) ;
#13267 = ADVANCED_FACE ( 'NONE', ( #3835 ), #13495, .T. ) ;
#13268 = CARTESIAN_POINT ( 'NONE',  ( 10.28773449565296083, 40.00000000000000000, -20.88174966193524895 ) ) ;
#13269 = AXIS2_PLACEMENT_3D ( 'NONE', #27721, #10916, #4114 ) ;
#13270 = AXIS2_PLACEMENT_3D ( 'NONE', #31786, #1874, #15237 ) ;
#13271 = ORIENTED_EDGE ( 'NONE', *, *, #36954, .T. ) ;
#13272 = EDGE_CURVE ( 'NONE', #13089, #6694, #30920, .T. ) ;
#13273 = AXIS2_PLACEMENT_3D ( 'NONE', #25137, #35113, #15313 ) ;
#13274 = LINE ( 'NONE', #17427, #17885 ) ;
#13275 = ORIENTED_EDGE ( 'NONE', *, *, #5733, .F. ) ;
#13276 = CARTESIAN_POINT ( 'NONE',  ( -59.63693792270941429, 31.00000000000000711, 15.87187584493272929 ) ) ;
#13277 = CARTESIAN_POINT ( 'NONE',  ( 16.92944795087012722, 40.00000000000000000, -62.81076020707057950 ) ) ;
#13278 = AXIS2_PLACEMENT_3D ( 'NONE', #14194, #37515, #37290 ) ;
#13279 = FACE_OUTER_BOUND ( 'NONE', #40606, .T. ) ;
#13280 = ORIENTED_EDGE ( 'NONE', *, *, #23057, .F. ) ;
#13281 = ORIENTED_EDGE ( 'NONE', *, *, #29366, .T. ) ;
#13282 =( LENGTH_UNIT ( ) NAMED_UNIT ( * ) SI_UNIT ( .MILLI., .METRE. ) );
#13283 = LINE ( 'NONE', #26372, #38880 ) ;
#13284 = CARTESIAN_POINT ( 'NONE',  ( 0.000000000000000000, 0.000000000000000000, 0.000000000000000000 ) ) ;
#13286 = ORIENTED_EDGE ( 'NONE', *, *, #40493, .F. ) ;
#13285 = DIRECTION ( 'NONE',  ( 1.000000000000000000, 1.836909530733573776E-16, 0.000000000000000000 ) ) ;
#13287 = DIRECTION ( 'NONE',  ( -1.000000000000000000, 0.000000000000000000, 0.000000000000000000 ) ) ;
#13288 = ORIENTED_EDGE ( 'NONE', *, *, #5624, .T. ) ;
#13289 = CARTESIAN_POINT ( 'NONE',  ( 17.99999999999999645, -16.77566611177856615, 119.3275660838941832 ) ) ;
#13290 = CARTESIAN_POINT ( 'NONE',  ( -77.37786320076959612, 40.00000000000000711, 44.69160382239309115 ) ) ;
#13291 = DIRECTION ( 'NONE',  ( -1.000000000000000000, -0.000000000000000000, -0.000000000000000000 ) ) ;
#13292 = VERTEX_POINT ( 'NONE', #17436 ) ;
#13293 = ADVANCED_FACE ( 'NONE', ( #40498 ), #10636, .T. ) ;
#13294 = DIRECTION ( 'NONE',  ( -1.000000000000000000, 0.000000000000000000, 0.000000000000000000 ) ) ;
#13295 = ADVANCED_FACE ( 'NONE', ( #16993 ), #24413, .F. ) ;
#13296 = DIRECTION ( 'NONE',  ( 1.000000000000000000, 0.000000000000000000, 0.000000000000000000 ) ) ;
#13297 = EDGE_CURVE ( 'NONE', #21728, #3675, #36604, .T. ) ;
#13298 = ADVANCED_FACE ( 'NONE', ( #350 ), #23968, .F. ) ;
#13299 = VERTEX_POINT ( 'NONE', #10859 ) ;
#13300 = AXIS2_PLACEMENT_3D ( 'NONE', #16541, #33514, #29842 ) ;
#13301 = EDGE_CURVE ( 'NONE', #42436, #37254, #26883, .T. ) ;
#13302 = ORIENTED_EDGE ( 'NONE', *, *, #12158, .T. ) ;
#13303 = FACE_OUTER_BOUND ( 'NONE', #12420, .T. ) ;
#13305 = VERTEX_POINT ( 'NONE', #34614 ) ;
#13304 = VECTOR ( 'NONE', #20448, 1000.000000000000000 ) ;
#13306 = CARTESIAN_POINT ( 'NONE',  ( -3.169834189307653816, 40.00000000000000000, -24.13593742708953727 ) ) ;
#13307 = CARTESIAN_POINT ( 'NONE',  ( 17.99999999999999645, 62.45178862086345362, -93.20969140437443912 ) ) ;
#13308 = VECTOR ( 'NONE', #31323, 1000.000000000000000 ) ;
#13309 = DIRECTION ( 'NONE',  ( -0.000000000000000000, -0.000000000000000000, -1.000000000000000000 ) ) ;
#13310 = AXIS2_PLACEMENT_3D ( 'NONE', #32069, #12021, #29026 ) ;
#13311 = LINE ( 'NONE', #36179, #12896 ) ;
#13312 = AXIS2_PLACEMENT_3D ( 'NONE', #23125, #8927, #36374 ) ;
#13313 = LINE ( 'NONE', #26604, #32473 ) ;
#13314 = ORIENTED_EDGE ( 'NONE', *, *, #31463, .T. ) ;
#13315 = DIRECTION ( 'NONE',  ( -1.000000000000000000, 0.000000000000000000, 0.000000000000000000 ) ) ;
#13316 = ORIENTED_EDGE ( 'NONE', *, *, #38502, .F. ) ;
#13317 = CYLINDRICAL_SURFACE ( 'NONE', #32212, 120.5010000000000190 ) ;
#13318 = CARTESIAN_POINT ( 'NONE',  ( -20.10416666680962550, 31.00000000000000355, -1.308996940106889273 ) ) ;
#13319 = ORIENTED_EDGE ( 'NONE', *, *, #9746, .T. ) ;
#13320 = DIRECTION ( 'NONE',  ( 0.000000000000000000, 0.000000000000000000, 1.000000000000000000 ) ) ;
#13321 = DIRECTION ( 'NONE',  ( -1.000000000000000000, -0.000000000000000000, -0.000000000000000000 ) ) ;
#13322 = APPLICATION_PROTOCOL_DEFINITION ( 'draft international standard', 'automotive_design', 1998, #2979 ) ;
#13323 = CYLINDRICAL_SURFACE ( 'NONE', #10712, 120.5010000000000190 ) ;
#13324 = CARTESIAN_POINT ( 'NONE',  ( -35.70415035507907930, 31.00000000000000355, 46.55071329160319493 ) ) ;
#13325 = ADVANCED_FACE ( 'NONE', ( #41359 ), #11509, .F. ) ;
#13326 = ORIENTED_EDGE ( 'NONE', *, *, #35282, .T. ) ;
#13327 = CARTESIAN_POINT ( 'NONE',  ( 2.319640971205256363, 31.00000000000000355, -34.59922639972668179 ) ) ;
#13328 = CARTESIAN_POINT ( 'NONE',  ( -4.417864660710832503, 40.00000000000000000, 67.60416666563759236 ) ) ;
#13329 = AXIS2_PLACEMENT_3D ( 'NONE', #7758, #18073, #38495 ) ;
#13330 = VECTOR ( 'NONE', #23675, 1000.000000000000000 ) ;
#13331 = VECTOR ( 'NONE', #19326, 1000.000000000000000 ) ;
#13332 = CARTESIAN_POINT ( 'NONE',  ( 17.99999999999999645, 0.000000000000000000, 0.000000000000000000 ) ) ;
#13333 = VECTOR ( 'NONE', #17391, 1000.000000000000000 ) ;
#13334 = EDGE_LOOP ( 'NONE', ( #32222, #12561, #4183, #922 ) ) ;
#13335 = CARTESIAN_POINT ( 'NONE',  ( 9.000000000000001776, -112.8457601792513714, -26.86697618949492039 ) ) ;
#13336 = DIRECTION ( 'NONE',  ( -1.000000000000000000, 0.000000000000000000, -0.000000000000000000 ) ) ;
#13337 = ORIENTED_EDGE ( 'NONE', *, *, #38978, .T. ) ;
#13338 = CARTESIAN_POINT ( 'NONE',  ( -2.781618486875174767, 40.00000000000000000, -42.39583333490362804 ) ) ;
#13339 = CARTESIAN_POINT ( 'NONE',  ( 0.000000000000000000, 0.000000000000000000, 0.000000000000000000 ) ) ;
#13340 = DIRECTION ( 'NONE',  ( 1.000000000000000000, 0.000000000000000000, 0.000000000000000000 ) ) ;
#13341 = CIRCLE ( 'NONE', #19611, 120.5010000000000190 ) ;
#13342 = EDGE_LOOP ( 'NONE', ( #38691, #3456, #9962, #31334 ) ) ;
#13343 = LINE ( 'NONE', #36644, #24539 ) ;
#13344 = DIRECTION ( 'NONE',  ( -1.000000000000000000, -0.000000000000000000, 0.000000000000000000 ) ) ;
#13345 = EDGE_CURVE ( 'NONE', #9453, #40002, #23411, .T. ) ;
#13346 = EDGE_CURVE ( 'NONE', #5841, #9004, #16427, .T. ) ;
#13347 = ORIENTED_EDGE ( 'NONE', *, *, #15250, .T. ) ;
#13348 = CARTESIAN_POINT ( 'NONE',  ( 0.000000000000000000, 19.74581912682842244, 48.10512059033399623 ) ) ;
#13349 = EDGE_LOOP ( 'NONE', ( #31149, #13185, #13687, #38615 ) ) ;
#13350 = ADVANCED_FACE ( 'NONE', ( #15246 ), #5153, .T. ) ;
#13351 = CIRCLE ( 'NONE', #9152, 20.00000000000000711 ) ;
#13352 = ORIENTED_EDGE ( 'NONE', *, *, #7547, .T. ) ;
#13353 = CYLINDRICAL_SURFACE ( 'NONE', #673, 36.00000000000000000 ) ;
#13354 = CARTESIAN_POINT ( 'NONE',  ( 92.49871336439160530, 31.00000000000000000, 31.53380891771210415 ) ) ;
#13355 = ORIENTED_EDGE ( 'NONE', *, *, #20049, .F. ) ;
#13356 = FACE_OUTER_BOUND ( 'NONE', #39749, .T. ) ;
#13357 = DIRECTION ( 'NONE',  ( -1.000000000000000000, -0.000000000000000000, -0.000000000000000000 ) ) ;
#13358 = DIRECTION ( 'NONE',  ( -1.000000000000000000, 0.000000000000000000, 0.000000000000000000 ) ) ;
#13359 = ORIENTED_EDGE ( 'NONE', *, *, #9285, .T. ) ;
#13360 = EDGE_CURVE ( 'NONE', #27819, #35211, #8060, .T. ) ;
#13361 = CARTESIAN_POINT ( 'NONE',  ( 0.000000000000000000, 107.1354928292869744, 44.47455650398100602 ) ) ;
#13362 = CIRCLE ( 'NONE', #4258, 47.49900000000000944 ) ;
#13363 = DIRECTION ( 'NONE',  ( 1.000000000000000000, 0.000000000000000000, 0.000000000000000000 ) ) ;
#13364 = EDGE_CURVE ( 'NONE', #12448, #17417, #12934, .T. ) ;
#13366 = CARTESIAN_POINT ( 'NONE',  ( 0.000000000000000000, 2.007101075699966763, 31.43498920425970411 ) ) ;
#13365 = DIRECTION ( 'NONE',  ( 0.000000000000000000, 0.000000000000000000, 1.000000000000000000 ) ) ;
#13367 = LINE ( 'NONE', #22992, #8910 ) ;
#13368 = ORIENTED_EDGE ( 'NONE', *, *, #31392, .F. ) ;
#13369 = DIRECTION ( 'NONE',  ( 0.000000000000000000, 0.000000000000000000, 1.000000000000000000 ) ) ;
#13370 = CARTESIAN_POINT ( 'NONE',  ( -2.127120017302697619, 31.00000000000000355, -32.39583333539214038 ) ) ;
#13371 = AXIS2_PLACEMENT_3D ( 'NONE', #40738, #14385, #27696 ) ;
#13372 = VERTEX_POINT ( 'NONE', #41804 ) ;
#13373 = DIRECTION ( 'NONE',  ( 1.000000000000000000, 0.000000000000000000, 0.000000000000000000 ) ) ;
#13374 = CARTESIAN_POINT ( 'NONE',  ( 17.99999999999999645, -118.8387007424472159, 19.94628303336445185 ) ) ;
#13375 = ORIENTED_EDGE ( 'NONE', *, *, #25989, .F. ) ;
#13376 = CARTESIAN_POINT ( 'NONE',  ( 0.000000000000000000, 27.24480646643629811, -15.80846360676556372 ) ) ;
#13377 = ADVANCED_FACE ( 'NONE', ( #32001 ), #18519, .T. ) ;
#13378 = CARTESIAN_POINT ( 'NONE',  ( 33.03432996520027132, 40.00000000000000000, -28.98482729919588863 ) ) ;
#13379 = CARTESIAN_POINT ( 'NONE',  ( -28.59133019391067165, 40.00000000000000000, -32.71076623427350683 ) ) ;
#13380 = VERTEX_POINT ( 'NONE', #17871 ) ;
#13381 = ORIENTED_EDGE ( 'NONE', *, *, #7547, .F. ) ;
#13382 = PRESENTATION_STYLE_ASSIGNMENT (( #6579 ) ) ;
#13383 = CARTESIAN_POINT ( 'NONE',  ( -3.239593890920906993, -13.56862304811759223, -1.199999999999999956 ) ) ;
#13384 = DIRECTION ( 'NONE',  ( -3.996523416598930318E-16, 2.658563593772947863E-15, 1.000000000000000000 ) ) ;
#13385 = DIRECTION ( 'NONE',  ( -1.000000000000000000, 0.000000000000000000, -0.000000000000000000 ) ) ;
#13386 = ORIENTED_EDGE ( 'NONE', *, *, #32240, .F. ) ;
#13387 = DIRECTION ( 'NONE',  ( 1.000000000000000000, -1.373900992973642263E-15, -3.736327486719295592E-16 ) ) ;
#13388 = ORIENTED_EDGE ( 'NONE', *, *, #20546, .F. ) ;
#13389 = DIRECTION ( 'NONE',  ( 1.000000000000000000, 0.000000000000000000, 0.000000000000000000 ) ) ;
#13390 = DIRECTION ( 'NONE',  ( -1.000000000000000000, 0.000000000000000000, 0.000000000000000000 ) ) ;
#13391 = CIRCLE ( 'NONE', #21083, 31.49900000000000233 ) ;
#13392 = ORIENTED_EDGE ( 'NONE', *, *, #20621, .F. ) ;
#13393 = DIRECTION ( 'NONE',  ( 0.000000000000000000, 0.5264321628773569461, -0.8502171357296133269 ) ) ;
#13394 = VECTOR ( 'NONE', #3025, 1000.000000000000000 ) ;
#13395 = EDGE_CURVE ( 'NONE', #10692, #1826, #28540, .T. ) ;
#13396 = DIRECTION ( 'NONE',  ( -1.058513553088275437E-16, -1.000000000000000000, 8.813324511995299047E-17 ) ) ;
#13397 = ORIENTED_EDGE ( 'NONE', *, *, #38291, .F. ) ;
#13398 = DIRECTION ( 'NONE',  ( -1.000000000000000000, 0.000000000000000000, 0.000000000000000000 ) ) ;
#13399 = VERTEX_POINT ( 'NONE', #21588 ) ;
#13400 = CYLINDRICAL_SURFACE ( 'NONE', #22575, 59.00000000000000000 ) ;
#13401 = EDGE_LOOP ( 'NONE', ( #22537, #15078, #31499, #18823 ) ) ;
#13403 = ORIENTED_EDGE ( 'NONE', *, *, #42519, .F. ) ;
#13402 = DIRECTION ( 'NONE',  ( 0.000000000000000000, -0.1253332335643113360, 0.9921147013144769877 ) ) ;
#13404 = CARTESIAN_POINT ( 'NONE',  ( -26.77709713317330653, 31.00000000000000355, 54.08981485145582013 ) ) ;
#13405 = VERTEX_POINT ( 'NONE', #34834 ) ;
#13406 = FACE_OUTER_BOUND ( 'NONE', #22238, .T. ) ;
#13407 = EDGE_CURVE ( 'NONE', #8083, #39631, #31145, .T. ) ;
#13408 = ORIENTED_EDGE ( 'NONE', *, *, #130, .F. ) ;
#13409 = ADVANCED_FACE ( 'NONE', ( #1235 ), #4947, .F. ) ;
#13410 = DIRECTION ( 'NONE',  ( -1.000000000000000000, 0.000000000000000000, -0.000000000000000000 ) ) ;
#13411 = PRODUCT_DEFINITION_SHAPE ( 'NONE', 'NONE',  #23650 ) ;
#13412 = VERTEX_POINT ( 'NONE', #18096 ) ;
#13413 = CARTESIAN_POINT ( 'NONE',  ( 52.26791824981292933, 40.00000000000000000, -67.94187691988643962 ) ) ;
#13414 = EDGE_CURVE ( 'NONE', #4007, #36553, #11292, .T. ) ;
#13416 = DIRECTION ( 'NONE',  ( -1.000000000000000000, -0.000000000000000000, -0.000000000000000000 ) ) ;
#13415 = DIRECTION ( 'NONE',  ( 0.000000000000000000, 0.000000000000000000, -1.000000000000000000 ) ) ;
#13417 = CARTESIAN_POINT ( 'NONE',  ( -101.6738636939643357, 31.00000000000000000, -5.192942712545359107 ) ) ;
#13418 = ORIENTED_EDGE ( 'NONE', *, *, #7629, .F. ) ;
#13419 = DIRECTION ( 'NONE',  ( 0.000000000000000000, 0.1837495178165637066, 0.9829730996839030066 ) ) ;
#13420 = ORIENTED_EDGE ( 'NONE', *, *, #41790, .T. ) ;
#13421 =( NAMED_UNIT ( * ) SI_UNIT ( $, .STERADIAN. ) SOLID_ANGLE_UNIT ( ) );
#13422 = VECTOR ( 'NONE', #23354, 1000.000000000000000 ) ;
#13423 = DIRECTION ( 'NONE',  ( -1.000000000000000000, 0.000000000000000000, -0.000000000000000000 ) ) ;
#13424 = AXIS2_PLACEMENT_3D ( 'NONE', #3513, #36910, #30170 ) ;
#13425 = CARTESIAN_POINT ( 'NONE',  ( 71.66629920589342362, 31.00000000000000000, 24.32769631419027689 ) ) ;
#13427 = DIRECTION ( 'NONE',  ( -1.000000000000000000, -0.000000000000000000, -0.000000000000000000 ) ) ;
#13426 = CYLINDRICAL_SURFACE ( 'NONE', #39942, 51.99999999999999289 ) ;
#13428 = VERTEX_POINT ( 'NONE', #31358 ) ;
#13429 = AXIS2_PLACEMENT_3D ( 'NONE', #27287, #40557, #36869 ) ;
#13430 = EDGE_CURVE ( 'NONE', #41700, #20548, #34528, .T. ) ;
#13431 = DIRECTION ( 'NONE',  ( 0.000000000000000000, -0.2486898871648415554, -0.9685831611286345177 ) ) ;
#13432 = EDGE_CURVE ( 'NONE', #36472, #4217, #21349, .T. ) ;
#13433 = AXIS2_PLACEMENT_3D ( 'NONE', #15322, #38188, #28612 ) ;
#13434 = ORIENTED_EDGE ( 'NONE', *, *, #33016, .T. ) ;
#13435 = DIRECTION ( 'NONE',  ( 1.000000000000000000, 0.000000000000000000, 0.000000000000000000 ) ) ;
#13436 = EDGE_CURVE ( 'NONE', #31605, #4616, #7497, .T. ) ;
#13437 = CARTESIAN_POINT ( 'NONE',  ( 18.00000000000000355, 0.000000000000000000, 0.000000000000000000 ) ) ;
#13438 =( NAMED_UNIT ( * ) PLANE_ANGLE_UNIT ( ) SI_UNIT ( $, .RADIAN. ) );
#13439 = CARTESIAN_POINT ( 'NONE',  ( 17.99999999999999645, -114.6488492393081913, 37.09625815499973100 ) ) ;
#13440 = ORIENTED_EDGE ( 'NONE', *, *, #42069, .F. ) ;
#13441 = DIRECTION ( 'NONE',  ( 0.000000000000000000, -0.9980267284282723361, 0.06279051952930261860 ) ) ;
#13442 = VERTEX_POINT ( 'NONE', #31066 ) ;
#13443 = CYLINDRICAL_SURFACE ( 'NONE', #31876, 59.00000000000000000 ) ;
#13444 = MANIFOLD_SOLID_BREP ( 'RollersSimplified', #23347 ) ;
#13445 = DIRECTION ( 'NONE',  ( -1.000000000000000000, -0.000000000000000000, 0.000000000000000000 ) ) ;
#13446 = DIRECTION ( 'NONE',  ( 0.000000000000000000, 0.000000000000000000, 1.000000000000000000 ) ) ;
#13447 = ORIENTED_EDGE ( 'NONE', *, *, #24054, .T. ) ;
#13448 = ORIENTED_EDGE ( 'NONE', *, *, #16296, .F. ) ;
#13449 = CARTESIAN_POINT ( 'NONE',  ( 17.99999999999999645, 0.000000000000000000, 0.000000000000000000 ) ) ;
#13450 = EDGE_CURVE ( 'NONE', #5730, #16033, #372, .T. ) ;
#13451 = DIRECTION ( 'NONE',  ( -1.000000000000000000, 0.000000000000000000, 0.000000000000000000 ) ) ;
#13452 = CIRCLE ( 'NONE', #29454, 116.0000000000000000 ) ;
#13453 = DIRECTION ( 'NONE',  ( 0.000000000000000000, -0.7164567402983067490, -0.6976315211349933820 ) ) ;
#13455 = ORIENTED_EDGE ( 'NONE', *, *, #9886, .T. ) ;
#13454 = CARTESIAN_POINT ( 'NONE',  ( 17.99999999999999645, 25.46650492921896713, 19.29328419707794495 ) ) ;
#13456 = CARTESIAN_POINT ( 'NONE',  ( 28.62564328229763788, 31.00000000000000355, -21.88780996306212501 ) ) ;
#13457 = CARTESIAN_POINT ( 'NONE',  ( 42.80287614962723808, -35.35525454449572180, 69.29271901957299917 ) ) ;
#13458 = AXIS2_PLACEMENT_3D ( 'NONE', #10433, #30724, #40511 ) ;
#13459 = EDGE_CURVE ( 'NONE', #4224, #39574, #8744, .T. ) ;
#13461 = ORIENTED_EDGE ( 'NONE', *, *, #6908, .T. ) ;
#13460 = CARTESIAN_POINT ( 'NONE',  ( 0.000000000000000000, 0.000000000000000000, 0.000000000000000000 ) ) ;
#13462 = UNCERTAINTY_MEASURE_WITH_UNIT (LENGTH_MEASURE( 1.000000000000000082E-05 ), #13282, 'distance_accuracy_value', 'NONE');
#13463 = ORIENTED_EDGE ( 'NONE', *, *, #12200, .F. ) ;
#13464 = LINE ( 'NONE', #21498, #15008 ) ;
#13465 = DIRECTION ( 'NONE',  ( -1.000000000000000000, -0.000000000000000000, -0.000000000000000000 ) ) ;
#13467 = CARTESIAN_POINT ( 'NONE',  ( -46.12092335263332643, 40.00000000000000000, 22.64177125690310177 ) ) ;
#13466 = AXIS2_PLACEMENT_3D ( 'NONE', #26824, #6741, #3450 ) ;
#13468 = CARTESIAN_POINT ( 'NONE',  ( 0.000000000000000000, 67.32409792376505209, 89.75376489259387824 ) ) ;
#13469 = DIRECTION ( 'NONE',  ( -1.000000000000000000, -0.000000000000000000, 0.000000000000000000 ) ) ;
#13470 = LINE ( 'NONE', #42884, #25569 ) ;
#13471 = VERTEX_POINT ( 'NONE', #34323 ) ;
#13472 = DIRECTION ( 'NONE',  ( -1.000000000000000000, 0.000000000000000000, -0.000000000000000000 ) ) ;
#13473 = ORIENTED_EDGE ( 'NONE', *, *, #17637, .F. ) ;
#13474 = DIRECTION ( 'NONE',  ( 0.000000000000000000, 0.000000000000000000, 1.000000000000000000 ) ) ;
#13475 = DIRECTION ( 'NONE',  ( -1.000000000000000000, 0.000000000000000000, 0.000000000000000000 ) ) ;
#13476 = CARTESIAN_POINT ( 'NONE',  ( 44.89583333484414140, 31.00000000000000355, -2.945243104263157274 ) ) ;
#13477 = CARTESIAN_POINT ( 'NONE',  ( 9.000000000000001776, -49.65209126885752511, -15.44894276735603889 ) ) ;
#13478 = ORIENTED_EDGE ( 'NONE', *, *, #23591, .F. ) ;
#13479 = DIRECTION ( 'NONE',  ( -1.000000000000000000, -0.000000000000000000, -0.000000000000000000 ) ) ;
#13480 = ORIENTED_EDGE ( 'NONE', *, *, #27106, .T. ) ;
#13481 = AXIS2_PLACEMENT_3D ( 'NONE', #31340, #21568, #1422 ) ;
#13482 = CARTESIAN_POINT ( 'NONE',  ( -19.47536345555549886, 40.00000000000000000, -6.605835105517199324 ) ) ;
#13483 = ADVANCED_FACE ( 'NONE', ( #20861 ), #40213, .T. ) ;
#13484 = VERTEX_POINT ( 'NONE', #37805 ) ;
#13485 = EDGE_CURVE ( 'NONE', #21478, #27228, #17160, .T. ) ;
#13486 = CARTESIAN_POINT ( 'NONE',  ( 18.00000000000000355, -9.744342220503087404, -46.48873837489808380 ) ) ;
#13487 = CARTESIAN_POINT ( 'NONE',  ( 50.06853320191206791, 31.00000000000000000, -56.91684085115753078 ) ) ;
#13488 = CARTESIAN_POINT ( 'NONE',  ( -60.98551593176824070, 40.00000000000000711, 53.34359504439791522 ) ) ;
#13489 = DIRECTION ( 'NONE',  ( -1.000000000000000000, -0.000000000000000000, -0.000000000000000000 ) ) ;
#13490 = PRESENTATION_LAYER_ASSIGNMENT (  '', '', ( #10670 ) ) ;
#13491 = EDGE_LOOP ( 'NONE', ( #10134, #7032, #35893, #41611 ) ) ;
#13492 = ORIENTED_EDGE ( 'NONE', *, *, #14242, .F. ) ;
#13493 = CARTESIAN_POINT ( 'NONE',  ( 0.000000000000000000, 0.000000000000000000, 0.000000000000000000 ) ) ;
#13494 = DIRECTION ( 'NONE',  ( 1.000000000000000000, 0.000000000000000000, 0.000000000000000000 ) ) ;
#13495 = CYLINDRICAL_SURFACE ( 'NONE', #3136, 51.99999999999999289 ) ;
#13497 = ORIENTED_EDGE ( 'NONE', *, *, #39998, .T. ) ;
#13496 = CARTESIAN_POINT ( 'NONE',  ( 0.000000000000000000, 112.5220807139884016, 28.19186676675879255 ) ) ;
#13498 = DIRECTION ( 'NONE',  ( 1.000000000000000000, 0.000000000000000000, 0.000000000000000000 ) ) ;
#13499 = VERTEX_POINT ( 'NONE', #30644 ) ;
#13500 = FACE_OUTER_BOUND ( 'NONE', #29526, .T. ) ;
#13501 = ADVANCED_FACE ( 'NONE', ( #4418 ), #4208, .T. ) ;
#13502 = CARTESIAN_POINT ( 'NONE',  ( 74.49266661913014786, 39.99999999999999289, 43.00976416799198176 ) ) ;
#13503 = DIRECTION ( 'NONE',  ( -1.000000000000000000, -0.000000000000000000, 0.000000000000000000 ) ) ;
#13504 = ORIENTED_EDGE ( 'NONE', *, *, #17362, .T. ) ;
#13505 = CARTESIAN_POINT ( 'NONE',  ( 17.99999999999999645, -73.78980555658671392, 95.26571049921967926 ) ) ;
#13506 = AXIS2_PLACEMENT_3D ( 'NONE', #42369, #12089, #38667 ) ;
#13507 = DIRECTION ( 'NONE',  ( 0.000000000000000000, 6.115635305138573842E-15, -1.000000000000000000 ) ) ;
#13508 = CIRCLE ( 'NONE', #20529, 116.0000000000000000 ) ;
#13509 = SHAPE_REPRESENTATION ( 'spur gear_iso_ISO - Spur gear 2M 50T 20PA 18FW ---S50B22H150L15.0N', ( #13552 ), #23928 ) ;
#13510 = VERTEX_POINT ( 'NONE', #36946 ) ;
#13511 = ADVANCED_FACE ( 'NONE', ( #21286 ), #17790, .T. ) ;
#13512 = AXIS2_PLACEMENT_3D ( 'NONE', #34498, #28425, #37985 ) ;
#13513 = ORIENTED_EDGE ( 'NONE', *, *, #4926, .F. ) ;
#13514 = CARTESIAN_POINT ( 'NONE',  ( 0.000000000000000000, 1.178949249685212974, -2.042000000000001148 ) ) ;
#13515 = ORIENTED_EDGE ( 'NONE', *, *, #16879, .T. ) ;
#13516 = CARTESIAN_POINT ( 'NONE',  ( -19.81637295874436333, 40.00000000000000000, -11.44243563873878777 ) ) ;
#13517 = CARTESIAN_POINT ( 'NONE',  ( 18.00000000000000355, 0.000000000000000000, 0.000000000000000000 ) ) ;
#13518 = DIRECTION ( 'NONE',  ( -1.000000000000000000, -0.000000000000000000, -0.000000000000000000 ) ) ;
#13519 = EDGE_CURVE ( 'NONE', #10297, #40092, #37159, .T. ) ;
#13520 = DIRECTION ( 'NONE',  ( 0.000000000000000000, 0.6783118362696123338, 0.7347741508630707408 ) ) ;
#13521 = DIRECTION ( 'NONE',  ( 0.000000000000000000, -0.8477344278896649099, -0.5304209081197521769 ) ) ;
#13522 = ORIENTED_EDGE ( 'NONE', *, *, #3431, .F. ) ;
#13523 = CARTESIAN_POINT ( 'NONE',  ( 17.99999999999999645, 29.02167576844250618, -108.3790330702166926 ) ) ;
#13524 = ORIENTED_EDGE ( 'NONE', *, *, #19420, .T. ) ;
#13525 = AXIS2_PLACEMENT_3D ( 'NONE', #38935, #5137, #18930 ) ;
#13526 = DIRECTION ( 'NONE',  ( -1.000000000000000000, 0.000000000000000000, 0.000000000000000000 ) ) ;
#13527 = LINE ( 'NONE', #27053, #19992 ) ;
#13528 = EDGE_CURVE ( 'NONE', #18562, #4807, #14277, .T. ) ;
#13529 = ORIENTED_EDGE ( 'NONE', *, *, #42224, .T. ) ;
#13530 = FACE_OUTER_BOUND ( 'NONE', #34312, .T. ) ;
#13531 = CARTESIAN_POINT ( 'NONE',  ( 0.000000000000000000, 0.000000000000000000, 0.000000000000000000 ) ) ;
#13532 = CIRCLE ( 'NONE', #19126, 116.0000000000000000 ) ;
#13533 = CARTESIAN_POINT ( 'NONE',  ( 18.00000000000000355, 0.000000000000000000, 0.000000000000000000 ) ) ;
#13534 = CARTESIAN_POINT ( 'NONE',  ( 43.85342918759069164, 31.00000000000000355, 49.98553323097543455 ) ) ;
#13535 = EDGE_CURVE ( 'NONE', #30056, #6492, #39368, .T. ) ;
#13536 = EDGE_CURVE ( 'NONE', #42855, #22705, #7333, .T. ) ;
#13537 = VERTEX_POINT ( 'NONE', #40631 ) ;
#13538 = CARTESIAN_POINT ( 'NONE',  ( 25.29542371717656835, 31.00000000000000355, 28.93716311998947788 ) ) ;
#13539 = EDGE_CURVE ( 'NONE', #39306, #34314, #19932, .T. ) ;
#13540 = ADVANCED_FACE ( 'NONE', ( #34973 ), #15575, .F. ) ;
#13541 = CARTESIAN_POINT ( 'NONE',  ( 46.64447153568531945, 40.00000000000000000, 60.78881617101084345 ) ) ;
#13542 = VECTOR ( 'NONE', #31618, 1000.000000000000000 ) ;
#13543 = DIRECTION ( 'NONE',  ( 0.000000000000000000, 0.000000000000000000, 1.000000000000000000 ) ) ;
#13544 = DIRECTION ( 'NONE',  ( -1.000000000000000000, 0.000000000000000000, -0.000000000000000000 ) ) ;
#13545 = ORIENTED_EDGE ( 'NONE', *, *, #10059, .T. ) ;
#13546 = CARTESIAN_POINT ( 'NONE',  ( 0.000000000000000000, 0.000000000000000000, 0.000000000000000000 ) ) ;
#13547 = DIRECTION ( 'NONE',  ( -1.000000000000000000, -0.000000000000000000, -0.000000000000000000 ) ) ;
#13548 = AXIS2_PLACEMENT_3D ( 'NONE', #41680, #35348, #11600 ) ;
#13549 = ORIENTED_EDGE ( 'NONE', *, *, #24497, .T. ) ;
#13550 = CARTESIAN_POINT ( 'NONE',  ( 26.72236725836960147, 40.00000000000000000, -46.28813965123160301 ) ) ;
#13551 = DIRECTION ( 'NONE',  ( 0.000000000000000000, 0.9510565162951544194, -0.3090169943749447312 ) ) ;
#13552 = AXIS2_PLACEMENT_3D ( 'NONE', #3852, #14597, #10213 ) ;
#13553 = DIRECTION ( 'NONE',  ( -1.000000000000000000, -0.000000000000000000, -0.000000000000000000 ) ) ;
#13554 = ORIENTED_EDGE ( 'NONE', *, *, #18087, .T. ) ;
#13555 = CYLINDRICAL_SURFACE ( 'NONE', #25946, 120.5010000000000190 ) ;
#13556 = DIRECTION ( 'NONE',  ( -1.000000000000000000, -0.000000000000000000, 0.000000000000000000 ) ) ;
#13557 = ORIENTED_EDGE ( 'NONE', *, *, #5551, .T. ) ;
#13558 = DIRECTION ( 'NONE',  ( -1.000000000000000000, -0.000000000000000000, 0.000000000000000000 ) ) ;
#13559 = ORIENTED_EDGE ( 'NONE', *, *, #39941, .F. ) ;
#13560 = CIRCLE ( 'NONE', #27474, 13.59999999999999964 ) ;
#13561 = AXIS2_PLACEMENT_3D ( 'NONE', #38181, #25558, #38388 ) ;
#13562 = EDGE_CURVE ( 'NONE', #11213, #3516, #31776, .T. ) ;
#13563 = VERTEX_POINT ( 'NONE', #11434 ) ;
#13564 = VECTOR ( 'NONE', #35466, 1000.000000000000000 ) ;
#13565 = PLANE ( 'NONE',  #29964 ) ;
#13566 = CARTESIAN_POINT ( 'NONE',  ( 73.86091552538547944, 31.00000000000000000, 64.94433634442138725 ) ) ;
#13567 = ORIENTED_EDGE ( 'NONE', *, *, #29074, .T. ) ;
#13568 = FACE_OUTER_BOUND ( 'NONE', #5859, .T. ) ;
#13569 = ADVANCED_FACE ( 'NONE', ( #5305 ), #8358, .F. ) ;
#13570 = VECTOR ( 'NONE', #8470, 1000.000000000000000 ) ;
#13571 = FACE_OUTER_BOUND ( 'NONE', #14724, .T. ) ;
#13572 = DIRECTION ( 'NONE',  ( 0.000000000000000000, 0.000000000000000000, 1.000000000000000000 ) ) ;
#13573 = ORIENTED_EDGE ( 'NONE', *, *, #30632, .F. ) ;
#13574 = DIRECTION ( 'NONE',  ( -1.000000000000000000, -0.000000000000000000, -0.000000000000000000 ) ) ;
#13575 = CIRCLE ( 'NONE', #37274, 20.00000000000000000 ) ;
#13576 = CARTESIAN_POINT ( 'NONE',  ( -91.96080130434580724, -40.05525454449572464, 14.45886780445738218 ) ) ;
#13578 = LINE ( 'NONE', #36890, #33783 ) ;
#13577 = DIRECTION ( 'NONE',  ( -1.000000000000000000, -0.000000000000000000, -0.000000000000000000 ) ) ;
#13579 = DIRECTION ( 'NONE',  ( -1.000000000000000000, 0.000000000000000000, 0.000000000000000000 ) ) ;
#13580 = EDGE_CURVE ( 'NONE', #27343, #19555, #23985, .T. ) ;
#13581 = ORIENTED_EDGE ( 'NONE', *, *, #21276, .T. ) ;
#13583 = AXIS2_PLACEMENT_3D ( 'NONE', #25001, #31291, #35180 ) ;
#13582 = FILL_AREA_STYLE ('',( #32760 ) ) ;
#13584 = CARTESIAN_POINT ( 'NONE',  ( -5.542584477697039880, 31.00000000000000355, -42.01772079774592328 ) ) ;
#13585 = ORIENTED_EDGE ( 'NONE', *, *, #26227, .T. ) ;
#13586 = FACE_OUTER_BOUND ( 'NONE', #37729, .T. ) ;
#13587 = LINE ( 'NONE', #36674, #8437 ) ;
#13588 = ORIENTED_EDGE ( 'NONE', *, *, #19959, .F. ) ;
#13589 = MANIFOLD_SOLID_BREP ( 'Boss-Extrude1', #35804 ) ;
#13590 = EDGE_CURVE ( 'NONE', #38310, #25529, #21389, .T. ) ;
#13591 = EDGE_CURVE ( 'NONE', #32317, #23529, #39400, .T. ) ;
#13592 = CARTESIAN_POINT ( 'NONE',  ( 38.32544124395173668, 40.00000000000000000, -22.13982348525413002 ) ) ;
#13593 = AXIS2_PLACEMENT_3D ( 'NONE', #27455, #31164, #1254 ) ;
#13594 = CARTESIAN_POINT ( 'NONE',  ( 46.49836147156941735, 40.00000000000000000, -6.043767708841586206 ) ) ;
#13595 = ADVANCED_FACE ( 'NONE', ( #15370 ), #34765, .F. ) ;
#13596 = AXIS2_PLACEMENT_3D ( 'NONE', #1171, #27829, #14736 ) ;
#13597 = ORIENTED_EDGE ( 'NONE', *, *, #35083, .T. ) ;
#13598 = DIRECTION ( 'NONE',  ( 1.000000000000000000, 0.000000000000000000, 0.000000000000000000 ) ) ;
#13599 = FACE_OUTER_BOUND ( 'NONE', #28797, .T. ) ;
#13600 = PRESENTATION_LAYER_ASSIGNMENT (  '', '', ( #33788 ) ) ;
#13601 = DIRECTION ( 'NONE',  ( 0.000000000000000000, 0.000000000000000000, 1.000000000000000000 ) ) ;
#13602 = AXIS2_PLACEMENT_3D ( 'NONE', #14748, #28052, #41310 ) ;
#13603 = ORIENTED_EDGE ( 'NONE', *, *, #26144, .F. ) ;
#13604 = CARTESIAN_POINT ( 'NONE',  ( 10.28773449565296083, 40.00000000000000000, -20.88174966193524895 ) ) ;
#13605 = ORIENTED_EDGE ( 'NONE', *, *, #11338, .F. ) ;
#13606 = CARTESIAN_POINT ( 'NONE',  ( 147.8499999999987153, 1.396194884625391392E-12, 6.999999999999958256 ) ) ;
#13607 = CARTESIAN_POINT ( 'NONE',  ( -10.00000000000000000, 0.000000000000000000, 0.000000000000000000 ) ) ;
#13608 = ADVANCED_FACE ( 'NONE', ( #31708 ), #28667, .T. ) ;
#13609 = EDGE_LOOP ( 'NONE', ( #25249, #35742, #35688, #41259 ) ) ;
#13610 = DIRECTION ( 'NONE',  ( 1.000000000000000000, 0.000000000000000000, 0.000000000000000000 ) ) ;
#13611 = DIRECTION ( 'NONE',  ( 0.000000000000000000, -1.224646799147364054E-16, 1.000000000000000000 ) ) ;
#13612 = ORIENTED_EDGE ( 'NONE', *, *, #40914, .F. ) ;
#13613 = FACE_OUTER_BOUND ( 'NONE', #11724, .T. ) ;
#13614 = EDGE_LOOP ( 'NONE', ( #8981, #32037, #17705, #19043 ) ) ;
#13615 = DIRECTION ( 'NONE',  ( 0.000000000000000000, 0.000000000000000000, 1.000000000000000000 ) ) ;
#13616 = AXIS2_PLACEMENT_3D ( 'NONE', #18674, #15373, #11437 ) ;
#13617 = ORIENTED_EDGE ( 'NONE', *, *, #6080, .T. ) ;
#13619 = EDGE_LOOP ( 'NONE', ( #2048, #21039, #30786, #7632 ) ) ;
#13618 = CARTESIAN_POINT ( 'NONE',  ( 0.000000000000000000, -34.03109950475806045, 115.5957406979048727 ) ) ;
#13620 = CARTESIAN_POINT ( 'NONE',  ( 8.570044366903687205, 31.00000000000000355, -64.27561742005508449 ) ) ;
#13621 = EDGE_LOOP ( 'NONE', ( #29673, #21273 ) ) ;
#13622 = CARTESIAN_POINT ( 'NONE',  ( -100.0589655806010967, 31.00000000000001421, 21.59728106529621172 ) ) ;
#13623 = VECTOR ( 'NONE', #15331, 1000.000000000000000 ) ;
#13624 = ADVANCED_FACE ( 'NONE', ( #1586 ), #21721, .F. ) ;
#13625 = AXIS2_PLACEMENT_3D ( 'NONE', #10386, #23724, #4858 ) ;
#13626 = ORIENTED_EDGE ( 'NONE', *, *, #5351, .T. ) ;
#13627 = CARTESIAN_POINT ( 'NONE',  ( 18.00000000000000355, 20.99948489194423118, 42.60488980472788967 ) ) ;
#13628 = ORIENTED_EDGE ( 'NONE', *, *, #23425, .T. ) ;
#13629 = CARTESIAN_POINT ( 'NONE',  ( -50.81742119984753714, 40.00000000000000000, -66.42451308377114572 ) ) ;
#13631 = CARTESIAN_POINT ( 'NONE',  ( 6.004904395537136175, 0.000000000000000000, 0.000000000000000000 ) ) ;
#13630 = CARTESIAN_POINT ( 'NONE',  ( 0.000000000000000000, 31.48608500567870294, -0.9019157472705674472 ) ) ;
#13632 = AXIS2_PLACEMENT_3D ( 'NONE', #5780, #20636, #33907 ) ;
#13633 = DIRECTION ( 'NONE',  ( 0.000000000000000000, 0.000000000000000000, 1.000000000000000000 ) ) ;
#13634 = VERTEX_POINT ( 'NONE', #41510 ) ;
#13635 = FACE_OUTER_BOUND ( 'NONE', #1180, .T. ) ;
#13636 = ORIENTED_EDGE ( 'NONE', *, *, #25433, .F. ) ;
#13637 = CIRCLE ( 'NONE', #40780, 58.99999999999999289 ) ;
#13638 = DIRECTION ( 'NONE',  ( 0.000000000000000000, -0.9574220383620080099, 0.2886919473396124536 ) ) ;
#13639 = ORIENTED_EDGE ( 'NONE', *, *, #12258, .F. ) ;
#13640 = DIRECTION ( 'NONE',  ( -1.000000000000000000, -0.000000000000000000, 0.000000000000000000 ) ) ;
#13641 = EDGE_CURVE ( 'NONE', #33690, #37185, #23444, .T. ) ;
#13642 = CARTESIAN_POINT ( 'NONE',  ( -40.67465422008825726, 31.00000000000000355, -82.48404079236435393 ) ) ;
#13643 = CARTESIAN_POINT ( 'NONE',  ( 1.274258131564866448, 3.883108878240963513, -3.220599429844046568 ) ) ;
#13644 = ORIENTED_EDGE ( 'NONE', *, *, #14381, .T. ) ;
#13645 = EDGE_CURVE ( 'NONE', #14175, #20513, #16462, .T. ) ;
#13646 = DIRECTION ( 'NONE',  ( -1.000000000000000000, -0.000000000000000000, -0.000000000000000000 ) ) ;
#13647 = ORIENTED_EDGE ( 'NONE', *, *, #29903, .T. ) ;
#13648 = CARTESIAN_POINT ( 'NONE',  ( 0.000000000000000000, -14.84191762912296930, -27.78316904333141224 ) ) ;
#13650 = CARTESIAN_POINT ( 'NONE',  ( 0.000000000000000000, 44.47301969247467923, -16.68249143361863318 ) ) ;
#13649 = AXIS2_PLACEMENT_3D ( 'NONE', #5565, #28922, #28071 ) ;
#13651 = FACE_OUTER_BOUND ( 'NONE', #29287, .T. ) ;
#13652 = CIRCLE ( 'NONE', #29655, 52.00000000000000000 ) ;
#13653 = EDGE_CURVE ( 'NONE', #7056, #38476, #17194, .T. ) ;
#13654 = CIRCLE ( 'NONE', #40074, 59.00000000000000000 ) ;
#13655 = ORIENTED_EDGE ( 'NONE', *, *, #11974, .T. ) ;
#13656 = DIRECTION ( 'NONE',  ( -1.000000000000000000, 0.000000000000000000, 0.000000000000000000 ) ) ;
#13657 = ORIENTED_EDGE ( 'NONE', *, *, #15199, .F. ) ;
#13658 = FACE_OUTER_BOUND ( 'NONE', #27503, .T. ) ;
#13659 = CIRCLE ( 'NONE', #12288, 116.0000000000000000 ) ;
#13660 = DIRECTION ( 'NONE',  ( 0.000000000000000000, 0.000000000000000000, -1.000000000000000000 ) ) ;
#13661 = CIRCLE ( 'NONE', #42281, 52.00000000000000000 ) ;
#13662 = ADVANCED_FACE ( 'NONE', ( #10358 ), #11024, .F. ) ;
#13663 = CARTESIAN_POINT ( 'NONE',  ( 0.000000000000000000, 0.000000000000000000, 0.000000000000000000 ) ) ;
#13664 = ORIENTED_EDGE ( 'NONE', *, *, #15710, .F. ) ;
#13665 = VERTEX_POINT ( 'NONE', #26947 ) ;
#13666 = DIRECTION ( 'NONE',  ( -1.000000000000000000, 1.373900992973641671E-15, 4.270088556250623393E-16 ) ) ;
#13667 = CARTESIAN_POINT ( 'NONE',  ( 2.164352920501968783E-14, -1.058809993658035131E-13, -39.99999999999997868 ) ) ;
#13668 = CARTESIAN_POINT ( 'NONE',  ( 8.999999999999998224, -104.0201923570379137, 51.34003878071028026 ) ) ;
#13670 = ORIENTED_EDGE ( 'NONE', *, *, #4134, .T. ) ;
#13669 = CARTESIAN_POINT ( 'NONE',  ( 17.99999999999999645, 21.56073507908645936, 23.57770962728572428 ) ) ;
#13671 = CARTESIAN_POINT ( 'NONE',  ( -9.709369018688816411, 31.00000000000000355, 28.47525938324675820 ) ) ;
#13672 = DIRECTION ( 'NONE',  ( 0.000000000000000000, 0.9618256431728199329, -0.2736629900720800590 ) ) ;
#13674 = ORIENTED_EDGE ( 'NONE', *, *, #3879, .F. ) ;
#13673 = FACE_OUTER_BOUND ( 'NONE', #9031, .T. ) ;
#13675 = EDGE_LOOP ( 'NONE', ( #29104, #14821, #36892, #1262 ) ) ;
#13676 = DIRECTION ( 'NONE',  ( -1.000000000000000000, 0.000000000000000000, 0.000000000000000000 ) ) ;
#13677 = EDGE_CURVE ( 'NONE', #23373, #37256, #22764, .T. ) ;
#13678 = CARTESIAN_POINT ( 'NONE',  ( 18.00000000000000355, 46.87740477351718482, -3.172455868805370560 ) ) ;
#13679 = CARTESIAN_POINT ( 'NONE',  ( 17.81483206086863191, 40.00000000000000000, -52.17936214187551514 ) ) ;
#13680 = CARTESIAN_POINT ( 'NONE',  ( 8.999999999999998224, 59.47573314508733944, 99.59235496188628645 ) ) ;
#13681 = VECTOR ( 'NONE', #19490, 1000.000000000000000 ) ;
#13682 = CYLINDRICAL_SURFACE ( 'NONE', #39356, 47.49900000000000233 ) ;
#13684 = ORIENTED_EDGE ( 'NONE', *, *, #32982, .F. ) ;
#13683 = AXIS2_PLACEMENT_3D ( 'NONE', #30531, #41168, #11318 ) ;
#13685 = DIRECTION ( 'NONE',  ( 0.000000000000000000, 0.000000000000000000, 1.000000000000000000 ) ) ;
#13686 = CIRCLE ( 'NONE', #33838, 58.99999999999999289 ) ;
#13687 = ORIENTED_EDGE ( 'NONE', *, *, #6217, .T. ) ;
#13688 = AXIS2_PLACEMENT_3D ( 'NONE', #37604, #17375, #7722 ) ;
#13689 = CARTESIAN_POINT ( 'NONE',  ( 0.000000000000000000, 0.000000000000000000, 0.000000000000000000 ) ) ;
#13690 = DIRECTION ( 'NONE',  ( 1.000000000000000000, 0.000000000000000000, 0.000000000000000000 ) ) ;
#13691 = CIRCLE ( 'NONE', #9462, 12.55910585664918422 ) ;
#13692 = CARTESIAN_POINT ( 'NONE',  ( -21.36651465564686703, 31.00000000000000355, 43.35257367405362317 ) ) ;
#13693 = CARTESIAN_POINT ( 'NONE',  ( 17.99999999999999645, 0.000000000000000000, 0.000000000000000000 ) ) ;
#13695 = ORIENTED_EDGE ( 'NONE', *, *, #27567, .T. ) ;
#13694 = AXIS2_PLACEMENT_3D ( 'NONE', #41191, #27486, #30328 ) ;
#13696 = CIRCLE ( 'NONE', #12292, 2.649999999999971934 ) ;
#13697 = EDGE_CURVE ( 'NONE', #22079, #21461, #16934, .T. ) ;
#13699 = AXIS2_PLACEMENT_3D ( 'NONE', #17721, #30992, #31435 ) ;
#13698 = DIRECTION ( 'NONE',  ( 1.000000000000000000, -0.000000000000000000, -0.000000000000000000 ) ) ;
#13700 = ORIENTED_EDGE ( 'NONE', *, *, #14633, .F. ) ;
#13701 = CARTESIAN_POINT ( 'NONE',  ( 6.381360069253262601, 31.00000000000000355, 97.39583333395333398 ) ) ;
#13702 = VERTEX_POINT ( 'NONE', #10791 ) ;
#13703 = DIRECTION ( 'NONE',  ( -1.000000000000000000, 0.000000000000000000, 0.000000000000000000 ) ) ;
#13704 = CARTESIAN_POINT ( 'NONE',  ( -63.15125318179580205, 31.00000000000000711, -36.59163237598400542 ) ) ;
#13705 = CARTESIAN_POINT ( 'NONE',  ( -81.27520743796613090, 40.00000000000000711, 10.59408403753070083 ) ) ;
#13706 = CYLINDRICAL_SURFACE ( 'NONE', #21652, 59.00000000000000000 ) ;
#13707 = EDGE_CURVE ( 'NONE', #14373, #40885, #27824, .T. ) ;
#13708 = ORIENTED_EDGE ( 'NONE', *, *, #17174, .F. ) ;
#13709 = DIRECTION ( 'NONE',  ( 0.000000000000000000, 0.000000000000000000, 1.000000000000000000 ) ) ;
#13710 = VERTEX_POINT ( 'NONE', #30655 ) ;
#13711 = DIRECTION ( 'NONE',  ( -1.000000000000000000, -0.000000000000000000, 0.000000000000000000 ) ) ;
#13712 = EDGE_CURVE ( 'NONE', #1657, #39558, #24429, .T. ) ;
#13713 = CARTESIAN_POINT ( 'NONE',  ( 0.000000000000000000, 12.43843445475317822, 111.5058645182329968 ) ) ;
#13714 = CIRCLE ( 'NONE', #25564, 51.99999999999999289 ) ;
#13716 = EDGE_LOOP ( 'NONE', ( #23230, #17825, #4623, #39231 ) ) ;
#13715 = DIRECTION ( 'NONE',  ( 0.000000000000000000, -0.9618256431728219313, 0.2736629900720728981 ) ) ;
#13717 = EDGE_CURVE ( 'NONE', #23467, #30139, #28344, .T. ) ;
#13718 = CIRCLE ( 'NONE', #42231, 58.99999999999998579 ) ;
#13719 = DIRECTION ( 'NONE',  ( -1.000000000000000000, 0.000000000000000000, 0.000000000000000000 ) ) ;
#13721 = VERTEX_POINT ( 'NONE', #14085 ) ;
#13720 = CIRCLE ( 'NONE', #24898, 120.5010000000000474 ) ;
#13722 = DIRECTION ( 'NONE',  ( -1.000000000000000000, 0.000000000000000000, 0.000000000000000000 ) ) ;
#13723 = VECTOR ( 'NONE', #8630, 1000.000000000000000 ) ;
#13724 = CARTESIAN_POINT ( 'NONE',  ( 66.75212336275305347, 39.99999999999999289, -51.21939497476837744 ) ) ;
#13725 = LINE ( 'NONE', #3426, #30557 ) ;
#13726 = VERTEX_POINT ( 'NONE', #11231 ) ;
#13727 = LINE ( 'NONE', #13505, #24844 ) ;
#13728 = CYLINDRICAL_SURFACE ( 'NONE', #11336, 59.00000000000000000 ) ;
#13729 = AXIS2_PLACEMENT_3D ( 'NONE', #42641, #22424, #6227 ) ;
#13730 = ORIENTED_EDGE ( 'NONE', *, *, #14202, .T. ) ;
#13731 = VECTOR ( 'NONE', #599, 1000.000000000000000 ) ;
#13732 = DIRECTION ( 'NONE',  ( -1.000000000000000000, -0.000000000000000000, -0.000000000000000000 ) ) ;
#13733 = ORIENTED_EDGE ( 'NONE', *, *, #7219, .T. ) ;
#13734 = FACE_OUTER_BOUND ( 'NONE', #9370, .T. ) ;
#13736 = ORIENTED_EDGE ( 'NONE', *, *, #23973, .T. ) ;
#13735 = ADVANCED_FACE ( 'NONE', ( #519 ), #30437, .F. ) ;
#13737 = CARTESIAN_POINT ( 'NONE',  ( 19.49047152472583022, 40.00000000000000000, -17.07028940128360617 ) ) ;
#13738 = FACE_OUTER_BOUND ( 'NONE', #13609, .T. ) ;
#13739 = CARTESIAN_POINT ( 'NONE',  ( 18.00000000000000355, -11.46872990052412788, 45.56340405422441364 ) ) ;
#13740 = EDGE_CURVE ( 'NONE', #2759, #38321, #33843, .T. ) ;
#13741 = MANIFOLD_SOLID_BREP ( 'Bore', #5156 ) ;
#13742 = LINE ( 'NONE', #34417, #21992 ) ;
#13743 = CARTESIAN_POINT ( 'NONE',  ( 4.000000000000000000, -1.084202172485504434E-14, -3.142992957459231906 ) ) ;
#13744 = ORIENTED_EDGE ( 'NONE', *, *, #18614, .F. ) ;
#13746 = CARTESIAN_POINT ( 'NONE',  ( 0.000000000000000000, 107.5680526044915410, 31.89649718262280231 ) ) ;
#13745 = DIRECTION ( 'NONE',  ( 0.000000000000000000, 0.000000000000000000, 1.000000000000000000 ) ) ;
#13747 = ORIENTED_EDGE ( 'NONE', *, *, #4876, .T. ) ;
#13748 = DIRECTION ( 'NONE',  ( -1.000000000000000000, -0.000000000000000000, -0.000000000000000000 ) ) ;
#13749 = CARTESIAN_POINT ( 'NONE',  ( 0.000000000000000000, 63.55543939553896848, -97.03971415477259654 ) ) ;
#13751 = ORIENTED_EDGE ( 'NONE', *, *, #17550, .F. ) ;
#13750 = VECTOR ( 'NONE', #41360, 1000.000000000000000 ) ;
#13752 = DIRECTION ( 'NONE',  ( 1.058513553088275437E-16, 1.000000000000000000, -8.813324511995299047E-17 ) ) ;
#13753 = CARTESIAN_POINT ( 'NONE',  ( -4.197393957002303999, -7.773935952363655451E-14, -3.503767560748929810 ) ) ;
#13754 = VECTOR ( 'NONE', #9013, 1000.000000000000000 ) ;
#13755 = DIRECTION ( 'NONE',  ( 0.000000000000000000, 0.9822872507286879440, 0.1873813145857286533 ) ) ;
#13756 = CARTESIAN_POINT ( 'NONE',  ( 52.51402048354923835, 31.00000000000000355, 40.27907379435107060 ) ) ;
#13757 = AXIS2_PLACEMENT_3D ( 'NONE', #20019, #2927, #26328 ) ;
#13758 = VERTEX_POINT ( 'NONE', #3561 ) ;
#13760 = CARTESIAN_POINT ( 'NONE',  ( 29.49207856985708176, 31.00000000000000355, 38.57905506995707867 ) ) ;
#13759 = AXIS2_PLACEMENT_3D ( 'NONE', #37825, #7943, #12107 ) ;
#13761 = CIRCLE ( 'NONE', #9567, 47.49900000000000233 ) ;
#13762 = CARTESIAN_POINT ( 'NONE',  ( 74.89583333416871369, 39.99999999999999289, -4.908738512848213276 ) ) ;
#13763 = CIRCLE ( 'NONE', #7375, 31.49899999999999878 ) ;
#13764 = ADVANCED_FACE ( 'NONE', ( #7280 ), #4000, .F. ) ;
#13765 = CARTESIAN_POINT ( 'NONE',  ( 0.000000000000000000, 0.000000000000000000, 0.000000000000000000 ) ) ;
#13766 = DIRECTION ( 'NONE',  ( 0.000000000000000000, 0.000000000000000000, 1.000000000000000000 ) ) ;
#13767 = ADVANCED_FACE ( 'NONE', ( #277 ), #18454, .F. ) ;
#13768 = EDGE_LOOP ( 'NONE', ( #39089, #40273, #20241, #11360 ) ) ;
#13769 = CARTESIAN_POINT ( 'NONE',  ( 53.30287614962722387, -34.05525454449571754, 69.29271901957299917 ) ) ;
#13770 = CYLINDRICAL_SURFACE ( 'NONE', #9790, 120.5010000000000190 ) ;
#13771 = PRODUCT_DEFINITION_SHAPE ( 'NONE', 'NONE',  #43189 ) ;
#13772 = ORIENTED_EDGE ( 'NONE', *, *, #38687, .F. ) ;
#13773 = CARTESIAN_POINT ( 'NONE',  ( 40.56819808336118882, 40.00000000000000000, -35.59309480518532354 ) ) ;
#13774 = CARTESIAN_POINT ( 'NONE',  ( 0.000000000000000000, -40.37724737309996215, -104.6802291180871265 ) ) ;
#13775 = CARTESIAN_POINT ( 'NONE',  ( 0.000000000000000000, 0.000000000000000000, 0.000000000000000000 ) ) ;
#13776 = ORIENTED_EDGE ( 'NONE', *, *, #28768, .F. ) ;
#13777 = CIRCLE ( 'NONE', #5381, 116.0000000000000000 ) ;
#13778 = CYLINDRICAL_SURFACE ( 'NONE', #2907, 120.5010000000000190 ) ;
#13779 = DIRECTION ( 'NONE',  ( 0.000000000000000000, 0.5264321628773506179, 0.8502171357296174348 ) ) ;
#13780 = EDGE_LOOP ( 'NONE', ( #18418, #2473, #14084, #36482 ) ) ;
#13781 = CARTESIAN_POINT ( 'NONE',  ( 9.000000000000001776, 25.18647942089895153, -113.2326863338525271 ) ) ;
#13782 = VERTEX_POINT ( 'NONE', #21526 ) ;
#13783 = AXIS2_PLACEMENT_3D ( 'NONE', #23007, #225, #33634 ) ;
#13784 = AXIS2_PLACEMENT_3D ( 'NONE', #41047, #11409, #11199 ) ;
#13785 = AXIS2_PLACEMENT_3D ( 'NONE', #23634, #20151, #36666 ) ;
#13786 = LINE ( 'NONE', #21209, #28138 ) ;
#13787 = VERTEX_POINT ( 'NONE', #21733 ) ;
#13788 = AXIS2_PLACEMENT_3D ( 'NONE', #25268, #32203, #25898 ) ;
#13789 = DIRECTION ( 'NONE',  ( 0.000000000000000000, -0.5000000000000009992, -0.8660254037844380415 ) ) ;
#13790 = VECTOR ( 'NONE', #34793, 1000.000000000000000 ) ;
#13791 = EDGE_CURVE ( 'NONE', #24778, #32443, #31510, .T. ) ;
#13792 = CARTESIAN_POINT ( 'NONE',  ( -61.59955500562279695, 31.00000000000000711, -70.40623950599746195 ) ) ;
#13793 = ORIENTED_EDGE ( 'NONE', *, *, #29946, .F. ) ;
#13794 = CYLINDRICAL_SURFACE ( 'NONE', #32828, 14.99999999999999822 ) ;
#13795 = ADVANCED_FACE ( 'NONE', ( #25214, #24780 ), #28039, .T. ) ;
#13796 = AXIS2_PLACEMENT_3D ( 'NONE', #9444, #9872, #35826 ) ;
#13797 = EDGE_CURVE ( 'NONE', #32816, #31641, #8578, .T. ) ;
#13798 = ADVANCED_FACE ( 'NONE', ( #31299 ), #28680, .T. ) ;
#13799 = DIRECTION ( 'NONE',  ( -1.000000000000000000, -0.000000000000000000, -0.000000000000000000 ) ) ;
#13800 = CARTESIAN_POINT ( 'NONE',  ( -91.96080130434573618, -34.05525454449571043, 14.45886780445633946 ) ) ;
#13801 = ORIENTED_EDGE ( 'NONE', *, *, #33405, .F. ) ;
#13802 = DIRECTION ( 'NONE',  ( 0.000000000000000000, 0.000000000000000000, 1.000000000000000000 ) ) ;
#13803 = PLANE ( 'NONE',  #29021 ) ;
#13805 = FACE_OUTER_BOUND ( 'NONE', #31384, .T. ) ;
#13804 = DIRECTION ( 'NONE',  ( 0.000000000000000000, 0.000000000000000000, -1.000000000000000000 ) ) ;
#13806 = CARTESIAN_POINT ( 'NONE',  ( 0.000000000000000000, 28.35267316522815406, -22.18391138608678403 ) ) ;
#13807 = ORIENTED_EDGE ( 'NONE', *, *, #39418, .F. ) ;
#13808 = CARTESIAN_POINT ( 'NONE',  ( 1.053186171485216370E-12, 1.999999999999996669, 150.5000000000000284 ) ) ;
#13809 = DIRECTION ( 'NONE',  ( 0.000000000000000000, 0.000000000000000000, 1.000000000000000000 ) ) ;
#13810 = CARTESIAN_POINT ( 'NONE',  ( -2.781618486875174767, 31.00000000000000355, -42.39583333490362804 ) ) ;
#13811 = ORIENTED_EDGE ( 'NONE', *, *, #32788, .F. ) ;
#13812 = DIRECTION ( 'NONE',  ( -1.000000000000000000, 0.000000000000000000, 0.000000000000000000 ) ) ;
#13813 = CARTESIAN_POINT ( 'NONE',  ( 0.000000000000000000, -31.11570115861498920, 4.898994019976531611 ) ) ;
#13814 = CIRCLE ( 'NONE', #11729, 36.00000000000000000 ) ;
#13815 = ORIENTED_EDGE ( 'NONE', *, *, #8445, .T. ) ;
#13816 = DIRECTION ( 'NONE',  ( -3.009274222672345096E-17, -1.000000000000000000, 2.455023325076454960E-18 ) ) ;
#13817 = CARTESIAN_POINT ( 'NONE',  ( 42.89889459577944564, 40.00000000000000000, -32.91970121835214513 ) ) ;
#13818 = CONICAL_SURFACE ( 'NONE', #11039, 2.059999999999998721, 0.9599310885968738161 ) ;
#13819 = CARTESIAN_POINT ( 'NONE',  ( 30.22238470470974292, 40.00000000000000000, -34.33595424619393555 ) ) ;
#13820 = AXIS2_PLACEMENT_3D ( 'NONE', #17501, #27083, #10482 ) ;
#13821 = EDGE_CURVE ( 'NONE', #6418, #28542, #38726, .T. ) ;
#13822 = CIRCLE ( 'NONE', #7529, 13.60000000000000142 ) ;
#13823 = EDGE_LOOP ( 'NONE', ( #23386, #24358, #34795, #28290 ) ) ;
#13824 = FACE_OUTER_BOUND ( 'NONE', #40727, .T. ) ;
#13825 = DIRECTION ( 'NONE',  ( -1.000000000000000000, 0.000000000000000000, 0.000000000000000000 ) ) ;
#13826 = AXIS2_PLACEMENT_3D ( 'NONE', #39316, #42968, #36640 ) ;
#13827 = CARTESIAN_POINT ( 'NONE',  ( 18.00000000000000355, 11.46872990052381880, 45.56340405422447049 ) ) ;
#13828 = EDGE_LOOP ( 'NONE', ( #11126, #8285 ) ) ;
#13829 = CARTESIAN_POINT ( 'NONE',  ( 8.699408683037360035, 40.00000000000000000, 25.59862650653646909 ) ) ;
#13830 = VERTEX_POINT ( 'NONE', #12096 ) ;
#13831 = CARTESIAN_POINT ( 'NONE',  ( 9.000000000000001776, -113.8630351447207119, 22.16324045874372572 ) ) ;
#13832 = CARTESIAN_POINT ( 'NONE',  ( 17.99999999999999645, 84.62908780824989208, -85.78116633471202590 ) ) ;
#13833 = ORIENTED_EDGE ( 'NONE', *, *, #4989, .F. ) ;
#13834 = CYLINDRICAL_SURFACE ( 'NONE', #23566, 59.00000000000000000 ) ;
#13835 = CARTESIAN_POINT ( 'NONE',  ( 125.9999999999992184, 8.256396357209550266E-13, 369.6955262170047263 ) ) ;
#13836 = ORIENTED_EDGE ( 'NONE', *, *, #33121, .T. ) ;
#13837 = CYLINDRICAL_SURFACE ( 'NONE', #4689, 120.5010000000000190 ) ;
#13838 = ORIENTED_EDGE ( 'NONE', *, *, #16361, .T. ) ;
#13839 = CARTESIAN_POINT ( 'NONE',  ( 17.99999999999999645, 119.8996782608631406, -12.02323392193236629 ) ) ;
#13840 = ORIENTED_EDGE ( 'NONE', *, *, #9099, .T. ) ;
#13842 = VERTEX_POINT ( 'NONE', #14951 ) ;
#13841 = DIRECTION ( 'NONE',  ( 0.000000000000000000, 0.05322217484217877520, -0.9985826956767620555 ) ) ;
#13843 = CARTESIAN_POINT ( 'NONE',  ( -59.29355402628473115, 31.00000000000000355, -20.23837177251482800 ) ) ;
#13844 = ORIENTED_EDGE ( 'NONE', *, *, #40250, .T. ) ;
#13845 = CARTESIAN_POINT ( 'NONE',  ( 0.000000000000000000, -34.78944633786272789, -9.257128253673986507 ) ) ;
#13847 = EDGE_CURVE ( 'NONE', #41179, #8111, #6680, .T. ) ;
#13846 = CIRCLE ( 'NONE', #28456, 58.99999999999999289 ) ;
#13848 = AXIS2_PLACEMENT_3D ( 'NONE', #10255, #6971, #7183 ) ;
#13849 = EDGE_CURVE ( 'NONE', #13442, #42855, #28254, .T. ) ;
#13850 = EDGE_CURVE ( 'NONE', #31429, #27234, #5529, .T. ) ;
#13851 = VECTOR ( 'NONE', #29425, 1000.000000000000000 ) ;
#13852 = EDGE_LOOP ( 'NONE', ( #42079, #43122, #28634, #26240 ) ) ;
#13853 = DIRECTION ( 'NONE',  ( -1.000000000000000000, -0.000000000000000000, 0.000000000000000000 ) ) ;
#13854 = ADVANCED_FACE ( 'NONE', ( #41950 ), #41519, .F. ) ;
#13855 = EDGE_LOOP ( 'NONE', ( #38370, #28080, #33278, #29803, #22932 ) ) ;
#13856 = AXIS2_PLACEMENT_3D ( 'NONE', #5716, #15570, #8564 ) ;
#13857 = CARTESIAN_POINT ( 'NONE',  ( -37.02054590706428172, 40.00000000000000000, -75.34311506435015815 ) ) ;
#13858 = CIRCLE ( 'NONE', #5453, 2.649999999999971934 ) ;
#13860 = CARTESIAN_POINT ( 'NONE',  ( 0.000000000000000000, 0.000000000000000000, 0.000000000000000000 ) ) ;
#13859 = CARTESIAN_POINT ( 'NONE',  ( 17.99999999999999645, 71.21168426767107462, 86.70160608319346807 ) ) ;
#13861 = CARTESIAN_POINT ( 'NONE',  ( 9.000000000000001776, -114.8812324315174038, -16.07179003769264369 ) ) ;
#13862 = ORIENTED_EDGE ( 'NONE', *, *, #21843, .F. ) ;
#13863 = CARTESIAN_POINT ( 'NONE',  ( 0.000000000000000000, -29.86146780999875716, -112.0905559814581665 ) ) ;
#13864 = ORIENTED_EDGE ( 'NONE', *, *, #21608, .T. ) ;
#13865 = DIRECTION ( 'NONE',  ( -1.000000000000000000, -0.000000000000000000, 0.000000000000000000 ) ) ;
#13866 = LINE ( 'NONE', #10117, #19885 ) ;
#13867 = CARTESIAN_POINT ( 'NONE',  ( 36.87680687886029318, 31.00000000000000355, -74.81172728975037955 ) ) ;
#13868 = CARTESIAN_POINT ( 'NONE',  ( 0.000000000000000000, 0.000000000000000000, 0.000000000000000000 ) ) ;
#13869 = ORIENTED_EDGE ( 'NONE', *, *, #1735, .T. ) ;
#13870 = CARTESIAN_POINT ( 'NONE',  ( 18.00000000000000355, 35.20873326984080620, 31.88259874184042886 ) ) ;
#13871 = VERTEX_POINT ( 'NONE', #35414 ) ;
#13872 = PRESENTATION_STYLE_ASSIGNMENT (( #937 ) ) ;
#13873 = DIRECTION ( 'NONE',  ( 0.000000000000000000, 0.000000000000000000, 1.000000000000000000 ) ) ;
#13874 = AXIS2_PLACEMENT_3D ( 'NONE', #11145, #8064, #3901 ) ;
#13875 = FACE_OUTER_BOUND ( 'NONE', #21794, .T. ) ;
#13876 = EDGE_CURVE ( 'NONE', #9442, #28845, #32508, .T. ) ;
#13877 = CIRCLE ( 'NONE', #20875, 59.00000000000000000 ) ;
#13878 = ORIENTED_EDGE ( 'NONE', *, *, #6968, .F. ) ;
#13879 = DIRECTION ( 'NONE',  ( -1.000000000000000000, 0.000000000000000000, -0.000000000000000000 ) ) ;
#13880 = ORIENTED_EDGE ( 'NONE', *, *, #42114, .F. ) ;
#13881 = LINE ( 'NONE', #30661, #33943 ) ;
#13882 = DIRECTION ( 'NONE',  ( 0.000000000000000000, 0.000000000000000000, 1.000000000000000000 ) ) ;
#13883 = DIRECTION ( 'NONE',  ( 0.000000000000000000, -0.8477344278896649099, -0.5304209081197521769 ) ) ;
#13884 = ORIENTED_EDGE ( 'NONE', *, *, #35729, .F. ) ;
#13885 = ORIENTED_EDGE ( 'NONE', *, *, #21887, .T. ) ;
#13886 = CARTESIAN_POINT ( 'NONE',  ( -2.107686228591307694E-13, 150.5000000000013642, 10.00000000000041922 ) ) ;
#13887 = CARTESIAN_POINT ( 'NONE',  ( 17.99999999999999645, -46.83041522348427321, -101.9567785075606139 ) ) ;
#13888 = CARTESIAN_POINT ( 'NONE',  ( -91.96080130434580724, -14.05525454449570866, 14.45886780445738218 ) ) ;
#13890 = ORIENTED_EDGE ( 'NONE', *, *, #25378, .F. ) ;
#13889 = CARTESIAN_POINT ( 'NONE',  ( 106.4195705685763471, -106.4195705685744855, 6.999999999999998224 ) ) ;
#13891 = CARTESIAN_POINT ( 'NONE',  ( 21.72498709342646706, 31.00000000000000355, -28.22316639787266013 ) ) ;
#13892 = DIRECTION ( 'NONE',  ( 0.000000000000000000, 0.000000000000000000, 1.000000000000000000 ) ) ;
#13893 = EDGE_CURVE ( 'NONE', #39372, #16140, #27642, .T. ) ;
#13895 = ORIENTED_EDGE ( 'NONE', *, *, #20759, .F. ) ;
#13894 = DIRECTION ( 'NONE',  ( 0.000000000000000000, 0.9714298932647106311, -0.2373266998711118791 ) ) ;
#13896 = EDGE_CURVE ( 'NONE', #30077, #21731, #25011, .T. ) ;
#13897 = UNCERTAINTY_MEASURE_WITH_UNIT (LENGTH_MEASURE( 1.000000000000000082E-05 ), #159, 'distance_accuracy_value', 'NONE');
#13898 = EDGE_LOOP ( 'NONE', ( #8784, #11629, #12933, #26310 ) ) ;
#13899 = FACE_OUTER_BOUND ( 'NONE', #30778, .T. ) ;
#13900 = CARTESIAN_POINT ( 'NONE',  ( -33.53193138075045709, 40.00000000000000000, 38.09769221459629307 ) ) ;
#13901 = AXIS2_PLACEMENT_3D ( 'NONE', #38275, #21958, #4684 ) ;
#13902 = CIRCLE ( 'NONE', #38258, 2.055000000000000160 ) ;
#13903 = DIRECTION ( 'NONE',  ( 0.000000000000000000, 0.8951632913550604531, 0.4457383557765421944 ) ) ;
#13904 = UNCERTAINTY_MEASURE_WITH_UNIT (LENGTH_MEASURE( 1.000000000000000082E-05 ), #34536, 'distance_accuracy_value', 'NONE');
#13905 = CARTESIAN_POINT ( 'NONE',  ( 0.000000000000000000, -117.9424311864587480, -24.69967462999156282 ) ) ;
#13906 = ORIENTED_EDGE ( 'NONE', *, *, #15404, .F. ) ;
#13907 = AXIS2_PLACEMENT_3D ( 'NONE', #23655, #7024, #32993 ) ;
#13908 = DIRECTION ( 'NONE',  ( -1.000000000000000000, 0.000000000000000000, 0.000000000000000000 ) ) ;
#13909 = EDGE_CURVE ( 'NONE', #11189, #33175, #33190, .T. ) ;
#13910 = ORIENTED_EDGE ( 'NONE', *, *, #1847, .T. ) ;
#13911 = DIRECTION ( 'NONE',  ( 0.000000000000000000, 0.000000000000000000, 1.000000000000000000 ) ) ;
#13912 = LINE ( 'NONE', #4038, #12254 ) ;
#13913 = CARTESIAN_POINT ( 'NONE',  ( 52.83624534446448706, 31.00000000000000355, -14.15919354876300318 ) ) ;
#13914 = DIRECTION ( 'NONE',  ( -1.000000000000000000, -0.000000000000000000, -0.000000000000000000 ) ) ;
#13915 = VERTEX_POINT ( 'NONE', #14732 ) ;
#13916 = DIRECTION ( 'NONE',  ( -1.000000000000000000, 0.000000000000000000, 0.000000000000000000 ) ) ;
#13917 = ORIENTED_EDGE ( 'NONE', *, *, #18446, .F. ) ;
#13918 = CARTESIAN_POINT ( 'NONE',  ( 23.22631124480444598, 40.00000000000000000, -7.893869537065737241 ) ) ;
#13919 = ORIENTED_EDGE ( 'NONE', *, *, #31879, .F. ) ;
#13920 = DIRECTION ( 'NONE',  ( 0.000000000000000000, 0.000000000000000000, -1.000000000000000000 ) ) ;
#13921 = CARTESIAN_POINT ( 'NONE',  ( -4.197393957002303999, -0.8151795401431414234, -3.503767560748935139 ) ) ;
#13922 = CARTESIAN_POINT ( 'NONE',  ( -68.78002826185903018, 31.00000000000000711, -23.46745878763085358 ) ) ;
#13923 = CARTESIAN_POINT ( 'NONE',  ( 76.30724621505197547, 39.99999999999999289, -9.942258256684034734 ) ) ;
#13924 = CARTESIAN_POINT ( 'NONE',  ( 0.000000000000000000, 0.000000000000000000, 0.000000000000000000 ) ) ;
#13925 = VERTEX_POINT ( 'NONE', #38675 ) ;
#13926 = CARTESIAN_POINT ( 'NONE',  ( 0.000000000000000000, 41.62036691425679180, -113.0850832732710529 ) ) ;
#13927 = EDGE_LOOP ( 'NONE', ( #38627, #37270, #25739, #29730 ) ) ;
#13928 = AXIS2_PLACEMENT_3D ( 'NONE', #26809, #16145, #40080 ) ;
#13929 = DIRECTION ( 'NONE',  ( 0.000000000000000000, 0.8443279255020162966, -0.5358267949789948803 ) ) ;
#13930 = CARTESIAN_POINT ( 'NONE',  ( 0.000000000000000000, 0.000000000000000000, 0.000000000000000000 ) ) ;
#13931 = AXIS2_PLACEMENT_3D ( 'NONE', #38917, #16244, #15820 ) ;
#13933 = ORIENTED_EDGE ( 'NONE', *, *, #22030, .T. ) ;
#13932 = LINE ( 'NONE', #40499, #17950 ) ;
#13934 = DIRECTION ( 'NONE',  ( 0.000000000000000000, 0.000000000000000000, 1.000000000000000000 ) ) ;
#13935 = ORIENTED_EDGE ( 'NONE', *, *, #685, .T. ) ;
#13936 = CARTESIAN_POINT ( 'NONE',  ( 2.171643655288379993, -3.365003104552334978, -1.195831703456429434E-14 ) ) ;
#13937 = CIRCLE ( 'NONE', #17443, 120.5010000000000474 ) ;
#13938 = CARTESIAN_POINT ( 'NONE',  ( 26.74431375183570481, 40.00000000000000000, -78.78324499025107741 ) ) ;
#13939 = CARTESIAN_POINT ( 'NONE',  ( 0.000000000000000000, 12.42760411676086818, -33.78690065568411427 ) ) ;
#13940 = ORIENTED_EDGE ( 'NONE', *, *, #15058, .F. ) ;
#13941 = CARTESIAN_POINT ( 'NONE',  ( 17.99999999999999645, -29.09613215194468339, -21.19941258140352858 ) ) ;
#13942 = LINE ( 'NONE', #7361, #9937 ) ;
#13943 = ADVANCED_FACE ( 'NONE', ( #15586 ), #12307, .T. ) ;
#13944 = VERTEX_POINT ( 'NONE', #18039 ) ;
#13945 = EDGE_CURVE ( 'NONE', #24349, #39974, #8812, .T. ) ;
#13946 = CARTESIAN_POINT ( 'NONE',  ( -12.69999999999999929, 0.000000000000000000, 0.000000000000000000 ) ) ;
#13947 = EDGE_LOOP ( 'NONE', ( #37921, #13175, #12897, #4626 ) ) ;
#13948 = FACE_OUTER_BOUND ( 'NONE', #26219, .T. ) ;
#13949 = ORIENTED_EDGE ( 'NONE', *, *, #9584, .F. ) ;
#13950 = CARTESIAN_POINT ( 'NONE',  ( -10.00000000000000000, 0.000000000000000000, 0.000000000000000000 ) ) ;
#13951 = CARTESIAN_POINT ( 'NONE',  ( 17.99999999999999645, 51.98489025774451733, -108.7109110710156159 ) ) ;
#13952 = CARTESIAN_POINT ( 'NONE',  ( 18.00000000000000355, -41.20225022064653331, 23.63323037071389621 ) ) ;
#13953 = CARTESIAN_POINT ( 'NONE',  ( 18.00000000000000355, 0.000000000000000000, 0.000000000000000000 ) ) ;
#13954 = DIRECTION ( 'NONE',  ( 0.000000000000000000, -0.9911528310040084166, 0.1327255272837126743 ) ) ;
#13955 = VERTEX_POINT ( 'NONE', #9220 ) ;
#13957 = DIRECTION ( 'NONE',  ( 0.000000000000000000, 1.787647243040506224E-14, -1.000000000000000000 ) ) ;
#13956 = DIRECTION ( 'NONE',  ( 0.000000000000000000, 0.9957341762950341346, 0.09226835946330559646 ) ) ;
#13958 = EDGE_CURVE ( 'NONE', #15836, #287, #18618, .T. ) ;
#13959 = ORIENTED_EDGE ( 'NONE', *, *, #32860, .T. ) ;
#13960 = AXIS2_PLACEMENT_3D ( 'NONE', #15268, #19170, #28561 ) ;
#13961 = DIRECTION ( 'NONE',  ( -1.000000000000000000, -0.000000000000000000, -0.000000000000000000 ) ) ;
#13962 = ADVANCED_FACE ( 'NONE', ( #33211 ), #5939, .F. ) ;
#13964 = CARTESIAN_POINT ( 'NONE',  ( 11.86982580658625075, 31.00000000000000355, 24.05989836594520526 ) ) ;
#13963 = VECTOR ( 'NONE', #31914, 1000.000000000000000 ) ;
#13965 = EDGE_LOOP ( 'NONE', ( #21962, #13302, #4339, #4539 ) ) ;
#13966 = CARTESIAN_POINT ( 'NONE',  ( 17.99999999999999645, -57.40245293794732362, 96.40140491896615060 ) ) ;
#13967 = CARTESIAN_POINT ( 'NONE',  ( 8.999999999999998224, -69.72480978690109055, 92.70626138605992139 ) ) ;
#13968 = FACE_OUTER_BOUND ( 'NONE', #40907, .T. ) ;
#13969 = CARTESIAN_POINT ( 'NONE',  ( 62.17703816010947548, 31.00000000000000000, 21.10553973062999589 ) ) ;
#13970 = VERTEX_POINT ( 'NONE', #12947 ) ;
#13971 = CARTESIAN_POINT ( 'NONE',  ( 14.57966847436265212, 31.00000000000000355, -42.69519604896471776 ) ) ;
#13972 = CARTESIAN_POINT ( 'NONE',  ( 26.74431375183570481, 40.00000000000000000, -78.78324499025107741 ) ) ;
#13973 = ADVANCED_FACE ( 'NONE', ( #19721 ), #16673, .F. ) ;
#13974 = DIRECTION ( 'NONE',  ( -1.000000000000000000, -0.000000000000000000, -0.000000000000000000 ) ) ;
#13975 = AXIS2_PLACEMENT_3D ( 'NONE', #3659, #40097, #19450 ) ;
#13976 = CARTESIAN_POINT ( 'NONE',  ( 0.000000000000000000, -71.21168426767047777, -86.70160608319397966 ) ) ;
#13977 = ADVANCED_FACE ( 'NONE', ( #43016 ), #19087, .F. ) ;
#13978 = DIRECTION ( 'NONE',  ( -1.000000000000000000, 0.000000000000000000, 0.000000000000000000 ) ) ;
#13979 = ORIENTED_EDGE ( 'NONE', *, *, #33578, .F. ) ;
#13980 = DIRECTION ( 'NONE',  ( 0.000000000000000000, 0.000000000000000000, 1.000000000000000000 ) ) ;
#13981 = DIRECTION ( 'NONE',  ( 1.000000000000000000, 0.000000000000000000, 0.000000000000000000 ) ) ;
#13982 = ORIENTED_EDGE ( 'NONE', *, *, #22086, .T. ) ;
#13983 = CARTESIAN_POINT ( 'NONE',  ( 7.506055610550203205, 40.00000000000000000, 56.92102948000351148 ) ) ;
#13984 = CYLINDRICAL_SURFACE ( 'NONE', #6240, 120.5010000000000190 ) ;
#13986 = CARTESIAN_POINT ( 'NONE',  ( -31.75000000000000000, 0.000000000000000000, 0.000000000000000000 ) ) ;
#13985 = AXIS2_PLACEMENT_3D ( 'NONE', #3302, #36466, #40988 ) ;
#13987 = CIRCLE ( 'NONE', #1404, 20.00000000000000355 ) ;
#13988 = EDGE_LOOP ( 'NONE', ( #7877, #692, #32063, #17365 ) ) ;
#13989 = CIRCLE ( 'NONE', #37655, 47.49900000000000233 ) ;
#13990 = DIRECTION ( 'NONE',  ( 1.000000000000000000, -0.000000000000000000, 0.000000000000000000 ) ) ;
#13991 = FACE_OUTER_BOUND ( 'NONE', #35822, .T. ) ;
#13992 = AXIS2_PLACEMENT_3D ( 'NONE', #11796, #25124, #8487 ) ;
#13993 = ORIENTED_EDGE ( 'NONE', *, *, #41711, .F. ) ;
#13994 = DIRECTION ( 'NONE',  ( 1.000000000000000000, 0.000000000000000000, 0.000000000000000000 ) ) ;
#13995 = ORIENTED_EDGE ( 'NONE', *, *, #28986, .F. ) ;
#13996 = FACE_OUTER_BOUND ( 'NONE', #9470, .T. ) ;
#13997 = ORIENTED_EDGE ( 'NONE', *, *, #24195, .F. ) ;
#13998 = DIRECTION ( 'NONE',  ( 0.000000000000000000, 0.000000000000000000, 1.000000000000000000 ) ) ;
#13999 = CARTESIAN_POINT ( 'NONE',  ( 17.99999999999999645, 114.8812324315175033, 16.07179003769187986 ) ) ;
#14000 = EDGE_LOOP ( 'NONE', ( #3538, #41211, #4527, #13844 ) ) ;
#14001 = DIRECTION ( 'NONE',  ( -1.000000000000000000, 0.000000000000000000, -0.000000000000000000 ) ) ;
#14002 = EDGE_CURVE ( 'NONE', #39508, #41141, #10911, .T. ) ;
#14003 = DIRECTION ( 'NONE',  ( 1.000000000000000000, 0.000000000000000000, 0.000000000000000000 ) ) ;
#14004 = EDGE_LOOP ( 'NONE', ( #24206, #40583, #22569, #23313 ) ) ;
#14005 = CARTESIAN_POINT ( 'NONE',  ( 17.99999999999999645, 120.2856157092986678, 7.201503623197233139 ) ) ;
#14006 = EDGE_CURVE ( 'NONE', #16643, #34774, #22802, .T. ) ;
#14007 = DIRECTION ( 'NONE',  ( -1.000000000000000000, 0.000000000000000000, 0.000000000000000000 ) ) ;
#14008 = CIRCLE ( 'NONE', #22780, 59.00000000000000000 ) ;
#14009 = ADVANCED_FACE ( 'NONE', ( #19509, #3066 ), #2434, .T. ) ;
#14010 = CARTESIAN_POINT ( 'NONE',  ( 0.000000000000000000, -78.18175027177490222, 85.69488855492974722 ) ) ;
#14011 = CIRCLE ( 'NONE', #15402, 36.00000000000000000 ) ;
#14012 = CARTESIAN_POINT ( 'NONE',  ( 0.000000000000000000, 100.8494052988179561, -65.95368414178808791 ) ) ;
#14013 = VERTEX_POINT ( 'NONE', #12 ) ;
#14014 = DIRECTION ( 'NONE',  ( 6.123233995736766036E-17, 1.000000000000000000, 0.000000000000000000 ) ) ;
#14015 = CARTESIAN_POINT ( 'NONE',  ( 17.99999999999999645, -110.3490479609630910, 38.71798610214488434 ) ) ;
#14016 = CARTESIAN_POINT ( 'NONE',  ( 2.454369252093185239, 31.00000000000000355, 37.39583333513270702 ) ) ;
#14017 = CIRCLE ( 'NONE', #36271, 36.00000000000000000 ) ;
#14018 = ORIENTED_EDGE ( 'NONE', *, *, #27198, .F. ) ;
#14019 = DIRECTION ( 'NONE',  ( -1.058513553088275437E-16, -1.000000000000000000, 8.813324511995299047E-17 ) ) ;
#14020 = AXIS2_PLACEMENT_3D ( 'NONE', #32378, #28708, #41974 ) ;
#14021 = AXIS2_PLACEMENT_3D ( 'NONE', #17673, #14376, #40729 ) ;
#14022 = DIRECTION ( 'NONE',  ( -1.000000000000000000, 0.000000000000000000, 0.000000000000000000 ) ) ;
#14023 = ORIENTED_EDGE ( 'NONE', *, *, #4159, .F. ) ;
#14024 = MANIFOLD_SOLID_BREP ( 'Bore', #3778 ) ;
#14025 = AXIS2_PLACEMENT_3D ( 'NONE', #40292, #26793, #355 ) ;
#14026 = DIRECTION ( 'NONE',  ( -1.807003620809174385E-16, 1.000000000000000000, 0.000000000000000000 ) ) ;
#14027 = CARTESIAN_POINT ( 'NONE',  ( -32.14164714139042189, 40.00000000000000000, 36.65395011347077059 ) ) ;
#14028 = CARTESIAN_POINT ( 'NONE',  ( -55.11358496761538106, 40.00000000000000711, 27.06326608206703099 ) ) ;
#14029 = AXIS2_PLACEMENT_3D ( 'NONE', #3222, #9793, #13745 ) ;
#14030 = ORIENTED_EDGE ( 'NONE', *, *, #226, .F. ) ;
#14031 = DIRECTION ( 'NONE',  ( -1.000000000000000000, -0.000000000000000000, -0.000000000000000000 ) ) ;
#14032 = DIRECTION ( 'NONE',  ( -1.000000000000000000, -0.000000000000000000, -0.000000000000000000 ) ) ;
#14033 = EDGE_CURVE ( 'NONE', #20369, #20160, #35812, .T. ) ;
#14034 = EDGE_CURVE ( 'NONE', #20730, #20374, #3201, .T. ) ;
#14035 = CARTESIAN_POINT ( 'NONE',  ( 0.000000000000000000, -0.6168405712489287707, 35.99471499692226217 ) ) ;
#14036 = CARTESIAN_POINT ( 'NONE',  ( 0.000000000000000000, 0.000000000000000000, -1.199999999999999956 ) ) ;
#14037 = VERTEX_POINT ( 'NONE', #42582 ) ;
#14038 = CARTESIAN_POINT ( 'NONE',  ( 17.96659372829068246, 40.00000000000000000, -15.76829228678407624 ) ) ;
#14039 = ORIENTED_EDGE ( 'NONE', *, *, #16011, .F. ) ;
#14040 = DIRECTION ( 'NONE',  ( 3.009274222672345096E-17, 1.000000000000000000, -2.455023325076454960E-18 ) ) ;
#14041 = DIRECTION ( 'NONE',  ( -1.000000000000000000, -0.000000000000000000, 0.000000000000000000 ) ) ;
#14042 = ORIENTED_EDGE ( 'NONE', *, *, #15961, .F. ) ;
#14043 = DIRECTION ( 'NONE',  ( -1.000000000000000000, -0.000000000000000000, 0.000000000000000000 ) ) ;
#14044 = CARTESIAN_POINT ( 'NONE',  ( 17.99999999999999645, -94.52951811191513798, -67.23221107124996365 ) ) ;
#14045 = ORIENTED_EDGE ( 'NONE', *, *, #26438, .F. ) ;
#14046 = DIRECTION ( 'NONE',  ( 1.000000000000000000, -0.000000000000000000, -0.000000000000000000 ) ) ;
#14047 = EDGE_LOOP ( 'NONE', ( #6675, #31962, #8576, #14913, #13497, #34580, #35866 ) ) ;
#14048 = AXIS2_PLACEMENT_3D ( 'NONE', #6201, #35649, #12130 ) ;
#14049 = DIRECTION ( 'NONE',  ( 0.000000000000000000, 1.000000000000000000, 0.000000000000000000 ) ) ;
#14050 = ADVANCED_FACE ( 'NONE', ( #12730 ), #31122, .T. ) ;
#14051 = VECTOR ( 'NONE', #16958, 1000.000000000000000 ) ;
#14052 = VERTEX_POINT ( 'NONE', #22787 ) ;
#14054 = EDGE_LOOP ( 'NONE', ( #38887, #21103 ) ) ;
#14053 = CARTESIAN_POINT ( 'NONE',  ( 17.99999999999999645, -111.8797445107944100, -8.437727291343872338 ) ) ;
#14055 = VECTOR ( 'NONE', #6780, 1000.000000000000000 ) ;
#14056 = CARTESIAN_POINT ( 'NONE',  ( -63.15125318179580205, 31.00000000000000711, -36.59163237598400542 ) ) ;
#14057 = ORIENTED_EDGE ( 'NONE', *, *, #2892, .F. ) ;
#14058 = DIRECTION ( 'NONE',  ( 0.000000000000000000, -0.6845471059286792892, -0.7289686274214203232 ) ) ;
#14059 = CIRCLE ( 'NONE', #38410, 2.649999999999971934 ) ;
#14060 = EDGE_LOOP ( 'NONE', ( #31950, #24151, #15977, #37331 ) ) ;
#14061 = PLANE ( 'NONE',  #7731 ) ;
#14062 = EDGE_CURVE ( 'NONE', #36837, #33813, #3510, .T. ) ;
#14063 = ORIENTED_EDGE ( 'NONE', *, *, #10055, .F. ) ;
#14064 = CARTESIAN_POINT ( 'NONE',  ( -11.85673204381699364, 40.00000000000000000, 89.11174773313419450 ) ) ;
#14065 = CIRCLE ( 'NONE', #19644, 20.00000000000000711 ) ;
#14066 = ADVANCED_FACE ( 'NONE', ( #3943 ), #17329, .F. ) ;
#14068 = DIRECTION ( 'NONE',  ( 0.000000000000000000, -0.9911528310040057521, -0.1327255272837325473 ) ) ;
#14067 = CYLINDRICAL_SURFACE ( 'NONE', #39827, 2.649999999999985700 ) ;
#14069 = DIRECTION ( 'NONE',  ( -1.000000000000000000, 0.000000000000000000, 0.000000000000000000 ) ) ;
#14070 = CARTESIAN_POINT ( 'NONE',  ( 18.00000000000000355, 0.000000000000000000, 0.000000000000000000 ) ) ;
#14071 = ORIENTED_EDGE ( 'NONE', *, *, #26825, .T. ) ;
#14072 = SHAPE_REPRESENTATION_RELATIONSHIP ( 'NONE' , 'NONE' ,  #39082, #3052 ) ;
#14073 = CARTESIAN_POINT ( 'NONE',  ( 17.99999999999999645, 119.7318547011703629, -13.59315897125608430 ) ) ;
#14074 = EDGE_LOOP ( 'NONE', ( #19931, #19634, #40276, #2348 ) ) ;
#14075 = CARTESIAN_POINT ( 'NONE',  ( 0.000000000000000000, 22.43957647427220081, -41.27978878573604504 ) ) ;
#14076 = CARTESIAN_POINT ( 'NONE',  ( 5.726861599741335240, 31.00000000000000355, 87.39583333411552246 ) ) ;
#14077 = PLANE ( 'NONE',  #37377 ) ;
#14078 = VERTEX_POINT ( 'NONE', #17750 ) ;
#14079 = CYLINDRICAL_SURFACE ( 'NONE', #41468, 13.60000000000000142 ) ;
#14080 = AXIS2_PLACEMENT_3D ( 'NONE', #23241, #17355, #30635 ) ;
#14081 = ORIENTED_EDGE ( 'NONE', *, *, #2796, .F. ) ;
#14082 = CIRCLE ( 'NONE', #5701, 31.49899999999999878 ) ;
#14083 = EDGE_CURVE ( 'NONE', #20422, #5066, #34590, .T. ) ;
#14084 = ORIENTED_EDGE ( 'NONE', *, *, #8389, .T. ) ;
#14085 = CARTESIAN_POINT ( 'NONE',  ( 18.00000000000000355, -24.72041153920759982, 40.55929306992680949 ) ) ;
#14086 = DIRECTION ( 'NONE',  ( 1.000000000000000000, 0.000000000000000000, 0.000000000000000000 ) ) ;
#14087 = ADVANCED_FACE ( 'NONE', ( #37121 ), #4163, .F. ) ;
#14088 = DIRECTION ( 'NONE',  ( 1.000000000000000000, 0.000000000000000000, 0.000000000000000000 ) ) ;
#14089 = ADVANCED_FACE ( 'NONE', ( #37338 ), #40592, .T. ) ;
#14090 = EDGE_CURVE ( 'NONE', #27124, #22079, #23478, .T. ) ;
#14091 = CIRCLE ( 'NONE', #802, 120.5010000000000474 ) ;
#14092 = CARTESIAN_POINT ( 'NONE',  ( 17.99999999999999645, 112.8457601792519256, -26.86697618949260402 ) ) ;
#14093 = ORIENTED_EDGE ( 'NONE', *, *, #28043, .F. ) ;
#14094 = CARTESIAN_POINT ( 'NONE',  ( 0.000000000000000000, 25.61928775981106554, -45.25098998563451147 ) ) ;
#14095 = ORIENTED_EDGE ( 'NONE', *, *, #20110, .T. ) ;
#14096 = VECTOR ( 'NONE', #10057, 1000.000000000000000 ) ;
#14097 = DIRECTION ( 'NONE',  ( 0.3211947320043981313, 0.000000000000000000, 0.9470131699890043109 ) ) ;
#14098 = LINE ( 'NONE', #17386, #17285 ) ;
#14099 = LINE ( 'NONE', #37402, #38640 ) ;
#14100 = VERTEX_POINT ( 'NONE', #33855 ) ;
#14101 = EDGE_LOOP ( 'NONE', ( #17500, #10523 ) ) ;
#14102 = LINE ( 'NONE', #10374, #31455 ) ;
#14103 = CARTESIAN_POINT ( 'NONE',  ( 17.99999999999999645, -114.8812324315176312, 16.07179003769107339 ) ) ;
#14104 = CARTESIAN_POINT ( 'NONE',  ( 4.197310751797292738, 0.8178363989516252985, -3.502498386812444409 ) ) ;
#14105 = ORIENTED_EDGE ( 'NONE', *, *, #40000, .T. ) ;
#14107 = EDGE_LOOP ( 'NONE', ( #39642, #37756, #35096, #12337 ) ) ;
#14106 = CYLINDRICAL_SURFACE ( 'NONE', #5503, 59.00000000000000000 ) ;
#14108 = CARTESIAN_POINT ( 'NONE',  ( 11.33656872182281816, 31.00000000000000355, -33.21392199183605243 ) ) ;
#14109 = DIRECTION ( 'NONE',  ( 0.000000000000000000, 0.000000000000000000, 1.000000000000000000 ) ) ;
#14111 = ORIENTED_EDGE ( 'NONE', *, *, #26225, .T. ) ;
#14110 = CARTESIAN_POINT ( 'NONE',  ( -0.2999999999999999889, -14.69693845669906906, -1.199999999999999956 ) ) ;
#14112 = VERTEX_POINT ( 'NONE', #17535 ) ;
#14113 = AXIS2_PLACEMENT_3D ( 'NONE', #12074, #26226, #8995 ) ;
#14114 = DIRECTION ( 'NONE',  ( -1.000000000000000000, -0.000000000000000000, -0.000000000000000000 ) ) ;
#14115 = CARTESIAN_POINT ( 'NONE',  ( 65.23019871244166268, 39.99999999999999289, 17.57949444736078703 ) ) ;
#14116 = CIRCLE ( 'NONE', #40536, 10.50000000000000178 ) ;
#14117 = DIRECTION ( 'NONE',  ( 0.000000000000000000, -0.8443279255020087470, -0.5358267949790065376 ) ) ;
#14118 = VECTOR ( 'NONE', #18155, 1000.000000000000000 ) ;
#14119 = DIRECTION ( 'NONE',  ( -1.000000000000000000, 0.000000000000000000, 0.000000000000000000 ) ) ;
#14120 = ORIENTED_EDGE ( 'NONE', *, *, #16228, .T. ) ;
#14121 = LINE ( 'NONE', #24161, #7693 ) ;
#14122 = ORIENTED_EDGE ( 'NONE', *, *, #19929, .F. ) ;
#14123 = AXIS2_PLACEMENT_3D ( 'NONE', #33194, #34058, #17514 ) ;
#14124 = CYLINDRICAL_SURFACE ( 'NONE', #19074, 116.0000000000000000 ) ;
#14125 = DIRECTION ( 'NONE',  ( 1.000000000000000000, 0.000000000000000000, 0.000000000000000000 ) ) ;
#14126 = CARTESIAN_POINT ( 'NONE',  ( -60.10416666555506993, 31.00000000000000711, -3.926990808566252156 ) ) ;
#14127 = DIRECTION ( 'NONE',  ( 0.000000000000000000, -0.4132121857683850874, 0.9106347728549100129 ) ) ;
#14128 = EDGE_LOOP ( 'NONE', ( #17641, #9148, #19832, #25654 ) ) ;
#14129 = DIRECTION ( 'NONE',  ( 0.000000000000000000, 0.9714298932647106311, -0.2373266998711118791 ) ) ;
#14130 = ORIENTED_EDGE ( 'NONE', *, *, #10568, .F. ) ;
#14131 = CARTESIAN_POINT ( 'NONE',  ( -14.11622541012940601, 40.00000000000000000, -16.08312669853564358 ) ) ;
#14132 = EDGE_LOOP ( 'NONE', ( #37286, #3361 ) ) ;
#14133 = CARTESIAN_POINT ( 'NONE',  ( 17.99999999999999645, 0.000000000000000000, 0.000000000000000000 ) ) ;
#14134 = DIRECTION ( 'NONE',  ( -1.000000000000000000, 0.000000000000000000, 0.000000000000000000 ) ) ;
#14135 = CARTESIAN_POINT ( 'NONE',  ( -48.39074809477736494, 31.00000000000000355, -55.33250407651094349 ) ) ;
#14136 = CARTESIAN_POINT ( 'NONE',  ( -63.15125318177969405, 40.00000000000000711, -36.59163237596791163 ) ) ;
#14137 = ADVANCED_FACE ( 'NONE', ( #460 ), #15110, .T. ) ;
#14138 = ADVANCED_FACE ( 'NONE', ( #14237 ), #1829, .T. ) ;
#14139 = CARTESIAN_POINT ( 'NONE',  ( 0.000000000000000000, -13.22719389141960100, -28.58720592780609593 ) ) ;
#14140 = ADVANCED_FACE ( 'NONE', ( #13824 ), #33426, .F. ) ;
#14141 = CIRCLE ( 'NONE', #24619, 36.00000000000000000 ) ;
#14142 = ORIENTED_EDGE ( 'NONE', *, *, #7869, .T. ) ;
#14143 = CYLINDRICAL_SURFACE ( 'NONE', #34661, 4.250000000000000000 ) ;
#14144 = ORIENTED_EDGE ( 'NONE', *, *, #19464, .F. ) ;
#14145 = FACE_OUTER_BOUND ( 'NONE', #34128, .T. ) ;
#14146 = CIRCLE ( 'NONE', #32921, 36.00000000000000000 ) ;
#14147 = CARTESIAN_POINT ( 'NONE',  ( 17.99999999999999645, 109.4038418350903470, 50.51029986767587587 ) ) ;
#14149 = ORIENTED_EDGE ( 'NONE', *, *, #28857, .T. ) ;
#14148 = DIRECTION ( 'NONE',  ( 1.000000000000000000, -0.000000000000000000, -0.000000000000000000 ) ) ;
#14150 = LINE ( 'NONE', #1239, #10788 ) ;
#14151 = ORIENTED_EDGE ( 'NONE', *, *, #37767, .T. ) ;
#14152 = CYLINDRICAL_SURFACE ( 'NONE', #7705, 59.00000000000000000 ) ;
#14153 = CARTESIAN_POINT ( 'NONE',  ( -70.15350862410126354, 40.00000000000000711, -40.50401079722123399 ) ) ;
#14154 = LINE ( 'NONE', #31368, #12496 ) ;
#14155 = VECTOR ( 'NONE', #34012, 1000.000000000000000 ) ;
#14156 = EDGE_LOOP ( 'NONE', ( #39555, #2163 ) ) ;
#14157 = EDGE_CURVE ( 'NONE', #5703, #12547, #436, .T. ) ;
#14158 = CARTESIAN_POINT ( 'NONE',  ( 18.00000000000000355, 6.109652351741791776, 46.58570277113511793 ) ) ;
#14159 = DIRECTION ( 'NONE',  ( -1.000000000000000000, 0.000000000000000000, 0.000000000000000000 ) ) ;
#14160 = ORIENTED_EDGE ( 'NONE', *, *, #33807, .T. ) ;
#14161 = ORIENTED_EDGE ( 'NONE', *, *, #11286, .F. ) ;
#14162 = DIRECTION ( 'NONE',  ( 0.000000000000000000, 0.000000000000000000, 1.000000000000000000 ) ) ;
#14163 = ORIENTED_EDGE ( 'NONE', *, *, #36153, .T. ) ;
#14164 = CARTESIAN_POINT ( 'NONE',  ( -21.70016380022027391, 40.00000000000000000, -5.809120511592388958 ) ) ;
#14165 = DIRECTION ( 'NONE',  ( -1.000000000000000000, 0.000000000000000000, 0.000000000000000000 ) ) ;
#14166 = DIRECTION ( 'NONE',  ( -3.009274222672345096E-17, -1.000000000000000000, 2.455023325076454960E-18 ) ) ;
#14167 = ADVANCED_FACE ( 'NONE', ( #4377 ), #6036, .F. ) ;
#14168 = DIRECTION ( 'NONE',  ( 0.000000000000000000, 0.1253332335642974305, 0.9921147013144787641 ) ) ;
#14169 = ORIENTED_EDGE ( 'NONE', *, *, #7103, .T. ) ;
#14171 = LINE ( 'NONE', #26013, #25567 ) ;
#14170 = DIRECTION ( 'NONE',  ( 0.000000000000000000, -0.7865515558026354714, -0.6175246149462008116 ) ) ;
#14172 = ORIENTED_EDGE ( 'NONE', *, *, #30681, .F. ) ;
#14173 = DIRECTION ( 'NONE',  ( -1.000000000000000000, -0.000000000000000000, 0.000000000000000000 ) ) ;
#14174 = CARTESIAN_POINT ( 'NONE',  ( 19.70274684888802952, 31.00000000000000355, 17.27304525429847359 ) ) ;
#14175 = VERTEX_POINT ( 'NONE', #30168 ) ;
#14176 = CARTESIAN_POINT ( 'NONE',  ( -16.80298683001096904, 17.11489954122026447, -2.367532924972506336 ) ) ;
#14177 = CARTESIAN_POINT ( 'NONE',  ( 18.00000000000000355, 11.46872990052444408, -45.56340405422433548 ) ) ;
#14178 =( GEOMETRIC_REPRESENTATION_CONTEXT ( 3 ) GLOBAL_UNCERTAINTY_ASSIGNED_CONTEXT ( ( #20903 ) ) GLOBAL_UNIT_ASSIGNED_CONTEXT ( ( #36294, #29354, #13421 ) ) REPRESENTATION_CONTEXT ( 'NONE', 'WORKASPACE' ) );
#14179 = CARTESIAN_POINT ( 'NONE',  ( 0.000000000000000000, 11.90021268425555512, 45.45261810511218670 ) ) ;
#14180 = CARTESIAN_POINT ( 'NONE',  ( -56.48955861152074220, 31.00000000000000711, -43.32902275382048174 ) ) ;
#14181 = ORIENTED_EDGE ( 'NONE', *, *, #16957, .T. ) ;
#14182 = CARTESIAN_POINT ( 'NONE',  ( 30.22238470471967631, 31.00000000000000355, -34.33595424619392844 ) ) ;
#14183 = ADVANCED_FACE ( 'NONE', ( #1112 ), #10306, .F. ) ;
#14184 = CARTESIAN_POINT ( 'NONE',  ( -53.76583044639610165, 40.00000000000000000, -61.28633540801820345 ) ) ;
#14185 = APPLICATION_CONTEXT ( 'automotive_design' ) ;
#14186 = CARTESIAN_POINT ( 'NONE',  ( 9.000000000000001776, 0.6819280456844267757, -115.9979955608738607 ) ) ;
#14187 = LINE ( 'NONE', #30553, #23570 ) ;
#14188 = CARTESIAN_POINT ( 'NONE',  ( -2.650000000000189981, 150.5000000000013642, 10.00000000000041922 ) ) ;
#14189 = EDGE_CURVE ( 'NONE', #14608, #755, #31814, .T. ) ;
#14190 = CIRCLE ( 'NONE', #24674, 59.00000000000000711 ) ;
#14192 = ORIENTED_EDGE ( 'NONE', *, *, #28082, .T. ) ;
#14191 = DIRECTION ( 'NONE',  ( 0.000000000000000000, 0.7164567402983116340, 0.6976315211349882750 ) ) ;
#14193 = LINE ( 'NONE', #13335, #6493 ) ;
#14194 = CARTESIAN_POINT ( 'NONE',  ( 17.99999999999999645, 0.000000000000000000, 0.000000000000000000 ) ) ;
#14195 = EDGE_CURVE ( 'NONE', #7227, #18461, #40384, .T. ) ;
#14196 = AXIS2_PLACEMENT_3D ( 'NONE', #9610, #35989, #9378 ) ;
#14197 = EDGE_LOOP ( 'NONE', ( #10697, #29546, #359, #38703 ) ) ;
#14198 = CARTESIAN_POINT ( 'NONE',  ( -25.79802671946675474, 40.00000000000000000, 52.34090327860478453 ) ) ;
#14199 = LINE ( 'NONE', #27496, #5535 ) ;
#14200 = CARTESIAN_POINT ( 'NONE',  ( 17.99999999999999645, 0.04937522221122418731, 31.94951095880159286 ) ) ;
#14201 = ORIENTED_EDGE ( 'NONE', *, *, #38015, .T. ) ;
#14202 = EDGE_CURVE ( 'NONE', #2350, #37579, #38113, .T. ) ;
#14203 = CARTESIAN_POINT ( 'NONE',  ( 17.99999999999999645, 0.000000000000000000, 0.000000000000000000 ) ) ;
#14204 = DIRECTION ( 'NONE',  ( 0.000000000000000000, 0.000000000000000000, 1.000000000000000000 ) ) ;
#14205 = ORIENTED_EDGE ( 'NONE', *, *, #9707, .F. ) ;
#14206 = CARTESIAN_POINT ( 'NONE',  ( 0.000000000000000000, 51.98489025774302519, 108.7109110710163549 ) ) ;
#14207 = EDGE_LOOP ( 'NONE', ( #31601, #14704, #32985, #29410 ) ) ;
#14208 = CARTESIAN_POINT ( 'NONE',  ( 18.00000000000000355, -42.03146605346801579, 22.12489237027304512 ) ) ;
#14209 = ORIENTED_EDGE ( 'NONE', *, *, #7900, .F. ) ;
#14210 = DIRECTION ( 'NONE',  ( 1.000000000000000000, -0.000000000000000000, -0.000000000000000000 ) ) ;
#14211 = DIRECTION ( 'NONE',  ( 0.000000000000000000, 0.9048270524660176894, 0.4257792915650767118 ) ) ;
#14212 = ORIENTED_EDGE ( 'NONE', *, *, #5545, .F. ) ;
#14213 = LINE ( 'NONE', #27516, #42817 ) ;
#14214 = LINE ( 'NONE', #17509, #8053 ) ;
#14216 = ORIENTED_EDGE ( 'NONE', *, *, #15129, .T. ) ;
#14215 = CIRCLE ( 'NONE', #39236, 1.000000000000000666 ) ;
#14217 = DIRECTION ( 'NONE',  ( -1.000000000000000000, -0.000000000000000000, 0.000000000000000000 ) ) ;
#14218 = EDGE_CURVE ( 'NONE', #34135, #22843, #18648, .T. ) ;
#14219 = DIRECTION ( 'NONE',  ( 0.000000000000000000, 0.9980267284282716700, -0.06279051952930995995 ) ) ;
#14220 = VECTOR ( 'NONE', #34328, 1000.000000000000000 ) ;
#14221 = DIRECTION ( 'NONE',  ( 0.000000000000000000, 0.000000000000000000, 1.000000000000000000 ) ) ;
#14222 = CARTESIAN_POINT ( 'NONE',  ( 18.00000000000000355, 0.000000000000000000, 0.000000000000000000 ) ) ;
#14223 = VERTEX_POINT ( 'NONE', #34725 ) ;
#14224 = DIRECTION ( 'NONE',  ( -1.110223024625168620E-16, -1.000000000000000000, 8.326672684688766498E-17 ) ) ;
#14226 = AXIS2_PLACEMENT_3D ( 'NONE', #24463, #17701, #31847 ) ;
#14225 = DIRECTION ( 'NONE',  ( -1.000000000000000000, 0.000000000000000000, 0.000000000000000000 ) ) ;
#14227 = CARTESIAN_POINT ( 'NONE',  ( 43.15607885788778475, 31.00000000000000355, -11.56636786368396486 ) ) ;
#14228 = VERTEX_POINT ( 'NONE', #41899 ) ;
#14230 = CARTESIAN_POINT ( 'NONE',  ( -15.99999999999997691, 40.00000000000000000, 5.571627607371296764E-15 ) ) ;
#14229 = DIRECTION ( 'NONE',  ( -1.000000000000000000, -0.000000000000000000, -0.000000000000000000 ) ) ;
#14231 = DIRECTION ( 'NONE',  ( -1.000000000000000000, 0.000000000000000000, -0.000000000000000000 ) ) ;
#14232 = ORIENTED_EDGE ( 'NONE', *, *, #26448, .T. ) ;
#14233 = DIRECTION ( 'NONE',  ( 0.000000000000000000, 0.000000000000000000, 1.000000000000000000 ) ) ;
#14234 = CARTESIAN_POINT ( 'NONE',  ( 44.50160557815096496, 40.00000000000000000, -5.869829666507492050 ) ) ;
#14235 = AXIS2_PLACEMENT_3D ( 'NONE', #11165, #33620, #17964 ) ;
#14236 = CARTESIAN_POINT ( 'NONE',  ( -45.80426865613544862, 40.00000000000000000, -26.55377233850569141 ) ) ;
#14237 = FACE_OUTER_BOUND ( 'NONE', #8185, .T. ) ;
#14238 = CARTESIAN_POINT ( 'NONE',  ( 17.99999999999999645, 0.000000000000000000, 0.000000000000000000 ) ) ;
#14239 = DIRECTION ( 'NONE',  ( -1.000000000000000000, 0.000000000000000000, 0.000000000000000000 ) ) ;
#14240 = AXIS2_PLACEMENT_3D ( 'NONE', #20729, #595, #30730 ) ;
#14241 = DIRECTION ( 'NONE',  ( -1.000000000000000000, -0.000000000000000000, -0.000000000000000000 ) ) ;
#14242 = EDGE_CURVE ( 'NONE', #29604, #17574, #19340, .T. ) ;
#14243 = ORIENTED_EDGE ( 'NONE', *, *, #5799, .F. ) ;
#14244 = CARTESIAN_POINT ( 'NONE',  ( -14.19360040536685830, 40.00000000000000000, 24.59234967646941783 ) ) ;
#14245 = EDGE_LOOP ( 'NONE', ( #9087, #26061, #6884, #1240 ) ) ;
#14246 = DIRECTION ( 'NONE',  ( 0.000000000000000000, 0.000000000000000000, 1.000000000000000000 ) ) ;
#14247 = CARTESIAN_POINT ( 'NONE',  ( -103.7695705685749772, 106.4195705685765745, 10.00000000000033573 ) ) ;
#14248 = AXIS2_PLACEMENT_3D ( 'NONE', #30866, #1602, #17806 ) ;
#14249 = ORIENTED_EDGE ( 'NONE', *, *, #27370, .F. ) ;
#14250 = DIRECTION ( 'NONE',  ( -3.009274222672345096E-17, -1.000000000000000000, 2.455023325076454960E-18 ) ) ;
#14251 = CIRCLE ( 'NONE', #42793, 52.00000000000000000 ) ;
#14252 = DIRECTION ( 'NONE',  ( -0.000000000000000000, 1.000000000000000000, 1.224646799147353207E-16 ) ) ;
#14253 = ORIENTED_EDGE ( 'NONE', *, *, #25492, .F. ) ;
#14254 = DIRECTION ( 'NONE',  ( 1.000000000000000000, 0.000000000000000000, 0.000000000000000000 ) ) ;
#14255 = VERTEX_POINT ( 'NONE', #41247 ) ;
#14256 = CARTESIAN_POINT ( 'NONE',  ( 17.99999999999999645, 0.000000000000000000, 0.000000000000000000 ) ) ;
#14257 = AXIS2_PLACEMENT_3D ( 'NONE', #12379, #22228, #35472 ) ;
#14258 = VERTEX_POINT ( 'NONE', #12049 ) ;
#14260 = VERTEX_POINT ( 'NONE', #4834 ) ;
#14259 = CARTESIAN_POINT ( 'NONE',  ( -10.00000000000000000, 0.000000000000000000, 0.000000000000000000 ) ) ;
#14261 = CARTESIAN_POINT ( 'NONE',  ( 39.32569335900156204, 31.00000000000000355, 68.32161714268157482 ) ) ;
#14262 = EDGE_LOOP ( 'NONE', ( #35236, #7407, #40307, #26642 ) ) ;
#14263 = CARTESIAN_POINT ( 'NONE',  ( -4.197312064133472020, -0.8182229787990021874, -3.502518405183886685 ) ) ;
#14264 = ORIENTED_EDGE ( 'NONE', *, *, #34915, .T. ) ;
#14265 = DIRECTION ( 'NONE',  ( -1.000000000000000000, 0.000000000000000000, 0.000000000000000000 ) ) ;
#14266 = EDGE_LOOP ( 'NONE', ( #6271, #11229, #24422, #33733 ) ) ;
#14268 = CARTESIAN_POINT ( 'NONE',  ( 93.52153384685561832, 39.99999999999999289, -24.92737483788710762 ) ) ;
#14267 = AXIS2_PLACEMENT_3D ( 'NONE', #31450, #14670, #8095 ) ;
#14269 = ADVANCED_FACE ( 'NONE', ( #21885 ), #24516, .T. ) ;
#14270 = EDGE_CURVE ( 'NONE', #25091, #8724, #35308, .T. ) ;
#14272 = DIRECTION ( 'NONE',  ( 0.000000000000000000, -0.1253332335643113360, 0.9921147013144769877 ) ) ;
#14271 = CARTESIAN_POINT ( 'NONE',  ( 18.00000000000000355, -22.43957647427129842, -41.27978878573651400 ) ) ;
#14273 = CYLINDRICAL_SURFACE ( 'NONE', #22051, 47.49900000000000233 ) ;
#14274 = CARTESIAN_POINT ( 'NONE',  ( -10.00000000000000000, 0.000000000000000000, 0.000000000000000000 ) ) ;
#14275 = CIRCLE ( 'NONE', #33775, 116.0000000000000000 ) ;
#14276 = VERTEX_POINT ( 'NONE', #31460 ) ;
#14277 = LINE ( 'NONE', #27158, #33812 ) ;
#14278 = VECTOR ( 'NONE', #29314, 1000.000000000000000 ) ;
#14279 = CARTESIAN_POINT ( 'NONE',  ( 18.00000000000000355, -39.64889472655755043, 33.64468972902493960 ) ) ;
#14280 = CARTESIAN_POINT ( 'NONE',  ( -58.57471716409879292, 31.00000000000000711, 66.78942258476980953 ) ) ;
#14281 = CARTESIAN_POINT ( 'NONE',  ( -8.920000000000003482, 0.000000000000000000, 11.08000000000000007 ) ) ;
#14282 = ORIENTED_EDGE ( 'NONE', *, *, #22573, .F. ) ;
#14283 = ADVANCED_FACE ( 'NONE', ( #14895 ), #28195, .F. ) ;
#14284 = CARTESIAN_POINT ( 'NONE',  ( 26.10672890669277990, 40.00000000000000000, 8.893381768402427667 ) ) ;
#14285 = AXIS2_PLACEMENT_3D ( 'NONE', #11459, #24795, #25025 ) ;
#14286 = EDGE_LOOP ( 'NONE', ( #15240, #6254, #3977, #7752 ) ) ;
#14287 = ORIENTED_EDGE ( 'NONE', *, *, #30448, .T. ) ;
#14288 = FACE_OUTER_BOUND ( 'NONE', #18744, .T. ) ;
#14289 = CARTESIAN_POINT ( 'NONE',  ( -61.42214656768812375, 31.00000000000000711, 79.86467493626638259 ) ) ;
#14290 = LINE ( 'NONE', #24355, #27479 ) ;
#14291 = CIRCLE ( 'NONE', #3090, 51.99999999999999289 ) ;
#14292 = ADVANCED_FACE ( 'NONE', ( #21244 ), #7883, .F. ) ;
#14293 = ORIENTED_EDGE ( 'NONE', *, *, #3912, .T. ) ;
#14294 = LINE ( 'NONE', #31085, #18027 ) ;
#14295 = ORIENTED_EDGE ( 'NONE', *, *, #30431, .T. ) ;
#14296 = CARTESIAN_POINT ( 'NONE',  ( 9.000000000000001776, 35.11945359308110426, 38.34871548466026070 ) ) ;
#14297 = DIRECTION ( 'NONE',  ( -3.996523416598930318E-16, 2.658563593772947863E-15, 1.000000000000000000 ) ) ;
#14298 = EDGE_CURVE ( 'NONE', #31074, #32443, #24934, .T. ) ;
#14299 = LINE ( 'NONE', #11034, #21472 ) ;
#14300 = CIRCLE ( 'NONE', #1026, 59.00000000000000000 ) ;
#14301 = CYLINDRICAL_SURFACE ( 'NONE', #5936, 51.99999999999999289 ) ;
#14302 = ORIENTED_EDGE ( 'NONE', *, *, #32005, .T. ) ;
#14303 = EDGE_CURVE ( 'NONE', #13702, #11934, #25603, .T. ) ;
#14304 = ORIENTED_EDGE ( 'NONE', *, *, #38202, .F. ) ;
#14305 = DIRECTION ( 'NONE',  ( 0.000000000000000000, 0.000000000000000000, 1.000000000000000000 ) ) ;
#14306 = VECTOR ( 'NONE', #1359, 1000.000000000000000 ) ;
#14307 = FACE_OUTER_BOUND ( 'NONE', #15263, .T. ) ;
#14308 = CARTESIAN_POINT ( 'NONE',  ( 109.0695705685734254, 106.4195705685780524, 7.000000000000249578 ) ) ;
#14309 = ORIENTED_EDGE ( 'NONE', *, *, #5706, .F. ) ;
#14311 = ORIENTED_EDGE ( 'NONE', *, *, #10418, .T. ) ;
#14310 = CARTESIAN_POINT ( 'NONE',  ( 0.000000000000000000, 0.000000000000000000, 0.000000000000000000 ) ) ;
#14312 = CARTESIAN_POINT ( 'NONE',  ( -32.45554871466278968, 31.00000000000000355, -28.56710966684966380 ) ) ;
#14313 = CIRCLE ( 'NONE', #38666, 47.49900000000000944 ) ;
#14314 = LINE ( 'NONE', #4456, #18910 ) ;
#14315 = CIRCLE ( 'NONE', #19903, 20.00000000000000355 ) ;
#14317 = ORIENTED_EDGE ( 'NONE', *, *, #22720, .F. ) ;
#14316 = CARTESIAN_POINT ( 'NONE',  ( 0.000000000000000000, -25.52601536738579213, -19.21447964122724272 ) ) ;
#14318 = AXIS2_PLACEMENT_3D ( 'NONE', #36919, #23661, #32791 ) ;
#14319 = VERTEX_POINT ( 'NONE', #38618 ) ;
#14320 = CARTESIAN_POINT ( 'NONE',  ( 49.67886955981430219, 40.00000000000000000, -43.43868092391004865 ) ) ;
#14321 = EDGE_CURVE ( 'NONE', #34774, #30296, #30471, .T. ) ;
#14322 = EDGE_CURVE ( 'NONE', #21257, #29613, #25365, .T. ) ;
#14323 = CARTESIAN_POINT ( 'NONE',  ( 17.99999999999999645, 0.000000000000000000, 0.000000000000000000 ) ) ;
#14324 = EDGE_CURVE ( 'NONE', #30077, #24613, #36693, .T. ) ;
#14325 = ADVANCED_FACE ( 'NONE', ( #5042 ), #22103, .F. ) ;
#14326 = EDGE_CURVE ( 'NONE', #40263, #1932, #16534, .T. ) ;
#14327 = PLANE ( 'NONE',  #32439 ) ;
#14328 = ORIENTED_EDGE ( 'NONE', *, *, #1659, .F. ) ;
#14329 = VERTEX_POINT ( 'NONE', #41695 ) ;
#14330 = AXIS2_PLACEMENT_3D ( 'NONE', #16212, #29508, #42776 ) ;
#14331 = CARTESIAN_POINT ( 'NONE',  ( 17.99999999999999645, -2.418575551220017328, -120.4767259403369053 ) ) ;
#14332 = DIRECTION ( 'NONE',  ( 0.000000000000000000, 0.000000000000000000, 1.000000000000000000 ) ) ;
#14333 = CARTESIAN_POINT ( 'NONE',  ( 23.58227068755204314, 31.00000000000000355, -47.84673847638903510 ) ) ;
#14334 = CYLINDRICAL_SURFACE ( 'NONE', #958, 47.49900000000000233 ) ;
#14335 = ORIENTED_EDGE ( 'NONE', *, *, #20207, .T. ) ;
#14336 = AXIS2_PLACEMENT_3D ( 'NONE', #23830, #1081, #34049 ) ;
#14337 = AXIS2_PLACEMENT_3D ( 'NONE', #14671, #11384, #8096 ) ;
#14338 = CIRCLE ( 'NONE', #5960, 20.00000000000000711 ) ;
#14339 = LINE ( 'NONE', #1428, #3068 ) ;
#14340 = ORIENTED_EDGE ( 'NONE', *, *, #23394, .F. ) ;
#14341 = CARTESIAN_POINT ( 'NONE',  ( 25.10416666396844576, 40.00000000000000000, 1.636246165087044124 ) ) ;
#14342 = MECHANICAL_DESIGN_GEOMETRIC_PRESENTATION_REPRESENTATION (  '', ( #9421 ), #19244 ) ;
#14343 = ORIENTED_EDGE ( 'NONE', *, *, #35908, .T. ) ;
#14345 = CIRCLE ( 'NONE', #17859, 58.99999999999999289 ) ;
#14344 = CARTESIAN_POINT ( 'NONE',  ( 17.99999999999999645, 34.03109950475885626, -115.5957406979046596 ) ) ;
#14346 = DIRECTION ( 'NONE',  ( 0.000000000000000000, 0.9980267284282712259, 0.06279051952931685721 ) ) ;
#14347 = CARTESIAN_POINT ( 'NONE',  ( 33.43413415811954081, 31.00000000000000355, -67.56680175473152872 ) ) ;
#14349 = CARTESIAN_POINT ( 'NONE',  ( 9.885896071376818028, 40.00000000000000000, -74.20985814143865866 ) ) ;
#14348 = CIRCLE ( 'NONE', #6649, 52.00000000000000000 ) ;
#14350 = DIRECTION ( 'NONE',  ( 0.000000000000000000, 0.000000000000000000, 1.000000000000000000 ) ) ;
#14351 = EDGE_CURVE ( 'NONE', #6315, #18244, #38206, .T. ) ;
#14352 = ORIENTED_EDGE ( 'NONE', *, *, #33507, .F. ) ;
#14353 = DIRECTION ( 'NONE',  ( 3.009274222672345096E-17, 1.000000000000000000, -2.455023325076455345E-18 ) ) ;
#14354 = ORIENTED_EDGE ( 'NONE', *, *, #12485, .F. ) ;
#14355 = DIRECTION ( 'NONE',  ( -1.000000000000000000, 0.000000000000000000, 0.000000000000000000 ) ) ;
#14356 = CARTESIAN_POINT ( 'NONE',  ( -4.211140560182196957, 2.431303136016537803, -3.745885042887433514 ) ) ;
#14358 = ORIENTED_EDGE ( 'NONE', *, *, #21761, .T. ) ;
#14357 = DIRECTION ( 'NONE',  ( -1.000000000000000000, -0.000000000000000000, 0.000000000000000000 ) ) ;
#14359 = CARTESIAN_POINT ( 'NONE',  ( 17.99999999999999645, 0.000000000000000000, 0.000000000000000000 ) ) ;
#14360 = EDGE_LOOP ( 'NONE', ( #8583, #42875, #8069, #24738 ) ) ;
#14361 = DIRECTION ( 'NONE',  ( -0.000000000000000000, -0.000000000000000000, 1.000000000000000000 ) ) ;
#14362 = CARTESIAN_POINT ( 'NONE',  ( -12.78314611188302052, 40.00000000000000000, 97.07982689498881257 ) ) ;
#14363 = CARTESIAN_POINT ( 'NONE',  ( 0.000000000000000000, 19.69434969228073484, 24.58291258574055860 ) ) ;
#14364 = ORIENTED_EDGE ( 'NONE', *, *, #9989, .T. ) ;
#14365 = FACE_OUTER_BOUND ( 'NONE', #29197, .T. ) ;
#14366 = CARTESIAN_POINT ( 'NONE',  ( 17.99999999999999645, -25.46650492921884279, -19.29328419707811193 ) ) ;
#14367 = CIRCLE ( 'NONE', #24862, 59.00000000000000000 ) ;
#14368 = AXIS2_PLACEMENT_3D ( 'NONE', #18533, #5397, #18761 ) ;
#14369 = AXIS2_PLACEMENT_3D ( 'NONE', #3649, #2786, #13096 ) ;
#14370 = VECTOR ( 'NONE', #3122, 1000.000000000000000 ) ;
#14371 = ORIENTED_EDGE ( 'NONE', *, *, #6241, .F. ) ;
#14372 = CYLINDRICAL_SURFACE ( 'NONE', #10737, 51.99999999999999289 ) ;
#14373 = VERTEX_POINT ( 'NONE', #21679 ) ;
#14374 = CARTESIAN_POINT ( 'NONE',  ( -20.28213647683248766, 40.00000000000000000, 23.06128528321566051 ) ) ;
#14375 = AXIS2_PLACEMENT_3D ( 'NONE', #21936, #4884, #1599 ) ;
#14376 = DIRECTION ( 'NONE',  ( 0.000000000000000000, 1.000000000000000000, -1.060184893785364939E-15 ) ) ;
#14377 = EDGE_CURVE ( 'NONE', #36486, #42699, #11835, .T. ) ;
#14378 = AXIS2_PLACEMENT_3D ( 'NONE', #28373, #5429, #1927 ) ;
#14379 = CARTESIAN_POINT ( 'NONE',  ( 1.798435537469519230E-14, -1.196353617197826191E-13, -44.99999999999999289 ) ) ;
#14380 = ADVANCED_FACE ( 'NONE', ( #6110 ), #15747, .T. ) ;
#14381 = EDGE_CURVE ( 'NONE', #16155, #25554, #26265, .T. ) ;
#14382 = CIRCLE ( 'NONE', #34565, 13.59999999999999787 ) ;
#14383 = CARTESIAN_POINT ( 'NONE',  ( 106.4195705685756792, -106.4195705685758213, 9.999999999999671374 ) ) ;
#14384 = ORIENTED_EDGE ( 'NONE', *, *, #27567, .F. ) ;
#14386 = DIRECTION ( 'NONE',  ( 0.000000000000000000, -0.6736956436465478815, -0.7390089172206675272 ) ) ;
#14385 = DIRECTION ( 'NONE',  ( -1.000000000000000000, -0.000000000000000000, -0.000000000000000000 ) ) ;
#14387 = ADVANCED_FACE ( 'NONE', ( #29051 ), #35987, .F. ) ;
#14389 = EDGE_LOOP ( 'NONE', ( #28326, #7818, #10347, #5693 ) ) ;
#14388 = CIRCLE ( 'NONE', #38736, 116.0000000000000000 ) ;
#14390 = DIRECTION ( 'NONE',  ( -1.000000000000000000, -0.000000000000000000, -0.000000000000000000 ) ) ;
#14391 = CARTESIAN_POINT ( 'NONE',  ( 25.04716826810500763, 31.00000000000000355, 3.293035637142270655 ) ) ;
#14392 = ORIENTED_EDGE ( 'NONE', *, *, #9014, .T. ) ;
#14393 = DIRECTION ( 'NONE',  ( 0.000000000000000000, -0.5528000653611833126, -0.8333139190825216147 ) ) ;
#14394 = CARTESIAN_POINT ( 'NONE',  ( 0.000000000000000000, 0.000000000000000000, 0.000000000000000000 ) ) ;
#14395 = ITEM_DEFINED_TRANSFORMATION ( 'NONE', 'NONE', #33731,  #13552 ) ;
#14396 = CARTESIAN_POINT ( 'NONE',  ( 0.000000000000000000, 0.000000000000000000, 0.000000000000000000 ) ) ;
#14397 = CARTESIAN_POINT ( 'NONE',  ( 66.75212336275305347, 31.00000000000000000, -51.21939497476837744 ) ) ;
#14398 = EDGE_CURVE ( 'NONE', #8366, #28381, #25584, .T. ) ;
#14400 = ORIENTED_EDGE ( 'NONE', *, *, #1170, .F. ) ;
#14399 = CIRCLE ( 'NONE', #24894, 20.00000000000000355 ) ;
#14401 = CARTESIAN_POINT ( 'NONE',  ( -41.92568936860566708, 31.00000000000000355, -5.596851440150872214 ) ) ;
#14402 = AXIS2_PLACEMENT_3D ( 'NONE', #817, #4306, #23786 ) ;
#14403 = CARTESIAN_POINT ( 'NONE',  ( -49.69442049507403425, 40.00000000000000000, -64.76435429890716478 ) ) ;
#14404 = CIRCLE ( 'NONE', #23475, 59.00000000000000000 ) ;
#14405 = AXIS2_PLACEMENT_3D ( 'NONE', #20425, #23481, #13873 ) ;
#14406 = FACE_BOUND ( 'NONE', #28309, .T. ) ;
#14407 = DIRECTION ( 'NONE',  ( 0.000000000000000000, 0.000000000000000000, 1.000000000000000000 ) ) ;
#14408 = CARTESIAN_POINT ( 'NONE',  ( 17.99999999999999645, 73.51007459736548810, -89.73443560133290475 ) ) ;
#14409 = CIRCLE ( 'NONE', #27682, 20.00000000000001066 ) ;
#14411 = ORIENTED_EDGE ( 'NONE', *, *, #3193, .F. ) ;
#14410 = CARTESIAN_POINT ( 'NONE',  ( 17.99999999999999645, -119.0898412705473532, -18.38751498043852806 ) ) ;
#14412 = CARTESIAN_POINT ( 'NONE',  ( 0.000000000000000000, 41.60679253225764285, 108.2814610871947423 ) ) ;
#14413 = EDGE_CURVE ( 'NONE', #7766, #26460, #29754, .T. ) ;
#14414 = LINE ( 'NONE', #37077, #23071 ) ;
#14415 = CIRCLE ( 'NONE', #1144, 20.00000000000000000 ) ;
#14416 = ORIENTED_EDGE ( 'NONE', *, *, #35271, .T. ) ;
#14417 = CARTESIAN_POINT ( 'NONE',  ( 34.44467569804516671, 40.00000000000000000, 44.88666365967159777 ) ) ;
#14418 = CYLINDRICAL_SURFACE ( 'NONE', #36885, 47.49900000000000233 ) ;
#14419 = DIRECTION ( 'NONE',  ( 1.000000000000000000, 0.000000000000000000, 0.000000000000000000 ) ) ;
#14420 = ORIENTED_EDGE ( 'NONE', *, *, #5313, .T. ) ;
#14421 = LINE ( 'NONE', #27731, #5705 ) ;
#14422 = DIRECTION ( 'NONE',  ( 0.000000000000000000, 0.000000000000000000, 1.000000000000000000 ) ) ;
#14423 = AXIS2_PLACEMENT_3D ( 'NONE', #16270, #26303, #41397 ) ;
#14424 = ORIENTED_EDGE ( 'NONE', *, *, #25334, .F. ) ;
#14425 = DIRECTION ( 'NONE',  ( 1.000000000000000000, 0.000000000000000000, 0.000000000000000000 ) ) ;
#14426 = VERTEX_POINT ( 'NONE', #42733 ) ;
#14427 = LINE ( 'NONE', #423, #26040 ) ;
#14428 = VERTEX_POINT ( 'NONE', #5888 ) ;
#14429 = FACE_OUTER_BOUND ( 'NONE', #3633, .T. ) ;
#14430 = DIRECTION ( 'NONE',  ( -1.000000000000000000, 0.000000000000000000, 0.000000000000000000 ) ) ;
#14431 = EDGE_CURVE ( 'NONE', #5278, #33305, #23753, .T. ) ;
#14432 = ORIENTED_EDGE ( 'NONE', *, *, #25232, .T. ) ;
#14433 = CIRCLE ( 'NONE', #31147, 20.00000000000000711 ) ;
#14434 = CARTESIAN_POINT ( 'NONE',  ( 17.99999999999999645, -45.89132998247981732, -102.3829004574634496 ) ) ;
#14435 = EDGE_CURVE ( 'NONE', #22146, #19271, #9560, .T. ) ;
#14436 = DIRECTION ( 'NONE',  ( 1.000000000000000000, 0.000000000000000000, 0.000000000000000000 ) ) ;
#14437 = ORIENTED_EDGE ( 'NONE', *, *, #14504, .T. ) ;
#14438 = AXIS2_PLACEMENT_3D ( 'NONE', #8372, #14519, #14952 ) ;
#14439 = DIRECTION ( 'NONE',  ( 1.000000000000000000, 0.000000000000000000, -0.000000000000000000 ) ) ;
#14440 = AXIS2_PLACEMENT_3D ( 'NONE', #39046, #22523, #19245 ) ;
#14442 = DIRECTION ( 'NONE',  ( 0.000000000000000000, -1.246648735278247733E-14, -1.000000000000000000 ) ) ;
#14441 = AXIS2_PLACEMENT_3D ( 'NONE', #19789, #33054, #22866 ) ;
#14443 = FACE_OUTER_BOUND ( 'NONE', #41889, .T. ) ;
#14444 = CIRCLE ( 'NONE', #12323, 59.00000000000000000 ) ;
#14445 = DIRECTION ( 'NONE',  ( -0.000000000000000000, -0.000000000000000000, -1.000000000000000000 ) ) ;
#14446 = B_SPLINE_CURVE_WITH_KNOTS ( 'NONE', 3,
 ( #8005, #31152, #34398, #1241, #4954, #15019 ),
 .UNSPECIFIED., .F., .F.,
 ( 4, 2, 4 ),
 ( -3.640115492407174633E-06, 0.0002066546034006553863, 0.0004169493222937179812 ),
 .UNSPECIFIED. ) ;
#14447 = VERTEX_POINT ( 'NONE', #19461 ) ;
#14448 = ADVANCED_FACE ( 'NONE', ( #39246 ), #32726, .T. ) ;
#14449 = DIRECTION ( 'NONE',  ( -0.6382733856524369642, 1.166608493463239706E-16, -0.7698097720656550402 ) ) ;
#14450 = AXIS2_PLACEMENT_3D ( 'NONE', #29892, #10219, #39224 ) ;
#14451 = DIRECTION ( 'NONE',  ( -1.000000000000000000, 0.000000000000000000, 0.000000000000000000 ) ) ;
#14452 = CARTESIAN_POINT ( 'NONE',  ( 27.23661496637203427, 31.00000000000000355, 23.88131275951389654 ) ) ;
#14453 = ORIENTED_EDGE ( 'NONE', *, *, #24802, .F. ) ;
#14455 = CARTESIAN_POINT ( 'NONE',  ( 0.000000000000000000, 108.8880088604282008, -39.99251838045848473 ) ) ;
#14454 = CYLINDRICAL_SURFACE ( 'NONE', #38617, 13.59999999999999964 ) ;
#14456 = AXIS2_PLACEMENT_3D ( 'NONE', #36940, #40206, #47 ) ;
#14457 = EDGE_CURVE ( 'NONE', #5006, #6315, #20752, .T. ) ;
#14458 = CARTESIAN_POINT ( 'NONE',  ( 0.000000000000000000, -42.41764978026593269, -20.20639853260334107 ) ) ;
#14459 = ORIENTED_EDGE ( 'NONE', *, *, #20500, .T. ) ;
#14460 = CYLINDRICAL_SURFACE ( 'NONE', #11568, 36.00000000000000000 ) ;
#14461 = CARTESIAN_POINT ( 'NONE',  ( -15.46676570949300000, 40.00000000000000000, 45.57083133015776610 ) ) ;
#14462 = CARTESIAN_POINT ( 'NONE',  ( -51.85848278221650531, 40.00000000000000000, -6.921372802089502230 ) ) ;
#14463 = CARTESIAN_POINT ( 'NONE',  ( -10.00000000000000000, 0.000000000000000000, 0.000000000000000000 ) ) ;
#14464 = DIRECTION ( 'NONE',  ( 0.000000000000000000, 0.000000000000000000, 1.000000000000000000 ) ) ;
#14465 = CIRCLE ( 'NONE', #42971, 120.5010000000000190 ) ;
#14466 = CARTESIAN_POINT ( 'NONE',  ( 8.999999999999998224, 19.47322409167269441, 30.27859877001407796 ) ) ;
#14467 = CARTESIAN_POINT ( 'NONE',  ( 18.00000000000000355, -20.99948489194393275, -42.60488980472802467 ) ) ;
#14468 = CIRCLE ( 'NONE', #30497, 120.5010000000000332 ) ;
#14469 = TOROIDAL_SURFACE ( 'NONE', #31188, 4.000000000000000000, 0.2500000000000000000 ) ;
#14470 = VERTEX_POINT ( 'NONE', #3013 ) ;
#14471 = CARTESIAN_POINT ( 'NONE',  ( 25.04716826810500763, 40.00000000000000000, 3.293035637142270655 ) ) ;
#14472 = ORIENTED_EDGE ( 'NONE', *, *, #24453, .F. ) ;
#14473 = DIRECTION ( 'NONE',  ( -1.000000000000000000, -0.000000000000000000, -0.000000000000000000 ) ) ;
#14474 = DIRECTION ( 'NONE',  ( 0.000000000000000000, 0.000000000000000000, 1.000000000000000000 ) ) ;
#14475 = AXIS2_PLACEMENT_3D ( 'NONE', #18301, #21793, #35041 ) ;
#14476 = AXIS2_PLACEMENT_3D ( 'NONE', #3089, #16034, #19527 ) ;
#14477 = ORIENTED_EDGE ( 'NONE', *, *, #16249, .F. ) ;
#14478 = AXIS2_PLACEMENT_3D ( 'NONE', #23490, #40446, #10581 ) ;
#14479 = CARTESIAN_POINT ( 'NONE',  ( 0.000000000000000000, 0.000000000000000000, -1.199999999999999956 ) ) ;
#14480 = DIRECTION ( 'NONE',  ( -1.000000000000000000, 0.000000000000000000, 0.000000000000000000 ) ) ;
#14481 = ORIENTED_EDGE ( 'NONE', *, *, #5095, .F. ) ;
#14482 = DIRECTION ( 'NONE',  ( -1.000000000000000000, -0.000000000000000000, -0.000000000000000000 ) ) ;
#14483 = AXIS2_PLACEMENT_3D ( 'NONE', #14672, #27533, #40808 ) ;
#14484 = ORIENTED_EDGE ( 'NONE', *, *, #1041, .T. ) ;
#14485 = VERTEX_POINT ( 'NONE', #16172 ) ;
#14486 = DIRECTION ( 'NONE',  ( 0.000000000000000000, 0.000000000000000000, 1.000000000000000000 ) ) ;
#14487 = CARTESIAN_POINT ( 'NONE',  ( -56.48168293059611500, 31.00000000000000711, 43.19841958068096233 ) ) ;
#14488 = EDGE_LOOP ( 'NONE', ( #8951, #12017, #40127, #33444 ) ) ;
#14489 = FACE_OUTER_BOUND ( 'NONE', #7839, .T. ) ;
#14490 = EDGE_CURVE ( 'NONE', #30129, #38244, #2554, .T. ) ;
#14491 = CARTESIAN_POINT ( 'NONE',  ( 103.7695705685763556, -106.4195705685744855, 10.00000000000000000 ) ) ;
#14492 = EDGE_CURVE ( 'NONE', #21903, #2287, #12354, .T. ) ;
#14493 = VERTEX_POINT ( 'NONE', #25787 ) ;
#14494 = LINE ( 'NONE', #28653, #21774 ) ;
#14495 = ORIENTED_EDGE ( 'NONE', *, *, #4487, .T. ) ;
#14496 = CARTESIAN_POINT ( 'NONE',  ( -45.36921519482122989, 40.00000000000000711, 78.33339762292068542 ) ) ;
#14497 = VECTOR ( 'NONE', #31035, 1000.000000000000000 ) ;
#14499 = CARTESIAN_POINT ( 'NONE',  ( 0.000000000000000000, 0.000000000000000000, 0.000000000000000000 ) ) ;
#14498 = DIRECTION ( 'NONE',  ( -1.000000000000000000, 0.000000000000000000, -0.000000000000000000 ) ) ;
#14500 = CYLINDRICAL_SURFACE ( 'NONE', #29005, 116.0000000000000000 ) ;
#14501 = DIRECTION ( 'NONE',  ( 0.000000000000000000, 0.000000000000000000, 1.000000000000000000 ) ) ;
#14502 = CIRCLE ( 'NONE', #1228, 59.00000000000002132 ) ;
#14503 = ORIENTED_EDGE ( 'NONE', *, *, #25789, .F. ) ;
#14504 = EDGE_CURVE ( 'NONE', #14228, #20215, #24205, .T. ) ;
#14505 = AXIS2_PLACEMENT_3D ( 'NONE', #9827, #36217, #32741 ) ;
#14506 = DIRECTION ( 'NONE',  ( -1.000000000000000000, -0.000000000000000000, 0.000000000000000000 ) ) ;
#14507 = LINE ( 'NONE', #18442, #21982 ) ;
#14508 = ADVANCED_FACE ( 'NONE', ( #15538 ), #28834, .F. ) ;
#14509 = CARTESIAN_POINT ( 'NONE',  ( 11.43299787627070607, 31.00000000000000355, 86.72764684403134083 ) ) ;
#14510 = DIRECTION ( 'NONE',  ( 1.000000000000000000, 0.000000000000000000, 0.000000000000000000 ) ) ;
#14512 = VERTEX_POINT ( 'NONE', #8966 ) ;
#14511 = VECTOR ( 'NONE', #15344, 1000.000000000000000 ) ;
#14513 = CARTESIAN_POINT ( 'NONE',  ( 12.70938237924789860, 40.00000000000000000, -21.97768283340562689 ) ) ;
#14514 = APPLICATION_CONTEXT ( 'automotive_design' ) ;
#14515 = EDGE_LOOP ( 'NONE', ( #1279, #4804, #39913, #24370 ) ) ;
#14516 = VECTOR ( 'NONE', #29398, 1000.000000000000000 ) ;
#14517 = ORIENTED_EDGE ( 'NONE', *, *, #6996, .T. ) ;
#14518 = CARTESIAN_POINT ( 'NONE',  ( -10.00000000000000000, 0.000000000000000000, 0.000000000000000000 ) ) ;
#14519 = DIRECTION ( 'NONE',  ( 3.009274222672345096E-17, 1.000000000000000000, -2.455023325076454960E-18 ) ) ;
#14520 = DIRECTION ( 'NONE',  ( -1.000000000000000000, -0.000000000000000000, -0.000000000000000000 ) ) ;
#14521 = CARTESIAN_POINT ( 'NONE',  ( 0.2142857142857142738, -10.49781318335647917, -1.199999999999999956 ) ) ;
#14522 = ORIENTED_EDGE ( 'NONE', *, *, #34277, .F. ) ;
#14523 = DIRECTION ( 'NONE',  ( -1.000000000000000000, 0.000000000000000000, -0.000000000000000000 ) ) ;
#14524 = ORIENTED_EDGE ( 'NONE', *, *, #12459, .T. ) ;
#14525 = DIRECTION ( 'NONE',  ( 0.000000000000000000, 0.000000000000000000, 1.000000000000000000 ) ) ;
#14526 = EDGE_CURVE ( 'NONE', #31565, #20200, #8160, .T. ) ;
#14527 = DIRECTION ( 'NONE',  ( 0.000000000000000000, 0.000000000000000000, -1.000000000000000000 ) ) ;
#14528 = ADVANCED_FACE ( 'NONE', ( #32298 ), #29262, .F. ) ;
#14529 = AXIS2_PLACEMENT_3D ( 'NONE', #8118, #21487, #4846 ) ;
#14530 = DIRECTION ( 'NONE',  ( -1.000000000000000000, -0.000000000000000000, -0.000000000000000000 ) ) ;
#14531 = CARTESIAN_POINT ( 'NONE',  ( -10.00000000000000000, 0.000000000000000000, 0.000000000000000000 ) ) ;
#14532 = ORIENTED_EDGE ( 'NONE', *, *, #16170, .T. ) ;
#14533 = ORIENTED_EDGE ( 'NONE', *, *, #20323, .F. ) ;
#14534 = CARTESIAN_POINT ( 'NONE',  ( 17.99999999999999645, 0.000000000000000000, 0.000000000000000000 ) ) ;
#14535 = AXIS2_PLACEMENT_3D ( 'NONE', #12208, #25531, #41412 ) ;
#14536 = LINE ( 'NONE', #955, #41600 ) ;
#14537 = CIRCLE ( 'NONE', #4765, 51.99999999999999289 ) ;
#14538 = AXIS2_PLACEMENT_3D ( 'NONE', #36024, #32131, #12082 ) ;
#14539 = CIRCLE ( 'NONE', #27076, 116.0000000000000000 ) ;
#14540 = ORIENTED_EDGE ( 'NONE', *, *, #16623, .T. ) ;
#14542 = ORIENTED_EDGE ( 'NONE', *, *, #28224, .F. ) ;
#14541 = CARTESIAN_POINT ( 'NONE',  ( 0.000000000000000000, 150.5000000000000284, 6.999999999999998224 ) ) ;
#14543 = CARTESIAN_POINT ( 'NONE',  ( -2.659806967433831382, 31.00000000000000355, 39.59793253467758944 ) ) ;
#14544 = CARTESIAN_POINT ( 'NONE',  ( 0.000000000000000000, -82.63181128086789329, 81.41243003646944487 ) ) ;
#14545 = AXIS2_PLACEMENT_3D ( 'NONE', #5488, #39480, #35573 ) ;
#14546 = EDGE_CURVE ( 'NONE', #21330, #28092, #32516, .T. ) ;
#14548 = FILL_AREA_STYLE ('',( #25242 ) ) ;
#14547 = CARTESIAN_POINT ( 'NONE',  ( -4.000000000000000000, 0.1981133338132459731, 2.096406544454392723E-17 ) ) ;
#14549 = VERTEX_POINT ( 'NONE', #13926 ) ;
#14550 = CARTESIAN_POINT ( 'NONE',  ( 67.09393615765254992, 39.99999999999999289, 4.495243625008655819 ) ) ;
#14551 = PLANE ( 'NONE',  #2537 ) ;
#14552 = CARTESIAN_POINT ( 'NONE',  ( 6.896599878636567205, -12.98179148322719101, -1.199999999999999956 ) ) ;
#14553 = EDGE_CURVE ( 'NONE', #22175, #10037, #40705, .T. ) ;
#14554 = ORIENTED_EDGE ( 'NONE', *, *, #33381, .F. ) ;
#14555 = DIRECTION ( 'NONE',  ( 1.000000000000000000, 0.000000000000000000, 0.000000000000000000 ) ) ;
#14556 = VERTEX_POINT ( 'NONE', #7344 ) ;
#14557 = EDGE_CURVE ( 'NONE', #9213, #42604, #4059, .T. ) ;
#14558 = DIRECTION ( 'NONE',  ( 0.000000000000000000, 0.9048270524660205760, -0.4257792915650704391 ) ) ;
#14559 = DIRECTION ( 'NONE',  ( 1.000000000000000000, 0.000000000000000000, 0.000000000000000000 ) ) ;
#14560 = ADVANCED_FACE ( 'NONE', ( #41356 ), #34388, .F. ) ;
#14561 = CARTESIAN_POINT ( 'NONE',  ( 44.56294422764113250, 31.00000000000000355, 34.17917587534974189 ) ) ;
#14562 = AXIS2_PLACEMENT_3D ( 'NONE', #24032, #31212, #24687 ) ;
#14563 = CARTESIAN_POINT ( 'NONE',  ( 8.999999999999998224, 59.47573314508868236, -99.59235496188547643 ) ) ;
#14564 = CIRCLE ( 'NONE', #42391, 120.5010000000000332 ) ;
#14565 = ORIENTED_EDGE ( 'NONE', *, *, #33118, .F. ) ;
#14566 = EDGE_CURVE ( 'NONE', #10279, #10758, #33970, .T. ) ;
#14567 = AXIS2_PLACEMENT_3D ( 'NONE', #18899, #39309, #12533 ) ;
#14568 = CARTESIAN_POINT ( 'NONE',  ( 8.999999999999998224, 82.63181128086732485, 81.41243003647002752 ) ) ;
#14569 = VERTEX_POINT ( 'NONE', #21585 ) ;
#14570 = CARTESIAN_POINT ( 'NONE',  ( -29.59829689555773058, 40.00000000000000000, 3.906358533625565954 ) ) ;
#14571 = ORIENTED_EDGE ( 'NONE', *, *, #10667, .F. ) ;
#14572 = DIRECTION ( 'NONE',  ( 1.000000000000000000, 0.000000000000000000, 0.000000000000000000 ) ) ;
#14573 = CARTESIAN_POINT ( 'NONE',  ( 0.000000000000000000, 0.000000000000000000, 15.00000000000000000 ) ) ;
#14574 = CARTESIAN_POINT ( 'NONE',  ( -29.11455967534192979, 31.00000000000000355, 85.38284731564058916 ) ) ;
#14575 = CARTESIAN_POINT ( 'NONE',  ( -72.38966680857410552, 40.00000000000000711, 55.38960906678870799 ) ) ;
#14576 = DIRECTION ( 'NONE',  ( 0.000000000000000000, 0.000000000000000000, 1.000000000000000000 ) ) ;
#14577 = ORIENTED_EDGE ( 'NONE', *, *, #28483, .T. ) ;
#14578 = LINE ( 'NONE', #27882, #3262 ) ;
#14579 = EDGE_LOOP ( 'NONE', ( #30452, #28341, #40053, #36922 ) ) ;
#14580 = DIRECTION ( 'NONE',  ( 0.000000000000000000, 0.000000000000000000, 1.000000000000000000 ) ) ;
#14581 = DIRECTION ( 'NONE',  ( -1.000000000000000000, 0.000000000000000000, 0.000000000000000000 ) ) ;
#14582 = EDGE_CURVE ( 'NONE', #29681, #39320, #27664, .T. ) ;
#14583 = EDGE_CURVE ( 'NONE', #40375, #18884, #22868, .T. ) ;
#14585 = ORIENTED_EDGE ( 'NONE', *, *, #32103, .T. ) ;
#14584 = DIRECTION ( 'NONE',  ( -1.000000000000000000, 0.000000000000000000, -0.000000000000000000 ) ) ;
#14586 = DIRECTION ( 'NONE',  ( 0.000000000000000000, 0.3641605752528167539, 0.9313361774523405412 ) ) ;
#14587 = VERTEX_POINT ( 'NONE', #7782 ) ;
#14588 = CYLINDRICAL_SURFACE ( 'NONE', #39081, 59.00000000000000000 ) ;
#14589 = CARTESIAN_POINT ( 'NONE',  ( -89.22528799552154055, 40.00000000000000711, 43.99828826784794700 ) ) ;
#14590 = CARTESIAN_POINT ( 'NONE',  ( -1.655952806101422814, 3.662737355149034979, -7.623296525288699970E-18 ) ) ;
#14591 = ORIENTED_EDGE ( 'NONE', *, *, #6860, .F. ) ;
#14592 = CARTESIAN_POINT ( 'NONE',  ( 53.80287614962789178, -34.05525454449571754, 69.29271901957253021 ) ) ;
#14593 = AXIS2_PLACEMENT_3D ( 'NONE', #30881, #20892, #33704 ) ;
#14594 = DIRECTION ( 'NONE',  ( 1.000000000000000000, 0.000000000000000000, 0.000000000000000000 ) ) ;
#14595 = AXIS2_PLACEMENT_3D ( 'NONE', #40294, #23763, #20717 ) ;
#14596 = CIRCLE ( 'NONE', #41017, 20.00000000000000711 ) ;
#14598 = CARTESIAN_POINT ( 'NONE',  ( -1.600000000000000089, -12.75000000000000000, -1.199999999999999956 ) ) ;
#14597 = DIRECTION ( 'NONE',  ( 0.000000000000000000, 0.000000000000000000, 1.000000000000000000 ) ) ;
#14599 = ORIENTED_EDGE ( 'NONE', *, *, #20848, .T. ) ;
#14600 = EDGE_CURVE ( 'NONE', #9115, #3440, #2589, .T. ) ;
#14601 = CARTESIAN_POINT ( 'NONE',  ( -106.4195705685756081, 106.4195705685752529, 10.00000000000000000 ) ) ;
#14602 = ORIENTED_EDGE ( 'NONE', *, *, #21778, .T. ) ;
#14603 = DIRECTION ( 'NONE',  ( 1.000000000000000000, 0.000000000000000000, 0.000000000000000000 ) ) ;
#14604 = CARTESIAN_POINT ( 'NONE',  ( 36.56095242094649933, 40.00000000000000000, -4.755136101395176951 ) ) ;
#14605 = DIRECTION ( 'NONE',  ( 0.000000000000000000, 0.000000000000000000, -1.000000000000000000 ) ) ;
#14606 = DIRECTION ( 'NONE',  ( -1.000000000000000000, 0.000000000000000000, 0.000000000000000000 ) ) ;
#14607 = DIRECTION ( 'NONE',  ( 1.000000000000000000, 0.000000000000000000, 0.000000000000000000 ) ) ;
#14608 = VERTEX_POINT ( 'NONE', #10856 ) ;
#14610 = DIRECTION ( 'NONE',  ( -1.000000000000000000, 0.000000000000000000, 0.000000000000000000 ) ) ;
#14609 = LINE ( 'NONE', #4090, #39767 ) ;
#14611 = EDGE_LOOP ( 'NONE', ( #6123, #15741, #32488, #38603 ) ) ;
#14612 = EDGE_CURVE ( 'NONE', #16671, #6774, #18682, .T. ) ;
#14613 = CYLINDRICAL_SURFACE ( 'NONE', #40562, 59.00000000000001421 ) ;
#14614 = DIRECTION ( 'NONE',  ( -1.000000000000000000, 0.000000000000000000, 0.000000000000000000 ) ) ;
#14615 = ADVANCED_FACE ( 'NONE', ( #30711 ), #31142, .T. ) ;
#14616 = CARTESIAN_POINT ( 'NONE',  ( -15.87544005811639458, 31.00000000000000355, -27.47754625559162989 ) ) ;
#14617 = VERTEX_POINT ( 'NONE', #7994 ) ;
#14618 = DIRECTION ( 'NONE',  ( 0.000000000000000000, 0.000000000000000000, 1.000000000000000000 ) ) ;
#14619 = DIRECTION ( 'NONE',  ( 1.000000000000000000, 0.000000000000000000, 0.000000000000000000 ) ) ;
#14620 = CARTESIAN_POINT ( 'NONE',  ( 0.000000000000000000, 61.59243992711459015, 93.77976230226062171 ) ) ;
#14621 = CARTESIAN_POINT ( 'NONE',  ( -40.93297376624923345, 31.00000000000000355, -70.86912620794510076 ) ) ;
#14622 = VECTOR ( 'NONE', #26914, 999.9999999999997726 ) ;
#14623 = ORIENTED_EDGE ( 'NONE', *, *, #11590, .T. ) ;
#14624 = VECTOR ( 'NONE', #33495, 1000.000000000000000 ) ;
#14625 = CARTESIAN_POINT ( 'NONE',  ( -26.81486728382429519, 31.00000000000000355, -46.61672233255472975 ) ) ;
#14626 = CARTESIAN_POINT ( 'NONE',  ( -78.83182461418512332, 40.00000000000000711, -45.51551753872077910 ) ) ;
#14627 = VECTOR ( 'NONE', #42537, 1000.000000000000000 ) ;
#14628 = CARTESIAN_POINT ( 'NONE',  ( 2.500000000000000000, 2.357898499370431722, -2.818925648462311528E-15 ) ) ;
#14629 = EDGE_CURVE ( 'NONE', #14052, #18492, #27016, .T. ) ;
#14630 = CARTESIAN_POINT ( 'NONE',  ( 0.000000000000000000, 0.000000000000000000, 0.000000000000000000 ) ) ;
#14631 = CYLINDRICAL_SURFACE ( 'NONE', #15689, 31.49899999999999878 ) ;
#14632 = ADVANCED_FACE ( 'NONE', ( #4493 ), #14143, .T. ) ;
#14633 = EDGE_CURVE ( 'NONE', #7972, #11152, #14578, .T. ) ;
#14634 = EDGE_CURVE ( 'NONE', #17487, #41070, #6775, .T. ) ;
#14636 = ORIENTED_EDGE ( 'NONE', *, *, #32697, .T. ) ;
#14635 = DIRECTION ( 'NONE',  ( -1.000000000000000000, 0.000000000000000000, -0.000000000000000000 ) ) ;
#14637 = DIRECTION ( 'NONE',  ( 0.000000000000000000, 0.3612416661871471479, 0.9324722294043581439 ) ) ;
#14638 = CARTESIAN_POINT ( 'NONE',  ( 0.000000000000000000, -109.4038418350907023, 50.51029986767514401 ) ) ;
#14639 = VERTEX_POINT ( 'NONE', #27434 ) ;
#14640 = CARTESIAN_POINT ( 'NONE',  ( -57.43240763726046794, 40.00000000000000000, -19.49446143887317717 ) ) ;
#14641 = CARTESIAN_POINT ( 'NONE',  ( 8.999999999999998224, 0.000000000000000000, 14.91999999999999993 ) ) ;
#14642 = CARTESIAN_POINT ( 'NONE',  ( 17.99999999999999645, 117.9424311864592312, -24.69967462998914698 ) ) ;
#14643 = ORIENTED_EDGE ( 'NONE', *, *, #36594, .F. ) ;
#14644 = CARTESIAN_POINT ( 'NONE',  ( 9.000000000000000000, -31.94619804602776725, 16.59639811537345366 ) ) ;
#14645 = CARTESIAN_POINT ( 'NONE',  ( 0.000000000000000000, 7.162210897275730126, 51.50439529848829778 ) ) ;
#14646 = ORIENTED_EDGE ( 'NONE', *, *, #6662, .T. ) ;
#14647 = CARTESIAN_POINT ( 'NONE',  ( 17.99999999999999645, -112.1427988504408120, 3.502162136923045566 ) ) ;
#14648 = EDGE_LOOP ( 'NONE', ( #27209, #14295, #12606, #42492 ) ) ;
#14649 = DIRECTION ( 'NONE',  ( 1.000000000000000000, 0.000000000000000000, -0.000000000000000000 ) ) ;
#14651 = VERTEX_POINT ( 'NONE', #37453 ) ;
#14650 = VECTOR ( 'NONE', #36128, 1000.000000000000000 ) ;
#14652 = DIRECTION ( 'NONE',  ( 0.000000000000000000, 0.8183027759081702435, -0.5747874102144051589 ) ) ;
#14653 = AXIS2_PLACEMENT_3D ( 'NONE', #23061, #8860, #19142 ) ;
#14654 = CARTESIAN_POINT ( 'NONE',  ( -76.05825820879897492, 31.00000000000000711, 66.55365856249082412 ) ) ;
#14655 = ORIENTED_EDGE ( 'NONE', *, *, #4756, .T. ) ;
#14656 = CIRCLE ( 'NONE', #20237, 59.00000000000000711 ) ;
#14657 = DIRECTION ( 'NONE',  ( 0.000000000000000000, 0.000000000000000000, 1.000000000000000000 ) ) ;
#14658 = DIRECTION ( 'NONE',  ( -1.000000000000000000, 0.000000000000000000, -0.000000000000000000 ) ) ;
#14659 = EDGE_LOOP ( 'NONE', ( #3412, #34790, #21364, #26270 ) ) ;
#14660 = FACE_OUTER_BOUND ( 'NONE', #14132, .T. ) ;
#14661 = CARTESIAN_POINT ( 'NONE',  ( 18.00000000000000355, -32.00046193115124282, -34.40241257139720688 ) ) ;
#14662 = ORIENTED_EDGE ( 'NONE', *, *, #24719, .T. ) ;
#14663 = CARTESIAN_POINT ( 'NONE',  ( 17.99999999999999645, -93.26762629039376407, -76.29967815892449323 ) ) ;
#14664 = DIRECTION ( 'NONE',  ( -1.000000000000000000, 0.000000000000000000, 0.000000000000000000 ) ) ;
#14665 = ORIENTED_EDGE ( 'NONE', *, *, #3431, .T. ) ;
#14666 = DIRECTION ( 'NONE',  ( -2.137915722948479303E-31, 1.000000000000000000, -6.123233995736766036E-17 ) ) ;
#14667 = CYLINDRICAL_SURFACE ( 'NONE', #18399, 120.5010000000000190 ) ;
#14668 = CARTESIAN_POINT ( 'NONE',  ( 35.44578089419255917, 31.00000000000000355, -40.42088417236866604 ) ) ;
#14669 = EDGE_LOOP ( 'NONE', ( #18523, #13015, #1173, #30310 ) ) ;
#14671 = CARTESIAN_POINT ( 'NONE',  ( 0.000000000000000000, -51.27532863109303918, -99.79535634195178773 ) ) ;
#14670 = DIRECTION ( 'NONE',  ( -1.000000000000000000, -0.000000000000000000, -0.000000000000000000 ) ) ;
#14672 = CARTESIAN_POINT ( 'NONE',  ( 18.00000000000000355, -36.34385289850609979, 29.77717097092063270 ) ) ;
#14673 = VERTEX_POINT ( 'NONE', #17214 ) ;
#14674 = CYLINDRICAL_SURFACE ( 'NONE', #19928, 120.5010000000000190 ) ;
#14675 = CARTESIAN_POINT ( 'NONE',  ( -48.80550277073417931, 40.00000000000000000, -13.06547612810710035 ) ) ;
#14676 = CARTESIAN_POINT ( 'NONE',  ( -7.015336270754768400, 40.00000000000000000, -53.95087245962636047 ) ) ;
#14677 = CIRCLE ( 'NONE', #40415, 120.5010000000000190 ) ;
#14678 = AXIS2_PLACEMENT_3D ( 'NONE', #4023, #30676, #13892 ) ;
#14679 = DIRECTION ( 'NONE',  ( 0.000000000000000000, 0.000000000000000000, -1.000000000000000000 ) ) ;
#14680 = DIRECTION ( 'NONE',  ( 0.000000000000000000, 0.9968120070307504577, -0.07978610555307970309 ) ) ;
#14681 = ADVANCED_FACE ( 'NONE', ( #30501 ), #18093, .T. ) ;
#14682 = EDGE_CURVE ( 'NONE', #14651, #1613, #17295, .T. ) ;
#14683 = AXIS2_PLACEMENT_3D ( 'NONE', #27724, #21852, #18578 ) ;
#14684 = DIRECTION ( 'NONE',  ( 1.000000000000000000, 0.000000000000000000, 0.000000000000000000 ) ) ;
#14685 = DIRECTION ( 'NONE',  ( 0.000000000000000000, 0.000000000000000000, 1.000000000000000000 ) ) ;
#14686 = EDGE_CURVE ( 'NONE', #21082, #8807, #9593, .T. ) ;
#14687 = ORIENTED_EDGE ( 'NONE', *, *, #9055, .F. ) ;
#14688 = CARTESIAN_POINT ( 'NONE',  ( -15.87544005811639458, 40.00000000000000000, -27.47754625559162989 ) ) ;
#14689 = ORIENTED_EDGE ( 'NONE', *, *, #17846, .T. ) ;
#14690 = DIRECTION ( 'NONE',  ( -1.000000000000000000, -0.000000000000000000, -0.000000000000000000 ) ) ;
#14691 = DIRECTION ( 'NONE',  ( 0.000000000000000000, 0.8183027759081701324, -0.5747874102144052699 ) ) ;
#14692 = VERTEX_POINT ( 'NONE', #12153 ) ;
#14693 = FACE_OUTER_BOUND ( 'NONE', #13988, .T. ) ;
#14694 = CARTESIAN_POINT ( 'NONE',  ( 18.00000000000000355, 32.32520163883584274, 34.09746168776050013 ) ) ;
#14695 = EDGE_LOOP ( 'NONE', ( #27651, #26561, #39131, #23138 ) ) ;
#14696 = DIRECTION ( 'NONE',  ( -1.000000000000000000, 0.000000000000000000, 0.000000000000000000 ) ) ;
#14697 = ORIENTED_EDGE ( 'NONE', *, *, #32192, .F. ) ;
#14698 = ADVANCED_FACE ( 'NONE', ( #38311 ), #29168, .F. ) ;
#14699 = VERTEX_POINT ( 'NONE', #21994 ) ;
#14700 = DIRECTION ( 'NONE',  ( 0.000000000000000000, 0.000000000000000000, 1.000000000000000000 ) ) ;
#14701 = EDGE_CURVE ( 'NONE', #41125, #8821, #41633, .T. ) ;
#14703 = AXIS2_PLACEMENT_3D ( 'NONE', #32714, #16157, #27057 ) ;
#14702 = CARTESIAN_POINT ( 'NONE',  ( -44.72205690102930475, 31.00000000000000355, -58.47036224961646411 ) ) ;
#14704 = ORIENTED_EDGE ( 'NONE', *, *, #28137, .T. ) ;
#14705 = DIRECTION ( 'NONE',  ( -1.000000000000000000, -0.000000000000000000, -0.000000000000000000 ) ) ;
#14706 = CIRCLE ( 'NONE', #8416, 19.19999999999999574 ) ;
#14707 = CARTESIAN_POINT ( 'NONE',  ( 0.000000000000000000, 29.36437154451999376, 116.8684075565137164 ) ) ;
#14708 = ORIENTED_EDGE ( 'NONE', *, *, #25467, .T. ) ;
#14709 = CARTESIAN_POINT ( 'NONE',  ( 22.90854556226710415, -12.05525454449572464, -74.83297477053821467 ) ) ;
#14710 = ORIENTED_EDGE ( 'NONE', *, *, #30088, .T. ) ;
#14711 = CARTESIAN_POINT ( 'NONE',  ( -40.08783408682389648, 40.00000000000000000, 81.04563091341927361 ) ) ;
#14712 = AXIS2_PLACEMENT_3D ( 'NONE', #9085, #39173, #22440 ) ;
#14713 = CIRCLE ( 'NONE', #15436, 4.000000000000000000 ) ;
#14714 = CARTESIAN_POINT ( 'NONE',  ( 27.10182830755124428, 31.00000000000000355, 1.799748011963437033 ) ) ;
#14715 = CIRCLE ( 'NONE', #2809, 58.99999999999999289 ) ;
#14717 = CYLINDRICAL_SURFACE ( 'NONE', #26993, 58.99999999999998579 ) ;
#14716 = CARTESIAN_POINT ( 'NONE',  ( 17.99999999999999645, 6.854627147200274884, -115.7972974066012881 ) ) ;
#14718 = AXIS2_PLACEMENT_3D ( 'NONE', #20714, #28545, #21802 ) ;
#14719 = CARTESIAN_POINT ( 'NONE',  ( -23.34979319748359927, -2.055254544495722868, 2.972870684497277427 ) ) ;
#14720 = ADVANCED_FACE ( 'NONE', ( #22421 ), #8431, .F. ) ;
#14721 = DIRECTION ( 'NONE',  ( -1.000000000000000000, 0.000000000000000000, 0.000000000000000000 ) ) ;
#14722 = ORIENTED_EDGE ( 'NONE', *, *, #18791, .F. ) ;
#14723 =( NAMED_UNIT ( * ) SI_UNIT ( $, .STERADIAN. ) SOLID_ANGLE_UNIT ( ) );
#14724 = EDGE_LOOP ( 'NONE', ( #22380, #3808, #37230, #36550 ) ) ;
#14725 = DIRECTION ( 'NONE',  ( 0.000000000000000000, 0.000000000000000000, 1.000000000000000000 ) ) ;
#14726 = CARTESIAN_POINT ( 'NONE',  ( 12.74197863150380883, 31.00000000000000355, 96.66318596537892915 ) ) ;
#14727 = CARTESIAN_POINT ( 'NONE',  ( 106.4195705685741302, 106.4195705685767166, 9.999999999999998224 ) ) ;
#14728 = VERTEX_POINT ( 'NONE', #1656 ) ;
#14729 = CARTESIAN_POINT ( 'NONE',  ( 20.65150112226537260, 40.00000000000000000, -15.81946110361252877 ) ) ;
#14730 = ORIENTED_EDGE ( 'NONE', *, *, #14002, .F. ) ;
#14731 = ORIENTED_EDGE ( 'NONE', *, *, #29228, .F. ) ;
#14732 = CARTESIAN_POINT ( 'NONE',  ( 0.000000000000000000, 0.000000000000000000, 130.0000000000000000 ) ) ;
#14733 = DIRECTION ( 'NONE',  ( 0.000000000000000000, 0.000000000000000000, 1.000000000000000000 ) ) ;
#14734 = CYLINDRICAL_SURFACE ( 'NONE', #12978, 47.49900000000000233 ) ;
#14735 = EDGE_CURVE ( 'NONE', #39353, #32376, #32566, .T. ) ;
#14736 = DIRECTION ( 'NONE',  ( 0.000000000000000000, 0.000000000000000000, 1.000000000000000000 ) ) ;
#14737 = VECTOR ( 'NONE', #2688, 1000.000000000000000 ) ;
#14738 = ORIENTED_EDGE ( 'NONE', *, *, #42848, .T. ) ;
#14739 = LINE ( 'NONE', #11238, #24270 ) ;
#14740 = VERTEX_POINT ( 'NONE', #38738 ) ;
#14741 = DIRECTION ( 'NONE',  ( 1.000000000000000000, 0.000000000000000000, 0.000000000000000000 ) ) ;
#14742 = AXIS2_PLACEMENT_3D ( 'NONE', #23929, #30039, #37197 ) ;
#14743 = CARTESIAN_POINT ( 'NONE',  ( 0.000000000000000000, -100.6739960869721102, 49.52796165323228195 ) ) ;
#14744 = CIRCLE ( 'NONE', #19633, 15.99999999999998579 ) ;
#14745 = EDGE_CURVE ( 'NONE', #17370, #28827, #29787, .T. ) ;
#14746 = DIRECTION ( 'NONE',  ( 0.000000000000000000, -0.9213119778704165208, 0.3888241754733123834 ) ) ;
#14747 = AXIS2_PLACEMENT_3D ( 'NONE', #15453, #42010, #38745 ) ;
#14748 = CARTESIAN_POINT ( 'NONE',  ( 17.99999999999999645, 88.56657216608614647, 68.87840567545953263 ) ) ;
#14749 = VERTEX_POINT ( 'NONE', #12373 ) ;
#14750 = ORIENTED_EDGE ( 'NONE', *, *, #25812, .F. ) ;
#14751 = FACE_OUTER_BOUND ( 'NONE', #4477, .T. ) ;
#14752 = FACE_OUTER_BOUND ( 'NONE', #29544, .T. ) ;
#14753 = ADVANCED_FACE ( 'NONE', ( #34830 ), #8863, .F. ) ;
#14754 = CIRCLE ( 'NONE', #39088, 116.0000000000000000 ) ;
#14755 = VERTEX_POINT ( 'NONE', #41584 ) ;
#14757 = VERTEX_POINT ( 'NONE', #2499 ) ;
#14756 = CARTESIAN_POINT ( 'NONE',  ( 0.000000000000000000, -46.90537658765333617, 2.727856614654147638 ) ) ;
#14758 = EDGE_CURVE ( 'NONE', #11646, #17236, #8197, .T. ) ;
#14759 = CARTESIAN_POINT ( 'NONE',  ( -41.03896728213481992, 31.00000000000000355, -11.06873348903806864 ) ) ;
#14760 = DIRECTION ( 'NONE',  ( 0.000000000000000000, 0.000000000000000000, 1.000000000000000000 ) ) ;
#14762 = DIRECTION ( 'NONE',  ( 1.000000000000000000, 0.000000000000000000, 0.000000000000000000 ) ) ;
#14761 = DIRECTION ( 'NONE',  ( 1.000000000000000000, 0.000000000000000000, 0.000000000000000000 ) ) ;
#14763 = VERTEX_POINT ( 'NONE', #35673 ) ;
#14764 = LINE ( 'NONE', #13952, #13731 ) ;
#14765 = CARTESIAN_POINT ( 'NONE',  ( -53.12901929299007975, 40.00000000000000000, 30.56653509229933263 ) ) ;
#14766 = CARTESIAN_POINT ( 'NONE',  ( 17.99999999999999645, -107.5680526044921947, 31.89649718262059608 ) ) ;
#14767 = DIRECTION ( 'NONE',  ( 1.000000000000000000, 0.000000000000000000, 0.000000000000000000 ) ) ;
#14768 = ORIENTED_EDGE ( 'NONE', *, *, #32837, .T. ) ;
#14769 = LINE ( 'NONE', #18281, #16129 ) ;
#14770 = EDGE_CURVE ( 'NONE', #23787, #3192, #12387, .T. ) ;
#14771 = ORIENTED_EDGE ( 'NONE', *, *, #4982, .F. ) ;
#14772 = PRESENTATION_STYLE_ASSIGNMENT (( #1421 ) ) ;
#14774 = EDGE_CURVE ( 'NONE', #27564, #25474, #14991, .T. ) ;
#14773 = AXIS2_PLACEMENT_3D ( 'NONE', #5917, #9637, #29288 ) ;
#14775 = CARTESIAN_POINT ( 'NONE',  ( 1.600000000000000089, -12.75000000000000000, -1.199999999999999956 ) ) ;
#14776 = CARTESIAN_POINT ( 'NONE',  ( 18.00000000000000355, -47.22458491092822896, 5.098390039074067737 ) ) ;
#14777 = CIRCLE ( 'NONE', #97, 2.041999999999999815 ) ;
#14779 = ADVANCED_FACE ( 'NONE', ( #31564 ), #32413, .F. ) ;
#14778 = CARTESIAN_POINT ( 'NONE',  ( -19.97695672607123640, 31.00000000000000355, -58.81104016858105155 ) ) ;
#14780 = DIRECTION ( 'NONE',  ( 1.000000000000000000, -0.000000000000000000, 0.000000000000000000 ) ) ;
#14781 = ORIENTED_EDGE ( 'NONE', *, *, #22481, .F. ) ;
#14782 = CARTESIAN_POINT ( 'NONE',  ( 17.99999999999999645, -18.42432724429495750, 30.92804820215996742 ) ) ;
#14783 = CIRCLE ( 'NONE', #16171, 59.00000000000001421 ) ;
#14784 = ORIENTED_EDGE ( 'NONE', *, *, #26874, .F. ) ;
#14785 = DIRECTION ( 'NONE',  ( -1.000000000000000000, -0.000000000000000000, 0.000000000000000000 ) ) ;
#14786 = CARTESIAN_POINT ( 'NONE',  ( 5.991980000000000750, 0.000000000000000000, 15.00000000000000178 ) ) ;
#14787 = CARTESIAN_POINT ( 'NONE',  ( 78.79907178683629354, 31.00000000000000000, 38.97904116289377185 ) ) ;
#14788 = CARTESIAN_POINT ( 'NONE',  ( -91.21105805184879500, 40.00000000000000711, 11.89862498596346718 ) ) ;
#14789 = DIRECTION ( 'NONE',  ( 1.000000000000000000, 0.000000000000000000, 0.000000000000000000 ) ) ;
#14790 = EDGE_CURVE ( 'NONE', #13665, #22361, #38146, .T. ) ;
#14791 = EDGE_LOOP ( 'NONE', ( #34249, #39366, #27113, #21073 ) ) ;
#14792 = DIRECTION ( 'NONE',  ( -1.000000000000000000, -0.000000000000000000, -0.000000000000000000 ) ) ;
#14793 = ORIENTED_EDGE ( 'NONE', *, *, #7769, .T. ) ;
#14794 = DIRECTION ( 'NONE',  ( 0.000000000000000000, -0.6783118362696222148, 0.7347741508630615259 ) ) ;
#14795 = DIRECTION ( 'NONE',  ( 0.000000000000000000, 0.000000000000000000, 1.000000000000000000 ) ) ;
#14797 = ORIENTED_EDGE ( 'NONE', *, *, #22975, .F. ) ;
#14796 = DIRECTION ( 'NONE',  ( 1.000000000000000000, 0.000000000000000000, 0.000000000000000000 ) ) ;
#14798 = CARTESIAN_POINT ( 'NONE',  ( 17.99999999999999645, 63.24564713401931471, -102.5693868539688651 ) ) ;
#14799 = EDGE_LOOP ( 'NONE', ( #12591, #14302, #19116, #4967, #22410, #7107, #39331, #33392, #15277, #23433, #19643, #20461, #18451, #14163, #6391 ) ) ;
#14800 = LINE ( 'NONE', #38322, #25227 ) ;
#14801 = EDGE_CURVE ( 'NONE', #20222, #32977, #10269, .T. ) ;
#14802 = CARTESIAN_POINT ( 'NONE',  ( -40.67465422008825726, 40.00000000000000000, -82.48404079236435393 ) ) ;
#14803 = CYLINDRICAL_SURFACE ( 'NONE', #31303, 2.100000000000000089 ) ;
#14804 = VECTOR ( 'NONE', #20563, 1000.000000000000000 ) ;
#14805 = CONICAL_SURFACE ( 'NONE', #26646, 2.500000000000000888, 0.9599310885968785900 ) ;
#14806 = ORIENTED_EDGE ( 'NONE', *, *, #11851, .T. ) ;
#14807 = DIRECTION ( 'NONE',  ( 0.000000000000000000, 0.000000000000000000, 1.000000000000000000 ) ) ;
#14808 = CARTESIAN_POINT ( 'NONE',  ( 17.99999999999999645, -14.84191762912334767, 27.78316904333121684 ) ) ;
#14809 = VECTOR ( 'NONE', #41207, 1000.000000000000000 ) ;
#14811 = CARTESIAN_POINT ( 'NONE',  ( 0.000000000000000000, -25.18647942089817349, 113.2326863338526977 ) ) ;
#14810 = DIRECTION ( 'NONE',  ( -1.000000000000000000, 0.000000000000000000, 0.000000000000000000 ) ) ;
#14812 = ORIENTED_EDGE ( 'NONE', *, *, #34223, .F. ) ;
#14813 = CARTESIAN_POINT ( 'NONE',  ( 17.99999999999999645, 0.000000000000000000, 0.000000000000000000 ) ) ;
#14814 = ORIENTED_EDGE ( 'NONE', *, *, #31274, .T. ) ;
#14815 = DIRECTION ( 'NONE',  ( 0.000000000000000000, 0.000000000000000000, 1.000000000000000000 ) ) ;
#14817 = CARTESIAN_POINT ( 'NONE',  ( 9.106956811744730373, 40.00000000000000000, -33.78410985268681799 ) ) ;
#14816 = TOROIDAL_SURFACE ( 'NONE', #7806, 19.59999999999999432, 0.4000000000000001887 ) ;
#14818 = DIRECTION ( 'NONE',  ( -1.000000000000000000, 0.000000000000000000, 0.000000000000000000 ) ) ;
#14819 = DIRECTION ( 'NONE',  ( 0.000000000000000000, 0.2113826236296182937, 0.9774033898178680069 ) ) ;
#14820 = DIRECTION ( 'NONE',  ( 0.000000000000000000, 0.000000000000000000, 1.000000000000000000 ) ) ;
#14821 = ORIENTED_EDGE ( 'NONE', *, *, #19612, .T. ) ;
#14823 = DIRECTION ( 'NONE',  ( -1.000000000000000000, 0.000000000000000000, 0.000000000000000000 ) ) ;
#14822 = CARTESIAN_POINT ( 'NONE',  ( 0.000000000000000000, 3.803237743091921086, 31.26855263151016118 ) ) ;
#14824 = VERTEX_POINT ( 'NONE', #15445 ) ;
#14825 = ADVANCED_FACE ( 'NONE', ( #31790 ), #1877, .F. ) ;
#14826 = CARTESIAN_POINT ( 'NONE',  ( -31.75000000000000000, 0.000000000000000000, 0.000000000000000000 ) ) ;
#14827 = CARTESIAN_POINT ( 'NONE',  ( 17.99999999999999645, 29.86146781000101669, -112.0905559814575696 ) ) ;
#14829 = ADVANCED_FACE ( 'NONE', ( #11947 ), #9718, .T. ) ;
#14828 = CARTESIAN_POINT ( 'NONE',  ( 23.79574588541966662, 31.00000000000000355, -6.380716493563439506 ) ) ;
#14830 = VERTEX_POINT ( 'NONE', #29375 ) ;
#14831 = DIRECTION ( 'NONE',  ( 0.000000000000000000, -0.6783118362696075598, -0.7347741508630751817 ) ) ;
#14832 = CARTESIAN_POINT ( 'NONE',  ( -3.996523416598931009E-15, 2.658563593772952281E-14, 10.00000000000000178 ) ) ;
#14833 = DIRECTION ( 'NONE',  ( -1.000000000000000000, 0.000000000000000000, 0.000000000000000000 ) ) ;
#14834 = AXIS2_PLACEMENT_3D ( 'NONE', #7161, #17025, #20517 ) ;
#14835 = CARTESIAN_POINT ( 'NONE',  ( -47.90394619311608437, 31.00000000000000355, 62.45286580340285099 ) ) ;
#14836 = AXIS2_PLACEMENT_3D ( 'NONE', #4029, #3382, #30245 ) ;
#14837 = ORIENTED_EDGE ( 'NONE', *, *, #24856, .T. ) ;
#14838 = CARTESIAN_POINT ( 'NONE',  ( 24.55685208794459129, 31.00000000000000355, -49.59815698162134368 ) ) ;
#14839 = CIRCLE ( 'NONE', #24625, 19.99999999999999289 ) ;
#14840 = CARTESIAN_POINT ( 'NONE',  ( 84.73112319332513209, 39.99999999999999289, -41.78253223598262167 ) ) ;
#14841 = EDGE_CURVE ( 'NONE', #3472, #34324, #16282, .T. ) ;
#14842 = ORIENTED_EDGE ( 'NONE', *, *, #40197, .F. ) ;
#14843 = AXIS2_PLACEMENT_3D ( 'NONE', #16868, #40148, #24051 ) ;
#14844 = FACE_OUTER_BOUND ( 'NONE', #29335, .T. ) ;
#14845 = DIRECTION ( 'NONE',  ( 1.000000000000000000, 0.000000000000000000, -6.546126324440850663E-16 ) ) ;
#14846 = DIRECTION ( 'NONE',  ( -1.000000000000000000, -0.000000000000000000, -0.000000000000000000 ) ) ;
#14848 = ORIENTED_EDGE ( 'NONE', *, *, #31800, .F. ) ;
#14847 = DIRECTION ( 'NONE',  ( 0.000000000000000000, 0.1062934856473589651, 0.9943348002101377592 ) ) ;
#14849 = DIRECTION ( 'NONE',  ( -1.000000000000000000, -0.000000000000000000, -0.000000000000000000 ) ) ;
#14850 = DIRECTION ( 'NONE',  ( -3.996523416598930318E-16, 2.658563593772947863E-15, 1.000000000000000000 ) ) ;
#14851 = EDGE_CURVE ( 'NONE', #27145, #34791, #36039, .T. ) ;
#14852 = ORIENTED_EDGE ( 'NONE', *, *, #26962, .T. ) ;
#14853 = CARTESIAN_POINT ( 'NONE',  ( 62.51641183113888900, 39.99999999999999289, -16.75201923384928548 ) ) ;
#14854 = DIRECTION ( 'NONE',  ( 0.000000000000000000, 0.000000000000000000, 1.000000000000000000 ) ) ;
#14855 = VERTEX_POINT ( 'NONE', #35879 ) ;
#14856 = EDGE_CURVE ( 'NONE', #24696, #42589, #33481, .T. ) ;
#14857 = CARTESIAN_POINT ( 'NONE',  ( 9.000000000000001776, -11.65176648920959757, -115.4133282497343487 ) ) ;
#14858 = CARTESIAN_POINT ( 'NONE',  ( 18.00000000000000355, -37.91532898920899441, -28.61088654061679648 ) ) ;
#14859 = ORIENTED_EDGE ( 'NONE', *, *, #39407, .T. ) ;
#14860 = DIRECTION ( 'NONE',  ( 0.000000000000000000, 0.000000000000000000, -1.000000000000000000 ) ) ;
#14861 = EDGE_LOOP ( 'NONE', ( #16143, #19178, #11205, #25313 ) ) ;
#14862 = AXIS2_PLACEMENT_3D ( 'NONE', #18128, #21617, #30951 ) ;
#14863 = CARTESIAN_POINT ( 'NONE',  ( 17.99999999999999645, 0.000000000000000000, 0.000000000000000000 ) ) ;
#14864 = ORIENTED_EDGE ( 'NONE', *, *, #4140, .T. ) ;
#14865 = LINE ( 'NONE', #28165, #35538 ) ;
#14866 = CARTESIAN_POINT ( 'NONE',  ( 17.99999999999999645, 0.000000000000000000, 0.000000000000000000 ) ) ;
#14867 = ORIENTED_EDGE ( 'NONE', *, *, #17366, .T. ) ;
#14868 = AXIS2_PLACEMENT_3D ( 'NONE', #28963, #12593, #25910 ) ;
#14869 = DIRECTION ( 'NONE',  ( 1.000000000000000000, 0.000000000000000000, 0.000000000000000000 ) ) ;
#14870 = CARTESIAN_POINT ( 'NONE',  ( 17.99999999999999645, 0.000000000000000000, 130.0000000000000000 ) ) ;
#14871 = ORIENTED_EDGE ( 'NONE', *, *, #28371, .F. ) ;
#14872 = CARTESIAN_POINT ( 'NONE',  ( 17.99999999999999645, -12.42760411676013810, -33.78690065568439138 ) ) ;
#14873 = CIRCLE ( 'NONE', #10674, 116.0000000000000000 ) ;
#14874 = CARTESIAN_POINT ( 'NONE',  ( 0.000000000000000000, 51.93417535146742381, -2.615612846549375536 ) ) ;
#14875 = EDGE_CURVE ( 'NONE', #37240, #10495, #13071, .T. ) ;
#14876 = EDGE_CURVE ( 'NONE', #19395, #27222, #21483, .T. ) ;
#14877 = VERTEX_POINT ( 'NONE', #10135 ) ;
#14878 = DIRECTION ( 'NONE',  ( -1.000000000000000000, -0.000000000000000000, -0.000000000000000000 ) ) ;
#14879 = EDGE_CURVE ( 'NONE', #31728, #22071, #3568, .T. ) ;
#14880 = ADVANCED_FACE ( 'NONE', ( #6645 ), #9921, .T. ) ;
#14881 = EDGE_CURVE ( 'NONE', #30882, #11023, #11708, .T. ) ;
#14882 = LINE ( 'NONE', #33834, #15908 ) ;
#14883 = SHAPE_DEFINITION_REPRESENTATION ( #13411, #9026 ) ;
#14884 = DIRECTION ( 'NONE',  ( -1.000000000000000000, -0.000000000000000000, 0.000000000000000000 ) ) ;
#14885 = CARTESIAN_POINT ( 'NONE',  ( 17.07784400123870938, 31.00000000000000355, -50.31546185293520779 ) ) ;
#14886 = ORIENTED_EDGE ( 'NONE', *, *, #12995, .F. ) ;
#14888 = DIRECTION ( 'NONE',  ( 0.000000000000000000, 0.9213119778704139673, -0.3888241754733182676 ) ) ;
#14887 = DIRECTION ( 'NONE',  ( -1.000000000000000000, 0.000000000000000000, -0.000000000000000000 ) ) ;
#14889 = LINE ( 'NONE', #4370, #29800 ) ;
#14890 = ORIENTED_EDGE ( 'NONE', *, *, #22139, .F. ) ;
#14891 = DIRECTION ( 'NONE',  ( 1.000000000000000000, 0.000000000000000000, 0.000000000000000000 ) ) ;
#14892 = CARTESIAN_POINT ( 'NONE',  ( -60.10416666555506993, 40.00000000000000711, -3.926990808566252156 ) ) ;
#14893 = CARTESIAN_POINT ( 'NONE',  ( 7.251580242022520828, 40.00000000000000000, -54.34182998362662431 ) ) ;
#14894 = AXIS2_PLACEMENT_3D ( 'NONE', #24166, #18284, #31549 ) ;
#14895 = FACE_OUTER_BOUND ( 'NONE', #32661, .T. ) ;
#14896 = DIRECTION ( 'NONE',  ( -1.000000000000000000, -0.000000000000000000, -0.000000000000000000 ) ) ;
#14897 = CARTESIAN_POINT ( 'NONE',  ( 22.90854556226730310, -35.35525454449573601, -74.83297477053802993 ) ) ;
#14898 = CARTESIAN_POINT ( 'NONE',  ( 0.000000000000000000, 0.000000000000000000, 0.000000000000000000 ) ) ;
#14899 = PRESENTATION_LAYER_ASSIGNMENT (  '', '', ( #26029 ) ) ;
#14900 = ADVANCED_FACE ( 'NONE', ( #36106 ), #26519, .T. ) ;
#14901 = ORIENTED_EDGE ( 'NONE', *, *, #40228, .T. ) ;
#14902 = CARTESIAN_POINT ( 'NONE',  ( 34.56606645648713538, 40.00000000000000000, -4.560848911255810378 ) ) ;
#14903 = VERTEX_POINT ( 'NONE', #6010 ) ;
#14904 = DIRECTION ( 'NONE',  ( 0.000000000000000000, 0.8993121301712202476, -0.4373073204588531770 ) ) ;
#14905 = VECTOR ( 'NONE', #28989, 1000.000000000000000 ) ;
#14906 = CARTESIAN_POINT ( 'NONE',  ( -1.360585162435467455, 4.061296242128285883, -3.505054077164959203 ) ) ;
#14907 = ORIENTED_EDGE ( 'NONE', *, *, #37157, .T. ) ;
#14908 = EDGE_CURVE ( 'NONE', #30500, #32325, #32632, .T. ) ;
#14909 = FACE_OUTER_BOUND ( 'NONE', #8045, .T. ) ;
#14910 = CARTESIAN_POINT ( 'NONE',  ( 17.99999999999999645, -95.31344542257777164, 66.11616384574416827 ) ) ;
#14911 = ORIENTED_EDGE ( 'NONE', *, *, #30113, .F. ) ;
#14912 = CARTESIAN_POINT ( 'NONE',  ( 0.000000000000000000, 27.79676263918241119, -37.88001506494740056 ) ) ;
#14913 = ORIENTED_EDGE ( 'NONE', *, *, #26227, .F. ) ;
#14914 = CIRCLE ( 'NONE', #7201, 20.00000000000000711 ) ;
#14915 = ORIENTED_EDGE ( 'NONE', *, *, #36976, .F. ) ;
#14916 = DIRECTION ( 'NONE',  ( -1.000000000000000000, -0.000000000000000000, -0.000000000000000000 ) ) ;
#14917 = CARTESIAN_POINT ( 'NONE',  ( 22.12550800842194931, 31.00000000000000355, 65.48657384636695156 ) ) ;
#14918 = VECTOR ( 'NONE', #32558, 1000.000000000000000 ) ;
#14919 = ORIENTED_EDGE ( 'NONE', *, *, #22326, .F. ) ;
#14920 = DIRECTION ( 'NONE',  ( -1.000000000000000000, -0.000000000000000000, 0.000000000000000000 ) ) ;
#14921 = AXIS2_PLACEMENT_3D ( 'NONE', #22836, #36086, #5986 ) ;
#14922 = CARTESIAN_POINT ( 'NONE',  ( -93.98204972788910538, -2.055254544495720648, 39.37702493556011518 ) ) ;
#14923 = VERTEX_POINT ( 'NONE', #16071 ) ;
#14924 = CARTESIAN_POINT ( 'NONE',  ( 18.00000000000000355, -44.47301969247432396, -16.68249143361957465 ) ) ;
#14925 = ORIENTED_EDGE ( 'NONE', *, *, #25713, .F. ) ;
#14926 = VECTOR ( 'NONE', #34028, 1000.000000000000000 ) ;
#14927 = CARTESIAN_POINT ( 'NONE',  ( -5.980347265640406640, 40.00000000000000000, 89.59238221261722401 ) ) ;
#14928 = CARTESIAN_POINT ( 'NONE',  ( 12.72035051019680729, 31.00000000000000355, 25.87482915247129611 ) ) ;
#14930 = CARTESIAN_POINT ( 'NONE',  ( -10.00000000000000000, 0.000000000000000000, 0.000000000000000000 ) ) ;
#14929 = CARTESIAN_POINT ( 'NONE',  ( 17.99999999999999645, 32.49609705003704363, 15.49205204337285657 ) ) ;
#14931 = EDGE_CURVE ( 'NONE', #42055, #8238, #26363, .T. ) ;
#14932 = EDGE_CURVE ( 'NONE', #18546, #20442, #29823, .T. ) ;
#14933 = DIRECTION ( 'NONE',  ( 0.000000000000000000, 0.000000000000000000, 1.000000000000000000 ) ) ;
#14934 = DIRECTION ( 'NONE',  ( 0.000000000000000000, -0.8183027759081623609, -0.5747874102144165942 ) ) ;
#14935 = ORIENTED_EDGE ( 'NONE', *, *, #18891, .T. ) ;
#14936 =( NAMED_UNIT ( * ) PLANE_ANGLE_UNIT ( ) SI_UNIT ( $, .RADIAN. ) );
#14937 = ADVANCED_FACE ( 'NONE', ( #23270 ), #26319, .T. ) ;
#14938 = CARTESIAN_POINT ( 'NONE',  ( 17.99999999999999645, 0.000000000000000000, 0.000000000000000000 ) ) ;
#14939 = VECTOR ( 'NONE', #9057, 1000.000000000000000 ) ;
#14940 = EDGE_LOOP ( 'NONE', ( #36467, #3586, #28027, #19294 ) ) ;
#14941 = DIRECTION ( 'NONE',  ( -1.000000000000000000, 0.000000000000000000, 0.000000000000000000 ) ) ;
#14942 = DIRECTION ( 'NONE',  ( -1.000000000000000000, -0.000000000000000000, 0.000000000000000000 ) ) ;
#14943 = DIRECTION ( 'NONE',  ( 0.000000000000000000, 0.000000000000000000, -1.000000000000000000 ) ) ;
#14944 = ORIENTED_EDGE ( 'NONE', *, *, #17864, .F. ) ;
#14945 = CIRCLE ( 'NONE', #14240, 47.49900000000000944 ) ;
#14946 = CARTESIAN_POINT ( 'NONE',  ( -1.587008504153756938, 40.00000000000000000, -24.39691638390478090 ) ) ;
#14947 = VERTEX_POINT ( 'NONE', #2920 ) ;
#14948 = AXIS2_PLACEMENT_3D ( 'NONE', #32836, #13012, #26315 ) ;
#14949 = ADVANCED_FACE ( 'NONE', ( #16512 ), #13016, .F. ) ;
#14950 = ORIENTED_EDGE ( 'NONE', *, *, #36251, .F. ) ;
#14951 = CARTESIAN_POINT ( 'NONE',  ( 17.99999999999999645, -25.18647942089668490, -113.2326863338530245 ) ) ;
#14952 = DIRECTION ( 'NONE',  ( -1.000000000000000000, 0.000000000000000000, 0.000000000000000000 ) ) ;
#14953 = FACE_OUTER_BOUND ( 'NONE', #20971, .T. ) ;
#14954 = VECTOR ( 'NONE', #41236, 1000.000000000000000 ) ;
#14955 = PLANE ( 'NONE',  #42083 ) ;
#14956 = ORIENTED_EDGE ( 'NONE', *, *, #8861, .F. ) ;
#14957 = CARTESIAN_POINT ( 'NONE',  ( -106.4195705685748550, -106.4195705685759776, 9.999999999999998224 ) ) ;
#14958 = VERTEX_POINT ( 'NONE', #20008 ) ;
#14959 = CARTESIAN_POINT ( 'NONE',  ( 0.000000000000000000, -0.04937522221101428577, -31.94951095880159286 ) ) ;
#14960 = CARTESIAN_POINT ( 'NONE',  ( -10.00000000000000000, 0.000000000000000000, 0.000000000000000000 ) ) ;
#14961 = CARTESIAN_POINT ( 'NONE',  ( 18.00000000000000355, -0.2227391519119825691, 46.98410307550729215 ) ) ;
#14962 = FACE_OUTER_BOUND ( 'NONE', #18100, .T. ) ;
#14963 = ORIENTED_EDGE ( 'NONE', *, *, #10055, .T. ) ;
#14964 = EDGE_CURVE ( 'NONE', #9297, #16728, #33277, .T. ) ;
#14965 = ORIENTED_EDGE ( 'NONE', *, *, #12257, .F. ) ;
#14966 = DIRECTION ( 'NONE',  ( 1.000000000000000000, 0.000000000000000000, 0.000000000000000000 ) ) ;
#14967 = AXIS2_PLACEMENT_3D ( 'NONE', #11825, #18388, #38832 ) ;
#14968 = CARTESIAN_POINT ( 'NONE',  ( 33.40854556226729954, -35.35525454449573601, -74.83297477053802993 ) ) ;
#14969 = VECTOR ( 'NONE', #2904, 1000.000000000000000 ) ;
#14970 = ORIENTED_EDGE ( 'NONE', *, *, #28876, .F. ) ;
#14972 = VERTEX_POINT ( 'NONE', #14094 ) ;
#14971 = DIRECTION ( 'NONE',  ( -1.000000000000000000, 0.000000000000000000, 0.000000000000000000 ) ) ;
#14973 = CARTESIAN_POINT ( 'NONE',  ( -32.60815990948594134, 31.00000000000000355, 24.92795611697640368 ) ) ;
#14974 = EDGE_LOOP ( 'NONE', ( #11455, #10767, #4298, #12695 ) ) ;
#14975 = DIRECTION ( 'NONE',  ( -1.000000000000000000, 0.000000000000000000, -0.000000000000000000 ) ) ;
#14976 = AXIS2_PLACEMENT_3D ( 'NONE', #38123, #25293, #5172 ) ;
#14977 = DIRECTION ( 'NONE',  ( 0.000000000000000000, 0.9996456111234524045, 0.02662052143777833904 ) ) ;
#14978 = AXIS2_PLACEMENT_3D ( 'NONE', #35738, #29893, #19861 ) ;
#14979 = ORIENTED_EDGE ( 'NONE', *, *, #988, .T. ) ;
#14980 = FACE_OUTER_BOUND ( 'NONE', #9138, .T. ) ;
#14981 = CARTESIAN_POINT ( 'NONE',  ( -31.81746463534672387, 40.00000000000000000, -55.29958784370776925 ) ) ;
#14982 = AXIS2_PLACEMENT_3D ( 'NONE', #12733, #9228, #25841 ) ;
#14983 = DIRECTION ( 'NONE',  ( -1.000000000000000000, -0.000000000000000000, 0.000000000000000000 ) ) ;
#14984 = AXIS2_PLACEMENT_3D ( 'NONE', #25736, #35705, #2955 ) ;
#14985 = ADVANCED_FACE ( 'NONE', ( #4672 ), #40875, .F. ) ;
#14986 = DIRECTION ( 'NONE',  ( 0.000000000000000000, -0.9048270524660145808, -0.4257792915650830956 ) ) ;
#14987 = VERTEX_POINT ( 'NONE', #1174 ) ;
#14988 = CARTESIAN_POINT ( 'NONE',  ( -15.99999999999997691, 31.00000000000000711, 4.500000000000005329 ) ) ;
#14989 = VERTEX_POINT ( 'NONE', #17809 ) ;
#14990 = AXIS2_PLACEMENT_3D ( 'NONE', #4067, #13080, #23972 ) ;
#14991 = B_SPLINE_CURVE_WITH_KNOTS ( 'NONE', 3,
 ( #5790, #19146, #5584, #15642, #25071, #28739 ),
 .UNSPECIFIED., .F., .F.,
 ( 4, 2, 4 ),
 ( 0.002365888236227995517, 0.003551327329835084114, 0.004736766423442172712 ),
 .UNSPECIFIED. ) ;
#14992 = CARTESIAN_POINT ( 'NONE',  ( 17.99999999999999645, 12.42760411676038323, 33.78690065568429191 ) ) ;
#14993 = DIRECTION ( 'NONE',  ( -1.000000000000000000, 0.000000000000000000, 0.000000000000000000 ) ) ;
#14994 = CARTESIAN_POINT ( 'NONE',  ( -63.57631528421845957, 31.00000000000000711, -31.33741679916209222 ) ) ;
#14995 = DIRECTION ( 'NONE',  ( 0.000000000000000000, 0.000000000000000000, -1.000000000000000000 ) ) ;
#14996 = ORIENTED_EDGE ( 'NONE', *, *, #24496, .T. ) ;
#14997 = EDGE_CURVE ( 'NONE', #9269, #36784, #16605, .T. ) ;
#14998 = VECTOR ( 'NONE', #2479, 1000.000000000000000 ) ;
#14999 = DIRECTION ( 'NONE',  ( -1.000000000000000000, 0.000000000000000000, 0.000000000000000000 ) ) ;
#15000 = EDGE_CURVE ( 'NONE', #30041, #37276, #14294, .T. ) ;
#15001 = ORIENTED_EDGE ( 'NONE', *, *, #4411, .T. ) ;
#15002 = DIRECTION ( 'NONE',  ( -1.000000000000000000, -0.000000000000000000, -0.000000000000000000 ) ) ;
#15003 = DIRECTION ( 'NONE',  ( -1.000000000000000000, 0.000000000000000000, 0.000000000000000000 ) ) ;
#15004 = CARTESIAN_POINT ( 'NONE',  ( 84.58694138809386232, 31.00000000000000000, 22.77597867319729374 ) ) ;
#15005 = CARTESIAN_POINT ( 'NONE',  ( 86.90011881125597881, 39.99999999999999289, -5.573058087428396590 ) ) ;
#15006 = EDGE_CURVE ( 'NONE', #14549, #9049, #13131, .T. ) ;
#15007 = CARTESIAN_POINT ( 'NONE',  ( 17.99999999999999645, 0.000000000000000000, 0.000000000000000000 ) ) ;
#15008 = VECTOR ( 'NONE', #33712, 1000.000000000000000 ) ;
#15009 = VERTEX_POINT ( 'NONE', #41085 ) ;
#15010 = DIRECTION ( 'NONE',  ( -1.000000000000000000, -0.000000000000000000, -0.000000000000000000 ) ) ;
#15011 = VERTEX_POINT ( 'NONE', #27605 ) ;
#15012 = CARTESIAN_POINT ( 'NONE',  ( -31.75000000000000711, 19.19999999999999574, 0.000000000000000000 ) ) ;
#15013 = CIRCLE ( 'NONE', #1033, 51.99999999999999289 ) ;
#15014 = DIRECTION ( 'NONE',  ( 0.000000000000000000, 1.000000000000000000, 1.224646799147353207E-16 ) ) ;
#15016 = ORIENTED_EDGE ( 'NONE', *, *, #36911, .T. ) ;
#15015 = DIRECTION ( 'NONE',  ( 0.000000000000000000, 0.000000000000000000, 1.000000000000000000 ) ) ;
#15017 = PLANE ( 'NONE',  #31685 ) ;
#15018 = ORIENTED_EDGE ( 'NONE', *, *, #35442, .F. ) ;
#15019 = CARTESIAN_POINT ( 'NONE',  ( 1.567478505476134606E-15, 4.618802153517012066, -3.433295621305382905 ) ) ;
#15020 = AXIS2_PLACEMENT_3D ( 'NONE', #34566, #4232, #41540 ) ;
#15021 = CARTESIAN_POINT ( 'NONE',  ( 92.36625196220676060, 39.99999999999999289, 24.73319171124347093 ) ) ;
#15022 = CARTESIAN_POINT ( 'NONE',  ( 0.000000000000000000, 115.5737863835462349, 9.934782381634081005 ) ) ;
#15023 = EDGE_CURVE ( 'NONE', #22307, #30436, #37397, .T. ) ;
#15024 = ORIENTED_EDGE ( 'NONE', *, *, #25625, .F. ) ;
#15025 = CARTESIAN_POINT ( 'NONE',  ( 17.99999999999999645, 120.4984140710909202, 0.7894348306988416830 ) ) ;
#15026 = DIRECTION ( 'NONE',  ( 0.000000000000000000, 0.8443279255020125218, 0.5358267949790006535 ) ) ;
#15028 = LINE ( 'NONE', #11758, #24829 ) ;
#15027 = DIRECTION ( 'NONE',  ( -1.000000000000000000, 0.000000000000000000, 0.000000000000000000 ) ) ;
#15029 = ORIENTED_EDGE ( 'NONE', *, *, #11833, .T. ) ;
#15030 = LINE ( 'NONE', #39176, #9379 ) ;
#15031 = ORIENTED_EDGE ( 'NONE', *, *, #15620, .F. ) ;
#15032 = DIRECTION ( 'NONE',  ( 0.000000000000000000, 1.000000000000000000, 0.000000000000000000 ) ) ;
#15034 = CIRCLE ( 'NONE', #21339, 13.59999999999999964 ) ;
#15033 = CARTESIAN_POINT ( 'NONE',  ( -31.59164309906362078, 40.00000000000000000, 4.115917706318550806 ) ) ;
#15035 = CARTESIAN_POINT ( 'NONE',  ( 17.99999999999999645, 0.000000000000000000, 0.000000000000000000 ) ) ;
#15036 = VECTOR ( 'NONE', #33252, 1000.000000000000000 ) ;
#15037 = CYLINDRICAL_SURFACE ( 'NONE', #30516, 58.99999999999998579 ) ;
#15038 = DIRECTION ( 'NONE',  ( 0.000000000000000000, 0.000000000000000000, 1.000000000000000000 ) ) ;
#15040 = ORIENTED_EDGE ( 'NONE', *, *, #37930, .F. ) ;
#15039 = AXIS2_PLACEMENT_3D ( 'NONE', #20242, #36772, #3799 ) ;
#15041 = CARTESIAN_POINT ( 'NONE',  ( -0.1750025118121544265, -4.719839900820635314, -3.469254087858253399 ) ) ;
#15042 = EDGE_CURVE ( 'NONE', #39753, #16742, #14739, .T. ) ;
#15043 = CIRCLE ( 'NONE', #36599, 13.59999999999999964 ) ;
#15044 = VERTEX_POINT ( 'NONE', #18044 ) ;
#15045 = AXIS2_PLACEMENT_3D ( 'NONE', #30714, #26787, #34184 ) ;
#15046 = FACE_OUTER_BOUND ( 'NONE', #42703, .T. ) ;
#15047 = LINE ( 'NONE', #2115, #41499 ) ;
#15048 = CIRCLE ( 'NONE', #36607, 58.99999999999999289 ) ;
#15049 = CARTESIAN_POINT ( 'NONE',  ( 28.66079171547214699, 31.00000000000000355, 21.97938003711830035 ) ) ;
#15050 = ORIENTED_EDGE ( 'NONE', *, *, #4062, .F. ) ;
#15051 = CARTESIAN_POINT ( 'NONE',  ( 0.000000000000000000, 27.43636312076321104, 38.14186064215159888 ) ) ;
#15052 = PRESENTATION_LAYER_ASSIGNMENT (  '', '', ( #9426 ) ) ;
#15053 = ITEM_DEFINED_TRANSFORMATION ( 'NONE', 'NONE', #14967,  #13552 ) ;
#15054 = EDGE_CURVE ( 'NONE', #34854, #10716, #24570, .T. ) ;
#15056 = AXIS2_PLACEMENT_3D ( 'NONE', #40605, #41045, #10748 ) ;
#15055 = DIRECTION ( 'NONE',  ( 1.000000000000000000, 0.000000000000000000, 0.000000000000000000 ) ) ;
#15057 = CARTESIAN_POINT ( 'NONE',  ( -20.19574676229028043, 31.00000000000000355, 75.42596061005518493 ) ) ;
#15058 = EDGE_CURVE ( 'NONE', #37680, #16448, #34007, .T. ) ;
#15059 = ORIENTED_EDGE ( 'NONE', *, *, #15856, .F. ) ;
#15060 = CARTESIAN_POINT ( 'NONE',  ( -32.53655534684842365, 31.00000000000000355, -42.55839752837237455 ) ) ;
#15061 = CARTESIAN_POINT ( 'NONE',  ( -60.37409795221152109, 40.00000000000000711, -68.82020352599361956 ) ) ;
#15062 = ORIENTED_EDGE ( 'NONE', *, *, #16383, .F. ) ;
#15063 = FACE_OUTER_BOUND ( 'NONE', #21524, .T. ) ;
#15064 = CARTESIAN_POINT ( 'NONE',  ( 0.000000000000000000, 0.000000000000000000, 0.000000000000000000 ) ) ;
#15065 = CYLINDRICAL_SURFACE ( 'NONE', #9387, 47.49900000000000233 ) ;
#15067 = ORIENTED_EDGE ( 'NONE', *, *, #3043, .T. ) ;
#15066 = DIRECTION ( 'NONE',  ( 1.000000000000000000, 0.000000000000000000, 0.000000000000000000 ) ) ;
#15068 = AXIS2_PLACEMENT_3D ( 'NONE', #37892, #8244, #22014 ) ;
#15069 = DIRECTION ( 'NONE',  ( -1.000000000000000000, 0.000000000000000000, 0.000000000000000000 ) ) ;
#15070 = CIRCLE ( 'NONE', #28976, 15.00000000000000178 ) ;
#15071 = CARTESIAN_POINT ( 'NONE',  ( 0.000000000000000000, 34.45183346761135113, 10.44371441202667761 ) ) ;
#15072 = VECTOR ( 'NONE', #26311, 1000.000000000000114 ) ;
#15073 = EDGE_LOOP ( 'NONE', ( #15502, #22963, #21427, #28057 ) ) ;
#15074 = CARTESIAN_POINT ( 'NONE',  ( -48.53848235557606472, 40.00000000000000000, -37.22912483484027035 ) ) ;
#15075 = DIRECTION ( 'NONE',  ( 0.000000000000000000, 0.000000000000000000, 1.000000000000000000 ) ) ;
#15076 = EDGE_CURVE ( 'NONE', #15150, #31530, #40932, .T. ) ;
#15077 = AXIS2_PLACEMENT_3D ( 'NONE', #38459, #34775, #42151 ) ;
#15078 = ORIENTED_EDGE ( 'NONE', *, *, #6428, .F. ) ;
#15079 = CIRCLE ( 'NONE', #39403, 25.00000000000000000 ) ;
#15080 = EDGE_CURVE ( 'NONE', #38421, #43113, #34558, .T. ) ;
#15081 = DIRECTION ( 'NONE',  ( 1.000000000000000000, 0.000000000000000000, 0.000000000000000000 ) ) ;
#15082 = CARTESIAN_POINT ( 'NONE',  ( 0.000000000000000000, 0.000000000000000000, 0.000000000000000000 ) ) ;
#15083 = AXIS2_PLACEMENT_3D ( 'NONE', #22572, #36630, #33375 ) ;
#15084 = AXIS2_PLACEMENT_3D ( 'NONE', #20824, #37561, #34077 ) ;
#15085 = CARTESIAN_POINT ( 'NONE',  ( 17.99999999999999645, 84.62908780824989208, -85.78116633471202590 ) ) ;
#15086 = VERTEX_POINT ( 'NONE', #34340 ) ;
#15087 = VECTOR ( 'NONE', #31681, 1000.000000000000000 ) ;
#15088 = ORIENTED_EDGE ( 'NONE', *, *, #41659, .T. ) ;
#15089 = DIRECTION ( 'NONE',  ( -1.000000000000000000, -0.000000000000000000, -0.000000000000000000 ) ) ;
#15090 = ORIENTED_EDGE ( 'NONE', *, *, #13067, .F. ) ;
#15091 = CARTESIAN_POINT ( 'NONE',  ( 0.000000000000000000, 0.000000000000000000, 0.000000000000000000 ) ) ;
#15092 = DIRECTION ( 'NONE',  ( 0.000000000000000000, 0.000000000000000000, 1.000000000000000000 ) ) ;
#15093 = DIRECTION ( 'NONE',  ( 0.000000000000000000, 0.000000000000000000, 1.000000000000000000 ) ) ;
#15094 = DIRECTION ( 'NONE',  ( -1.000000000000000000, 0.000000000000000000, -0.000000000000000000 ) ) ;
#15095 = ORIENTED_EDGE ( 'NONE', *, *, #12108, .F. ) ;
#15096 = CARTESIAN_POINT ( 'NONE',  ( -10.00000000000000000, 0.000000000000000000, 0.000000000000000000 ) ) ;
#15097 = LINE ( 'NONE', #8302, #5023 ) ;
#15099 = ORIENTED_EDGE ( 'NONE', *, *, #27755, .T. ) ;
#15098 = VECTOR ( 'NONE', #29008, 1000.000000000000000 ) ;
#15100 = CYLINDRICAL_SURFACE ( 'NONE', #22516, 120.5010000000000190 ) ;
#15101 = VECTOR ( 'NONE', #33567, 1000.000000000000000 ) ;
#15102 = FACE_OUTER_BOUND ( 'NONE', #5655, .T. ) ;
#15103 = CIRCLE ( 'NONE', #26909, 19.99999999999989342 ) ;
#15104 = VECTOR ( 'NONE', #28312, 1000.000000000000000 ) ;
#15105 = DIRECTION ( 'NONE',  ( 0.7071067811865463515, -6.123233995736766036E-17, -0.7071067811865487940 ) ) ;
#15106 = EDGE_CURVE ( 'NONE', #7888, #42671, #17383, .T. ) ;
#15107 = DIRECTION ( 'NONE',  ( 0.000000000000000000, 1.000000000000000000, 0.000000000000000000 ) ) ;
#15108 = CARTESIAN_POINT ( 'NONE',  ( -22.94860596549062848, 31.00000000000000355, -46.53072237555588231 ) ) ;
#15109 = ORIENTED_EDGE ( 'NONE', *, *, #23805, .T. ) ;
#15110 = CONICAL_SURFACE ( 'NONE', #26944, 4.000000000000000000, 0.8911886515913786111 ) ;
#15112 = CARTESIAN_POINT ( 'NONE',  ( 18.00000000000000355, 36.05989434073613609, 30.12041790338630776 ) ) ;
#15111 = DIRECTION ( 'NONE',  ( 0.000000000000000000, -0.2631025642275283127, 0.9647678688145140402 ) ) ;
#15113 = VECTOR ( 'NONE', #12714, 1000.000000000000000 ) ;
#15114 = ADVANCED_FACE ( 'NONE', ( #24129 ), #3774, .T. ) ;
#15115 = VERTEX_POINT ( 'NONE', #17595 ) ;
#15116 = CIRCLE ( 'NONE', #19278, 52.00000000000000000 ) ;
#15117 = CARTESIAN_POINT ( 'NONE',  ( -59.40491426035100631, 40.00000000000000711, 7.833300799371349932 ) ) ;
#15118 = CARTESIAN_POINT ( 'NONE',  ( -9.228224334387265415, 40.00000000000000000, 69.24269282083176336 ) ) ;
#15119 = CARTESIAN_POINT ( 'NONE',  ( -15.99999999999997691, 17.11489954122026447, 5.571627607371296764E-15 ) ) ;
#15120 = DIRECTION ( 'NONE',  ( -1.000000000000000000, 0.000000000000000000, 0.000000000000000000 ) ) ;
#15121 = CIRCLE ( 'NONE', #17941, 20.00000000000000711 ) ;
#15122 = DIRECTION ( 'NONE',  ( 0.000000000000000000, 0.000000000000000000, 1.000000000000000000 ) ) ;
#15123 = CARTESIAN_POINT ( 'NONE',  ( 24.63052733448982323, 31.00000000000000355, -3.251868155982907904 ) ) ;
#15124 = ORIENTED_EDGE ( 'NONE', *, *, #39250, .F. ) ;
#15125 = CARTESIAN_POINT ( 'NONE',  ( 32.71557229150619861, 40.00000000000000000, -11.11602612089219910 ) ) ;
#15126 = ORIENTED_EDGE ( 'NONE', *, *, #36221, .T. ) ;
#15127 = FACE_OUTER_BOUND ( 'NONE', #34253, .T. ) ;
#15128 = CARTESIAN_POINT ( 'NONE',  ( 17.99999999999999645, -80.74349901498459303, 77.90224541347254217 ) ) ;
#15129 = EDGE_CURVE ( 'NONE', #17775, #15772, #6122, .T. ) ;
#15130 = ORIENTED_EDGE ( 'NONE', *, *, #344, .F. ) ;
#15131 = EDGE_CURVE ( 'NONE', #9666, #40313, #32603, .T. ) ;
#15132 = CIRCLE ( 'NONE', #21444, 13.60000000000000320 ) ;
#15133 = DIRECTION ( 'NONE',  ( 1.000000000000000000, 0.000000000000000000, 0.000000000000000000 ) ) ;
#15134 = ADVANCED_FACE ( 'NONE', ( #27173 ), #945, .F. ) ;
#15135 = EDGE_CURVE ( 'NONE', #40496, #30041, #36078, .T. ) ;
#15136 = DIRECTION ( 'NONE',  ( 0.000000000000000000, 0.000000000000000000, 1.000000000000000000 ) ) ;
#15137 = EDGE_LOOP ( 'NONE', ( #22829, #12988 ) ) ;
#15138 = CARTESIAN_POINT ( 'NONE',  ( 18.00000000000000355, -51.85248208264519576, 3.914090171286020325 ) ) ;
#15139 = ORIENTED_EDGE ( 'NONE', *, *, #400, .T. ) ;
#15140 = VECTOR ( 'NONE', #8460, 1000.000000000000000 ) ;
#15141 = AXIS2_PLACEMENT_3D ( 'NONE', #10521, #33427, #3512 ) ;
#15142 = ORIENTED_EDGE ( 'NONE', *, *, #6177, .T. ) ;
#15143 = AXIS2_PLACEMENT_3D ( 'NONE', #16886, #10967, #33633 ) ;
#15144 = DIRECTION ( 'NONE',  ( -1.000000000000000000, 0.000000000000000000, 0.000000000000000000 ) ) ;
#15145 = CARTESIAN_POINT ( 'NONE',  ( 66.32976035609178211, 31.00000000000000000, 58.33333674018341952 ) ) ;
#15146 = ORIENTED_EDGE ( 'NONE', *, *, #29852, .F. ) ;
#15147 = CARTESIAN_POINT ( 'NONE',  ( -4.000000000000000000, -0.8382240730041925492, -3.220610619767135141 ) ) ;
#15148 = CIRCLE ( 'NONE', #39466, 120.5010000000000332 ) ;
#15149 = DIRECTION ( 'NONE',  ( 0.000000000000000000, 0.000000000000000000, 1.000000000000000000 ) ) ;
#15150 = VERTEX_POINT ( 'NONE', #33919 ) ;
#15151 = CARTESIAN_POINT ( 'NONE',  ( -4.198928548860774157, 0.8158838809860065044, -3.526471437616918170 ) ) ;
#15152 = VECTOR ( 'NONE', #28809, 1000.000000000000000 ) ;
#15153 = PLANE ( 'NONE',  #7394 ) ;
#15154 = CIRCLE ( 'NONE', #38189, 116.0000000000000000 ) ;
#15155 = CARTESIAN_POINT ( 'NONE',  ( 11.19416946702030735, 31.00000000000000355, -22.66942529387728555 ) ) ;
#15156 = DIRECTION ( 'NONE',  ( 0.000000000000000000, 0.000000000000000000, 1.000000000000000000 ) ) ;
#15157 = DIRECTION ( 'NONE',  ( 1.058513553088275437E-16, 1.000000000000000000, -8.813324511995299047E-17 ) ) ;
#15158 = DIRECTION ( 'NONE',  ( -1.000000000000000000, 0.000000000000000000, 0.000000000000000000 ) ) ;
#15159 = ORIENTED_EDGE ( 'NONE', *, *, #21394, .T. ) ;
#15160 = EDGE_CURVE ( 'NONE', #24128, #16426, #730, .T. ) ;
#15161 = CARTESIAN_POINT ( 'NONE',  ( -31.74999999999995737, 0.000000000000000000, 0.000000000000000000 ) ) ;
#15162 = ORIENTED_EDGE ( 'NONE', *, *, #29483, .F. ) ;
#15163 = DIRECTION ( 'NONE',  ( 0.000000000000000000, 0.000000000000000000, -1.000000000000000000 ) ) ;
#15164 = DIRECTION ( 'NONE',  ( 0.000000000000000000, 0.000000000000000000, 1.000000000000000000 ) ) ;
#15165 = EDGE_CURVE ( 'NONE', #2401, #5171, #28260, .T. ) ;
#15166 = CYLINDRICAL_SURFACE ( 'NONE', #36676, 2.649999999999985700 ) ;
#15167 = CIRCLE ( 'NONE', #25623, 120.5010000000000616 ) ;
#15168 = ORIENTED_EDGE ( 'NONE', *, *, #39856, .T. ) ;
#15169 = CIRCLE ( 'NONE', #39488, 36.00000000000000000 ) ;
#15170 = CARTESIAN_POINT ( 'NONE',  ( 7.507699080470448649, 40.00000000000000000, 28.16210111025598906 ) ) ;
#15171 = VECTOR ( 'NONE', #38412, 1000.000000000000000 ) ;
#15172 = ORIENTED_EDGE ( 'NONE', *, *, #16142, .F. ) ;
#15173 = AXIS2_PLACEMENT_3D ( 'NONE', #14200, #17708, #9079 ) ;
#15174 = ORIENTED_EDGE ( 'NONE', *, *, #16894, .F. ) ;
#15175 = DIRECTION ( 'NONE',  ( -1.000000000000000000, 0.000000000000000000, 0.000000000000000000 ) ) ;
#15176 = DIRECTION ( 'NONE',  ( -1.000000000000000000, 0.000000000000000000, 0.000000000000000000 ) ) ;
#15177 = CARTESIAN_POINT ( 'NONE',  ( 0.000000000000000000, -23.21237537461820466, 109.7700237000591414 ) ) ;
#15178 = AXIS2_PLACEMENT_3D ( 'NONE', #34996, #31731, #25022 ) ;
#15179 = FACE_BOUND ( 'NONE', #15973, .T. ) ;
#15180 = AXIS2_PLACEMENT_3D ( 'NONE', #23063, #33859, #6429 ) ;
#15181 = CARTESIAN_POINT ( 'NONE',  ( 18.00000000000000355, 36.06787431788676912, 37.45808914225501240 ) ) ;
#15182 = VERTEX_POINT ( 'NONE', #28488 ) ;
#15183 = DIRECTION ( 'NONE',  ( 0.5000000000000013323, -0.8660254037844379305, 0.000000000000000000 ) ) ;
#15184 = VERTEX_POINT ( 'NONE', #18693 ) ;
#15185 = CARTESIAN_POINT ( 'NONE',  ( 17.99999999999999645, -97.19627249181047546, -71.22763238166585609 ) ) ;
#15186 = CARTESIAN_POINT ( 'NONE',  ( 22.90854556226730310, -34.05525454449573175, -74.83297477053802993 ) ) ;
#15187 = AXIS2_PLACEMENT_3D ( 'NONE', #38017, #8144, #4865 ) ;
#15188 = EDGE_CURVE ( 'NONE', #42499, #33862, #6805, .T. ) ;
#15189 = EDGE_CURVE ( 'NONE', #1626, #18362, #38047, .T. ) ;
#15190 = FACE_OUTER_BOUND ( 'NONE', #241, .T. ) ;
#15191 = ADVANCED_FACE ( 'NONE', ( #31951 ), #38467, .F. ) ;
#15192 = EDGE_CURVE ( 'NONE', #23382, #19555, #8911, .T. ) ;
#15193 = LINE ( 'NONE', #42595, #24813 ) ;
#15194 = SHAPE_REPRESENTATION ( 'needle roller bearing_nm_iso_ISO 3030 - 15C2230 - Full,SI,AC,Full', ( #13552 ), #41322 ) ;
#15195 = ORIENTED_EDGE ( 'NONE', *, *, #13519, .T. ) ;
#15196 = ORIENTED_EDGE ( 'NONE', *, *, #40856, .F. ) ;
#15197 = FACE_OUTER_BOUND ( 'NONE', #5225, .T. ) ;
#15198 = DIRECTION ( 'NONE',  ( -1.000000000000000000, 0.000000000000000000, -0.000000000000000000 ) ) ;
#15199 = EDGE_CURVE ( 'NONE', #33331, #14549, #31902, .T. ) ;
#15200 = ORIENTED_EDGE ( 'NONE', *, *, #42423, .F. ) ;
#15202 = ORIENTED_EDGE ( 'NONE', *, *, #5891, .T. ) ;
#15201 = CARTESIAN_POINT ( 'NONE',  ( 0.000000000000000000, 112.8457601792515419, 26.86697618949414945 ) ) ;
#15203 = CARTESIAN_POINT ( 'NONE',  ( -23.74678488967455436, 31.00000000000000355, -48.36925102894097961 ) ) ;
#15204 = ORIENTED_EDGE ( 'NONE', *, *, #10818, .F. ) ;
#15205 = CYLINDRICAL_SURFACE ( 'NONE', #12582, 51.99999999999999289 ) ;
#15206 = AXIS2_PLACEMENT_3D ( 'NONE', #29973, #9674, #36263 ) ;
#15207 = ADVANCED_FACE ( 'NONE', ( #5739 ), #25644, .T. ) ;
#15208 = CIRCLE ( 'NONE', #24232, 120.5010000000000332 ) ;
#15209 = AXIS2_PLACEMENT_3D ( 'NONE', #40922, #24402, #30906 ) ;
#15211 = SURFACE_STYLE_USAGE ( .BOTH. , #4913 ) ;
#15210 = CARTESIAN_POINT ( 'NONE',  ( -4.000000000000000000, 2.309401076758498483, -0.4999999999999927280 ) ) ;
#15212 = ORIENTED_EDGE ( 'NONE', *, *, #42017, .F. ) ;
#15213 = CIRCLE ( 'NONE', #1919, 59.00000000000000711 ) ;
#15214 = CARTESIAN_POINT ( 'NONE',  ( -48.39074809477736494, 40.00000000000000000, -55.33250407649475733 ) ) ;
#15215 = AXIS2_PLACEMENT_3D ( 'NONE', #18743, #15010, #42435 ) ;
#15216 = AXIS2_PLACEMENT_3D ( 'NONE', #40602, #27126, #36692 ) ;
#15217 = LINE ( 'NONE', #31111, #6137 ) ;
#15218 = CARTESIAN_POINT ( 'NONE',  ( 0.000000000000000000, 30.74337109795208178, 8.695908345466650147 ) ) ;
#15219 = ORIENTED_EDGE ( 'NONE', *, *, #34270, .T. ) ;
#15220 = CARTESIAN_POINT ( 'NONE',  ( -109.0695705685755996, 106.4195705685752529, 10.00000000000000000 ) ) ;
#15221 = ORIENTED_EDGE ( 'NONE', *, *, #28143, .T. ) ;
#15222 = FILL_AREA_STYLE_COLOUR ( '', #11397 ) ;
#15223 = CARTESIAN_POINT ( 'NONE',  ( 0.000000000000000000, -35.72777019205596361, -106.3569410558020962 ) ) ;
#15224 = DIRECTION ( 'NONE',  ( 1.000000000000000000, 0.000000000000000000, -0.000000000000000000 ) ) ;
#15225 = AXIS2_PLACEMENT_3D ( 'NONE', #24879, #25298, #38129 ) ;
#15226 = CARTESIAN_POINT ( 'NONE',  ( 57.13603463884887645, 31.00000000000000355, 32.98675068510902264 ) ) ;
#15227 = FACE_OUTER_BOUND ( 'NONE', #36399, .T. ) ;
#15228 = ORIENTED_EDGE ( 'NONE', *, *, #13345, .T. ) ;
#15229 = ADVANCED_FACE ( 'NONE', ( #21532 ), #5098, .T. ) ;
#15230 = FILL_AREA_STYLE_COLOUR ( '', #12906 ) ;
#15231 = ORIENTED_EDGE ( 'NONE', *, *, #26453, .F. ) ;
#15232 = DIRECTION ( 'NONE',  ( -1.000000000000000000, -0.000000000000000000, -0.000000000000000000 ) ) ;
#15233 = CARTESIAN_POINT ( 'NONE',  ( 17.99999999999999645, 69.90696807222488474, 98.15042952503540619 ) ) ;
#15234 = CIRCLE ( 'NONE', #39553, 58.99999999999998579 ) ;
#15235 = CARTESIAN_POINT ( 'NONE',  ( 83.84057477258951963, 31.00000000000000000, -22.33845567675551180 ) ) ;
#15236 = CARTESIAN_POINT ( 'NONE',  ( -65.95487968126425926, 40.00000000000000711, -50.74205456615700882 ) ) ;
#15237 = DIRECTION ( 'NONE',  ( 0.000000000000000000, 0.000000000000000000, 1.000000000000000000 ) ) ;
#15238 = CIRCLE ( 'NONE', #18712, 20.00000000000001066 ) ;
#15239 = CIRCLE ( 'NONE', #12445, 13.59999999999999964 ) ;
#15240 = ORIENTED_EDGE ( 'NONE', *, *, #3748, .F. ) ;
#15241 = CARTESIAN_POINT ( 'NONE',  ( 17.99999999999999645, -56.51398178981757070, -96.92493144647505687 ) ) ;
#15242 = AXIS2_PLACEMENT_3D ( 'NONE', #41284, #24765, #38021 ) ;
#15243 = ORIENTED_EDGE ( 'NONE', *, *, #3139, .T. ) ;
#15244 = AXIS2_PLACEMENT_3D ( 'NONE', #28895, #24786, #8584 ) ;
#15245 = DIRECTION ( 'NONE',  ( -1.000000000000000000, 0.000000000000000000, 0.000000000000000000 ) ) ;
#15246 = FACE_OUTER_BOUND ( 'NONE', #6969, .T. ) ;
#15247 = VECTOR ( 'NONE', #42538, 1000.000000000000000 ) ;
#15249 = ORIENTED_EDGE ( 'NONE', *, *, #28371, .T. ) ;
#15248 = DIRECTION ( 'NONE',  ( -1.000000000000000000, -0.000000000000000000, 0.000000000000000000 ) ) ;
#15250 = EDGE_CURVE ( 'NONE', #33958, #33515, #21516, .T. ) ;
#15251 = EDGE_CURVE ( 'NONE', #1962, #16404, #35373, .T. ) ;
#15252 = FACE_OUTER_BOUND ( 'NONE', #30204, .T. ) ;
#15253 = ORIENTED_EDGE ( 'NONE', *, *, #33156, .F. ) ;
#15254 = LINE ( 'NONE', #21150, #37659 ) ;
#15255 = EDGE_CURVE ( 'NONE', #8245, #31622, #5538, .T. ) ;
#15256 = CARTESIAN_POINT ( 'NONE',  ( 6.199999999999997513, 6.971071669133949438E-15, 0.000000000000000000 ) ) ;
#15257 = ORIENTED_EDGE ( 'NONE', *, *, #19674, .F. ) ;
#15258 = DIRECTION ( 'NONE',  ( -1.000000000000000000, -0.000000000000000000, -0.000000000000000000 ) ) ;
#15259 = DIRECTION ( 'NONE',  ( 0.000000000000000000, 0.000000000000000000, 1.000000000000000000 ) ) ;
#15260 = ADVANCED_FACE ( 'NONE', ( #41958 ), #25220, .F. ) ;
#15262 = CARTESIAN_POINT ( 'NONE',  ( 0.000000000000000000, 0.000000000000000000, 0.000000000000000000 ) ) ;
#15261 = CARTESIAN_POINT ( 'NONE',  ( -6.473970235329672780E-16, -4.862606272033106691, -3.745885042887442395 ) ) ;
#15263 = EDGE_LOOP ( 'NONE', ( #9922, #10584, #17554, #18731 ) ) ;
#15264 = DIRECTION ( 'NONE',  ( 1.000000000000000000, 0.000000000000000000, 0.000000000000000000 ) ) ;
#15265 = ORIENTED_EDGE ( 'NONE', *, *, #24391, .T. ) ;
#15266 = DIRECTION ( 'NONE',  ( 1.000000000000000000, -1.373900992973642263E-15, 0.000000000000000000 ) ) ;
#15267 = CARTESIAN_POINT ( 'NONE',  ( 32.80084743084300669, 40.00000000000000000, 19.01436317119532760 ) ) ;
#15268 = CARTESIAN_POINT ( 'NONE',  ( 18.00000000000000355, 0.000000000000000000, 0.000000000000000000 ) ) ;
#15269 = ADVANCED_FACE ( 'NONE', ( #4890 ), #34784, .F. ) ;
#15270 = AXIS2_PLACEMENT_3D ( 'NONE', #34248, #20778, #14204 ) ;
#15271 = VECTOR ( 'NONE', #17003, 1000.000000000000000 ) ;
#15272 = CARTESIAN_POINT ( 'NONE',  ( 0.000000000000000000, -51.93417535146743802, 2.615612846549014492 ) ) ;
#15273 = DIRECTION ( 'NONE',  ( -1.000000000000000000, -0.000000000000000000, -0.000000000000000000 ) ) ;
#15274 = ORIENTED_EDGE ( 'NONE', *, *, #2420, .T. ) ;
#15275 = TOROIDAL_SURFACE ( 'NONE', #21543, 19.11697999999999809, 0.08401999999999801294 ) ;
#15276 = DIRECTION ( 'NONE',  ( -1.000000000000000000, -0.000000000000000000, 0.000000000000000000 ) ) ;
#15277 = ORIENTED_EDGE ( 'NONE', *, *, #32217, .T. ) ;
#15278 = CIRCLE ( 'NONE', #28501, 129.9999999999993463 ) ;
#15279 = CYLINDRICAL_SURFACE ( 'NONE', #8532, 116.0000000000000000 ) ;
#15280 = CARTESIAN_POINT ( 'NONE',  ( 2.649999999999993694, 150.5000000000000284, 9.999999999999998224 ) ) ;
#15281 = CARTESIAN_POINT ( 'NONE',  ( 18.38119342899891961, 31.00000000000000355, 31.81670425098764099 ) ) ;
#15282 = VERTEX_POINT ( 'NONE', #2441 ) ;
#15283 = DIRECTION ( 'NONE',  ( 3.009274222672345096E-17, 1.000000000000000000, -2.455023325076454960E-18 ) ) ;
#15284 = CARTESIAN_POINT ( 'NONE',  ( -21.28946418274055929, 31.00000000000000355, -79.45670318283352174 ) ) ;
#15285 = ORIENTED_EDGE ( 'NONE', *, *, #12667, .T. ) ;
#15286 = CARTESIAN_POINT ( 'NONE',  ( -51.85848278221650531, 31.00000000000000355, -6.921372802086644072 ) ) ;
#15287 = CARTESIAN_POINT ( 'NONE',  ( -40.67465422008825726, 40.00000000000000000, -82.48404079236435393 ) ) ;
#15288 = ORIENTED_EDGE ( 'NONE', *, *, #24169, .F. ) ;
#15289 = CARTESIAN_POINT ( 'NONE',  ( 0.000000000000000000, -51.98489025774233596, -108.7109110710166391 ) ) ;
#15290 = DIRECTION ( 'NONE',  ( 0.000000000000000000, 0.000000000000000000, 1.000000000000000000 ) ) ;
#15291 = CARTESIAN_POINT ( 'NONE',  ( 18.00000000000000355, 0.000000000000000000, 0.000000000000000000 ) ) ;
#15292 = CIRCLE ( 'NONE', #3357, 59.00000000000000711 ) ;
#15293 = AXIS2_PLACEMENT_3D ( 'NONE', #43089, #19790, #13453 ) ;
#15295 = ORIENTED_EDGE ( 'NONE', *, *, #37195, .F. ) ;
#15294 = CARTESIAN_POINT ( 'NONE',  ( 17.99999999999999645, 52.19040376560566585, -99.31985817764127944 ) ) ;
#15296 = EDGE_CURVE ( 'NONE', #1993, #3154, #12418, .T. ) ;
#15297 = FACE_OUTER_BOUND ( 'NONE', #27201, .T. ) ;
#15298 = LINE ( 'NONE', #37720, #7671 ) ;
#15299 = AXIS2_PLACEMENT_3D ( 'NONE', #31309, #7730, #31729 ) ;
#15300 = ADVANCED_FACE ( 'NONE', ( #31517 ), #31727, .T. ) ;
#15301 = ORIENTED_EDGE ( 'NONE', *, *, #1105, .T. ) ;
#15302 = CARTESIAN_POINT ( 'NONE',  ( -54.82550897924149069, 40.00000000000000711, 42.06954809655981364 ) ) ;
#15303 = CARTESIAN_POINT ( 'NONE',  ( 0.000000000000000000, 0.000000000000000000, 0.000000000000000000 ) ) ;
#15304 = ORIENTED_EDGE ( 'NONE', *, *, #27639, .F. ) ;
#15305 = DIRECTION ( 'NONE',  ( -1.000000000000000000, -0.000000000000000000, -0.000000000000000000 ) ) ;
#15306 = DIRECTION ( 'NONE',  ( -0.06345332152672161774, 1.058048417131579272E-15, 0.9979848074931934043 ) ) ;
#15307 = DIRECTION ( 'NONE',  ( -1.000000000000000000, 0.000000000000000000, 0.000000000000000000 ) ) ;
#15308 = ORIENTED_EDGE ( 'NONE', *, *, #36929, .F. ) ;
#15309 = EDGE_CURVE ( 'NONE', #29305, #9725, #17358, .T. ) ;
#15310 = ORIENTED_EDGE ( 'NONE', *, *, #28357, .F. ) ;
#15311 = LINE ( 'NONE', #39659, #17753 ) ;
#15312 = ORIENTED_EDGE ( 'NONE', *, *, #10733, .T. ) ;
#15313 = DIRECTION ( 'NONE',  ( 0.000000000000000000, -1.000000000000000000, 1.287488025362403787E-15 ) ) ;
#15314 = DIRECTION ( 'NONE',  ( 0.000000000000000000, 0.000000000000000000, 1.000000000000000000 ) ) ;
#15315 = EDGE_CURVE ( 'NONE', #9874, #30346, #41694, .T. ) ;
#15316 = DIRECTION ( 'NONE',  ( 0.000000000000000000, 0.5000000000000009992, 0.8660254037844380415 ) ) ;
#15317 = DIRECTION ( 'NONE',  ( 0.000000000000000000, -1.000000000000000000, 0.000000000000000000 ) ) ;
#15318 = EDGE_LOOP ( 'NONE', ( #29441, #39256, #28160, #17224 ) ) ;
#15319 = FACE_OUTER_BOUND ( 'NONE', #28205, .T. ) ;
#15320 = DIRECTION ( 'NONE',  ( 0.000000000000000000, 0.6845471059286899473, -0.7289686274214103312 ) ) ;
#15321 = EDGE_LOOP ( 'NONE', ( #7474, #38475, #12728, #13473 ) ) ;
#15322 = CARTESIAN_POINT ( 'NONE',  ( 17.99999999999999645, 28.62203781743003717, 14.19692359621465094 ) ) ;
#15323 = DIRECTION ( 'NONE',  ( -1.000000000000000000, -0.000000000000000000, -0.000000000000000000 ) ) ;
#15324 = AXIS2_PLACEMENT_3D ( 'NONE', #895, #38214, #8330 ) ;
#15325 = EDGE_CURVE ( 'NONE', #24215, #7262, #568, .T. ) ;
#15326 = FACE_OUTER_BOUND ( 'NONE', #40059, .T. ) ;
#15327 = CARTESIAN_POINT ( 'NONE',  ( -6.238242335983215092, 31.00000000000000355, 47.40213128959678102 ) ) ;
#15328 = EDGE_CURVE ( 'NONE', #3009, #32816, #35403, .T. ) ;
#15329 = ORIENTED_EDGE ( 'NONE', *, *, #12485, .T. ) ;
#15331 = DIRECTION ( 'NONE',  ( -1.000000000000000000, -0.000000000000000000, 0.000000000000000000 ) ) ;
#15330 = CARTESIAN_POINT ( 'NONE',  ( 17.99999999999999645, 0.000000000000000000, 0.000000000000000000 ) ) ;
#15332 = EDGE_CURVE ( 'NONE', #7188, #24964, #13858, .T. ) ;
#15333 = EDGE_LOOP ( 'NONE', ( #21053, #43023 ) ) ;
#15334 = CARTESIAN_POINT ( 'NONE',  ( 42.30435120181500963, 40.00000000000000000, 37.09784777058769123 ) ) ;
#15335 = CARTESIAN_POINT ( 'NONE',  ( 17.99999999999999645, 46.83041522348636931, -101.9567785075596618 ) ) ;
#15336 = DIRECTION ( 'NONE',  ( -1.807003620809174878E-16, 1.000000000000000000, 0.000000000000000000 ) ) ;
#15337 = CARTESIAN_POINT ( 'NONE',  ( -158.5000000000000284, 1.941065176648555254E-14, 9.999999999999998224 ) ) ;
#15338 = CARTESIAN_POINT ( 'NONE',  ( 153.1500000000000057, 1.576403824487674918E-12, 6.999999999999998224 ) ) ;
#15339 = EDGE_CURVE ( 'NONE', #25565, #12306, #20855, .T. ) ;
#15340 = ORIENTED_EDGE ( 'NONE', *, *, #24773, .F. ) ;
#15341 = CARTESIAN_POINT ( 'NONE',  ( -19.20510714644778361, 40.00000000000000000, 33.27066566623395261 ) ) ;
#15342 = EDGE_LOOP ( 'NONE', ( #35374, #39061, #30187, #35800 ) ) ;
#15343 = CARTESIAN_POINT ( 'NONE',  ( 0.000000000000000000, -97.19627249181141337, 71.22763238166453448 ) ) ;
#15344 = DIRECTION ( 'NONE',  ( 1.000000000000000000, -0.000000000000000000, 0.000000000000000000 ) ) ;
#15345 = EDGE_LOOP ( 'NONE', ( #17907, #40789, #40434, #18003 ) ) ;
#15346 = AXIS2_PLACEMENT_3D ( 'NONE', #14259, #37578, #1783 ) ;
#15347 = CARTESIAN_POINT ( 'NONE',  ( 0.000000000000000000, 80.74349901498510462, -77.90224541347200216 ) ) ;
#15348 = ORIENTED_EDGE ( 'NONE', *, *, #39810, .F. ) ;
#15349 = DIRECTION ( 'NONE',  ( 0.000000000000000000, 0.000000000000000000, -1.000000000000000000 ) ) ;
#15350 = VERTEX_POINT ( 'NONE', #26044 ) ;
#15351 = EDGE_CURVE ( 'NONE', #20442, #28617, #42366, .T. ) ;
#15352 = VERTEX_POINT ( 'NONE', #22580 ) ;
#15353 = APPLICATION_CONTEXT ( 'automotive_design' ) ;
#15354 = CARTESIAN_POINT ( 'NONE',  ( 0.000000000000000000, -87.92975456462950490, 69.68953103478128241 ) ) ;
#15355 = CARTESIAN_POINT ( 'NONE',  ( -35.65230965298280097, 31.00000000000000355, 72.05959145978816593 ) ) ;
#15356 = EDGE_CURVE ( 'NONE', #37256, #39961, #37521, .T. ) ;
#15357 = VERTEX_POINT ( 'NONE', #9441 ) ;
#15358 = DIRECTION ( 'NONE',  ( -1.000000000000000000, -0.000000000000000000, -0.000000000000000000 ) ) ;
#15359 = LINE ( 'NONE', #35164, #35174 ) ;
#15360 = ORIENTED_EDGE ( 'NONE', *, *, #5238, .T. ) ;
#15361 = CARTESIAN_POINT ( 'NONE',  ( 0.000000000000000000, 0.000000000000000000, 0.000000000000000000 ) ) ;
#15362 = DIRECTION ( 'NONE',  ( 0.000000000000000000, 0.1062934856473656403, -0.9943348002101370930 ) ) ;
#15363 = CARTESIAN_POINT ( 'NONE',  ( 26.62151981922249533, 31.00000000000000355, -3.482817046706074393 ) ) ;
#15365 = CARTESIAN_POINT ( 'NONE',  ( 17.99999999999999645, 0.000000000000000000, 0.000000000000000000 ) ) ;
#15364 = DIRECTION ( 'NONE',  ( -1.000000000000000000, -0.000000000000000000, -0.000000000000000000 ) ) ;
#15366 = CARTESIAN_POINT ( 'NONE',  ( 0.000000000000000000, -75.03166794516737070, -94.29071961951585479 ) ) ;
#15367 = DIRECTION ( 'NONE',  ( -1.000000000000000000, -0.000000000000000000, -0.000000000000000000 ) ) ;
#15368 = ORIENTED_EDGE ( 'NONE', *, *, #10818, .T. ) ;
#15369 = SURFACE_STYLE_USAGE ( .BOTH. , #5302 ) ;
#15370 = FACE_OUTER_BOUND ( 'NONE', #31778, .T. ) ;
#15371 = AXIS2_PLACEMENT_3D ( 'NONE', #24461, #6168, #19516 ) ;
#15372 = ORIENTED_EDGE ( 'NONE', *, *, #11420, .T. ) ;
#15373 = DIRECTION ( 'NONE',  ( -1.000000000000000000, -0.000000000000000000, 0.000000000000000000 ) ) ;
#15374 = AXIS2_PLACEMENT_3D ( 'NONE', #25265, #27880, #21989 ) ;
#15375 = CARTESIAN_POINT ( 'NONE',  ( 29.96647033545507455, 31.00000000000000355, -88.27250603610892199 ) ) ;
#15377 = EDGE_CURVE ( 'NONE', #4507, #29613, #34724, .T. ) ;
#15376 = CIRCLE ( 'NONE', #19542, 116.0000000000000000 ) ;
#15378 = CARTESIAN_POINT ( 'NONE',  ( 33.40854556226729954, -34.05525454449573175, -74.83297477053802993 ) ) ;
#15379 = EDGE_LOOP ( 'NONE', ( #33448, #3202, #831 ) ) ;
#15380 = PRODUCT_DEFINITION ( 'UNKNOWN', '', #31662, #22078 ) ;
#15381 = CIRCLE ( 'NONE', #13278, 120.5010000000000190 ) ;
#15382 = CARTESIAN_POINT ( 'NONE',  ( 32.71557229150619861, 40.00000000000000000, -11.11602612089219910 ) ) ;
#15383 = CARTESIAN_POINT ( 'NONE',  ( -41.89947471387619515, 40.00000000000000000, 2.670153906482984230 ) ) ;
#15384 = ORIENTED_EDGE ( 'NONE', *, *, #36187, .T. ) ;
#15385 = EDGE_LOOP ( 'NONE', ( #16983, #4363, #15146, #22943 ) ) ;
#15386 = CARTESIAN_POINT ( 'NONE',  ( -10.00000000000000000, 0.000000000000000000, 51.99999999999999289 ) ) ;
#15387 = CARTESIAN_POINT ( 'NONE',  ( 0.000000000000000000, -16.77727049691090500, -27.19001440037564166 ) ) ;
#15388 = FACE_OUTER_BOUND ( 'NONE', #27604, .T. ) ;
#15389 = CARTESIAN_POINT ( 'NONE',  ( -3.349226789952655547, -2.685125164760744809, -0.2236248678334863682 ) ) ;
#15390 = EDGE_CURVE ( 'NONE', #239, #24680, #15278, .T. ) ;
#15391 = DIRECTION ( 'NONE',  ( 0.000000000000000000, 0.7525707698561396874, -0.6585113790650372056 ) ) ;
#15392 = ORIENTED_EDGE ( 'NONE', *, *, #26345, .F. ) ;
#15393 = DIRECTION ( 'NONE',  ( 0.000000000000000000, -0.1837495178165775567, 0.9829730996839004531 ) ) ;
#15394 = VERTEX_POINT ( 'NONE', #23428 ) ;
#15395 = CARTESIAN_POINT ( 'NONE',  ( 0.000000000000000000, 103.4151313792870610, 61.85306461934443689 ) ) ;
#15396 = CYLINDRICAL_SURFACE ( 'NONE', #15178, 59.00000000000000000 ) ;
#15397 = AXIS2_PLACEMENT_3D ( 'NONE', #14222, #24052, #24499 ) ;
#15398 = DIRECTION ( 'NONE',  ( -1.000000000000000000, -0.000000000000000000, 0.000000000000000000 ) ) ;
#15399 = CYLINDRICAL_SURFACE ( 'NONE', #8752, 20.00000000000000711 ) ;
#15400 = ORIENTED_EDGE ( 'NONE', *, *, #42719, .T. ) ;
#15401 = ORIENTED_EDGE ( 'NONE', *, *, #20323, .T. ) ;
#15402 = AXIS2_PLACEMENT_3D ( 'NONE', #25509, #15896, #42888 ) ;
#15403 = DIRECTION ( 'NONE',  ( 0.000000000000000000, 0.9407002666710342353, -0.3392388661180278930 ) ) ;
#15404 = EDGE_CURVE ( 'NONE', #32412, #3192, #29750, .T. ) ;
#15405 = AXIS2_PLACEMENT_3D ( 'NONE', #27193, #16748, #3795 ) ;
#15406 = ORIENTED_EDGE ( 'NONE', *, *, #32896, .T. ) ;
#15408 = ORIENTED_EDGE ( 'NONE', *, *, #41049, .F. ) ;
#15407 = DIRECTION ( 'NONE',  ( 1.000000000000000000, 0.000000000000000000, -0.000000000000000000 ) ) ;
#15409 = CARTESIAN_POINT ( 'NONE',  ( -51.85848278221650531, 31.00000000000000355, -6.921372802086644072 ) ) ;
#15410 = EDGE_CURVE ( 'NONE', #16222, #10174, #27775, .T. ) ;
#15412 = ORIENTED_EDGE ( 'NONE', *, *, #2004, .F. ) ;
#15411 = CIRCLE ( 'NONE', #10477, 58.99999999999999289 ) ;
#15413 = CARTESIAN_POINT ( 'NONE',  ( 17.99999999999999645, 0.000000000000000000, 0.000000000000000000 ) ) ;
#15414 = VECTOR ( 'NONE', #24253, 1000.000000000000000 ) ;
#15415 = CARTESIAN_POINT ( 'NONE',  ( 4.211140560182196957, 2.431303136016536470, -3.745885042887433514 ) ) ;
#15416 = ORIENTED_EDGE ( 'NONE', *, *, #25200, .T. ) ;
#15417 = CARTESIAN_POINT ( 'NONE',  ( 33.43413415811954792, 40.00000000000000000, -67.56680175473154293 ) ) ;
#15418 = CARTESIAN_POINT ( 'NONE',  ( 17.99999999999999645, 0.000000000000000000, 0.000000000000000000 ) ) ;
#15419 = CARTESIAN_POINT ( 'NONE',  ( 17.99999999999999645, -34.74871106919551522, -106.6808302961375148 ) ) ;
#15420 = ORIENTED_EDGE ( 'NONE', *, *, #37480, .F. ) ;
#15421 = CARTESIAN_POINT ( 'NONE',  ( 17.99999999999999645, -115.6826031496111398, -8.575274253898639287 ) ) ;
#15422 = VERTEX_POINT ( 'NONE', #12531 ) ;
#15423 = DIRECTION ( 'NONE',  ( 1.000000000000000000, 0.000000000000000000, 0.000000000000000000 ) ) ;
#15424 = LINE ( 'NONE', #1423, #2491 ) ;
#15425 = EDGE_CURVE ( 'NONE', #9420, #20431, #29968, .T. ) ;
#15426 = CIRCLE ( 'NONE', #9804, 59.00000000000000000 ) ;
#15427 = CARTESIAN_POINT ( 'NONE',  ( 52.51402048354923835, 31.00000000000000355, 40.27907379435107060 ) ) ;
#15428 = EDGE_CURVE ( 'NONE', #39201, #20639, #12449, .T. ) ;
#15429 = LINE ( 'NONE', #26717, #6508 ) ;
#15430 = VERTEX_POINT ( 'NONE', #36689 ) ;
#15431 = ADVANCED_FACE ( 'NONE', ( #6587 ), #26683, .T. ) ;
#15432 = EDGE_CURVE ( 'NONE', #29484, #42037, #4049, .T. ) ;
#15433 = CIRCLE ( 'NONE', #23800, 2.041999999999999815 ) ;
#15434 = CYLINDRICAL_SURFACE ( 'NONE', #16369, 59.00000000000000000 ) ;
#15435 = AXIS2_PLACEMENT_3D ( 'NONE', #38486, #4912, #11701 ) ;
#15436 = AXIS2_PLACEMENT_3D ( 'NONE', #25441, #12757, #12121 ) ;
#15437 = ORIENTED_EDGE ( 'NONE', *, *, #9828, .F. ) ;
#15438 = DIRECTION ( 'NONE',  ( 0.000000000000000000, 0.000000000000000000, 1.000000000000000000 ) ) ;
#15439 = DIRECTION ( 'NONE',  ( -1.000000000000000000, -0.000000000000000000, -0.000000000000000000 ) ) ;
#15440 = CARTESIAN_POINT ( 'NONE',  ( 68.41293481155882716, 31.00000000000000000, -52.34142988146868447 ) ) ;
#15441 = CARTESIAN_POINT ( 'NONE',  ( 52.26791824981292933, 40.00000000000000000, -67.94187691988643962 ) ) ;
#15442 = VECTOR ( 'NONE', #23761, 1000.000000000000000 ) ;
#15443 = DIRECTION ( 'NONE',  ( 1.000000000000000000, 0.000000000000000000, 0.000000000000000000 ) ) ;
#15444 = ORIENTED_EDGE ( 'NONE', *, *, #27157, .T. ) ;
#15445 = CARTESIAN_POINT ( 'NONE',  ( 5.639656061357294803, -10.48075544252183100, -1.199999999999999956 ) ) ;
#15446 = ORIENTED_EDGE ( 'NONE', *, *, #13219, .F. ) ;
#15447 = CIRCLE ( 'NONE', #18265, 13.59999999999999964 ) ;
#15448 = DIRECTION ( 'NONE',  ( 0.000000000000000000, 0.4610925014493266194, -0.8873520750565710991 ) ) ;
#15450 = ORIENTED_EDGE ( 'NONE', *, *, #39763, .F. ) ;
#15449 = CARTESIAN_POINT ( 'NONE',  ( 17.99999999999999645, 17.33727698085324320, -110.8498592715971967 ) ) ;
#15451 = DIRECTION ( 'NONE',  ( -1.000000000000000000, 0.000000000000000000, -0.000000000000000000 ) ) ;
#15452 = ORIENTED_EDGE ( 'NONE', *, *, #15937, .T. ) ;
#15453 = CARTESIAN_POINT ( 'NONE',  ( 17.99999999999999645, 31.81777574834302058, 2.898764365605871696 ) ) ;
#15454 = CARTESIAN_POINT ( 'NONE',  ( -135.4416936590755540, -2.055254544495720648, -102.7350398871816424 ) ) ;
#15455 = FACE_OUTER_BOUND ( 'NONE', #23729, .T. ) ;
#15456 = ORIENTED_EDGE ( 'NONE', *, *, #37195, .T. ) ;
#15457 = DIRECTION ( 'NONE',  ( 1.000000000000000000, 0.000000000000000000, 0.000000000000000000 ) ) ;
#15458 = CARTESIAN_POINT ( 'NONE',  ( 17.99999999999999645, -105.3681574666266414, 38.54638589714855357 ) ) ;
#15459 = CIRCLE ( 'NONE', #21050, 59.00000000000000000 ) ;
#15461 = CARTESIAN_POINT ( 'NONE',  ( 17.99999999999999645, -11.41303419184897017, -111.6154788735837116 ) ) ;
#15460 = DIRECTION ( 'NONE',  ( 0.000000000000000000, 0.000000000000000000, 1.000000000000000000 ) ) ;
#15462 = EDGE_LOOP ( 'NONE', ( #35155, #13418, #7472, #10528 ) ) ;
#15463 = CARTESIAN_POINT ( 'NONE',  ( 17.99999999999999645, -100.6739960869721102, 49.52796165323228195 ) ) ;
#15464 = CIRCLE ( 'NONE', #38427, 13.59999999999999964 ) ;
#15465 = FACE_OUTER_BOUND ( 'NONE', #31433, .T. ) ;
#15466 = CARTESIAN_POINT ( 'NONE',  ( -28.59133019391067165, 40.00000000000000000, -32.71076623427350683 ) ) ;
#15467 = CARTESIAN_POINT ( 'NONE',  ( 17.99999999999999645, 84.77518783075095143, 73.49448960231384831 ) ) ;
#15468 = CIRCLE ( 'NONE', #5676, 120.5010000000000190 ) ;
#15469 = DIRECTION ( 'NONE',  ( -1.000000000000000000, -0.000000000000000000, -0.000000000000000000 ) ) ;
#15470 = VECTOR ( 'NONE', #9078, 1000.000000000000000 ) ;
#15471 = LINE ( 'NONE', #5405, #17223 ) ;
#15472 = ORIENTED_EDGE ( 'NONE', *, *, #10444, .F. ) ;
#15473 = CARTESIAN_POINT ( 'NONE',  ( 0.000000000000000000, -97.97378550988267421, 62.10585602713726416 ) ) ;
#15474 = ORIENTED_EDGE ( 'NONE', *, *, #37560, .F. ) ;
#15475 = AXIS2_PLACEMENT_3D ( 'NONE', #2470, #29554, #16257 ) ;
#15476 = CARTESIAN_POINT ( 'NONE',  ( 17.99999999999999645, 29.02167576844106023, 108.3790330702170621 ) ) ;
#15477 = CARTESIAN_POINT ( 'NONE',  ( 9.000000000000001776, 47.31079789947484926, 105.9135893174952656 ) ) ;
#15478 = CARTESIAN_POINT ( 'NONE',  ( -39.53383601736616271, 31.00000000000000355, 5.215339288884301538 ) ) ;
#15479 = VERTEX_POINT ( 'NONE', #25845 ) ;
#15480 = FACE_OUTER_BOUND ( 'NONE', #7789, .T. ) ;
#15481 = ORIENTED_EDGE ( 'NONE', *, *, #19048, .F. ) ;
#15482 = ADVANCED_FACE ( 'NONE', ( #3304 ), #12954, .T. ) ;
#15483 = EDGE_CURVE ( 'NONE', #20704, #27145, #9232, .T. ) ;
#15484 = ITEM_DEFINED_TRANSFORMATION ( 'NONE', 'NONE', #38586,  #13552 ) ;
#15485 = EDGE_CURVE ( 'NONE', #6578, #36284, #36260, .T. ) ;
#15486 = LINE ( 'NONE', #28362, #29570 ) ;
#15487 = CARTESIAN_POINT ( 'NONE',  ( -40.67465422008825726, 31.00000000000000355, -82.48404079236435393 ) ) ;
#15488 = ORIENTED_EDGE ( 'NONE', *, *, #25061, .F. ) ;
#15489 = CARTESIAN_POINT ( 'NONE',  ( -49.80813925210023996, 31.00000000000000355, -17.00652635548579994 ) ) ;
#15490 = CARTESIAN_POINT ( 'NONE',  ( 84.24376206367318787, 39.99999999999999289, -11.10575268747775901 ) ) ;
#15491 = ORIENTED_EDGE ( 'NONE', *, *, #15687, .F. ) ;
#15492 = AXIS2_PLACEMENT_3D ( 'NONE', #12658, #22944, #15518 ) ;
#15493 = DIRECTION ( 'NONE',  ( 0.000000000000000000, 0.000000000000000000, 1.000000000000000000 ) ) ;
#15494 = EDGE_CURVE ( 'NONE', #37143, #17989, #12962, .T. ) ;
#15495 = DIRECTION ( 'NONE',  ( 0.000000000000000000, 0.000000000000000000, 1.000000000000000000 ) ) ;
#15496 = CARTESIAN_POINT ( 'NONE',  ( 0.000000000000000000, -46.77034588191289544, -22.72740077717278595 ) ) ;
#15497 = CIRCLE ( 'NONE', #27308, 52.00000000000000000 ) ;
#15499 = EDGE_LOOP ( 'NONE', ( #19665, #24039, #15709, #32495 ) ) ;
#15498 = LINE ( 'NONE', #25121, #27214 ) ;
#15500 = CARTESIAN_POINT ( 'NONE',  ( 0.000000000000000000, 104.2166695095712470, 60.49278301857841456 ) ) ;
#15501 = LINE ( 'NONE', #15924, #34208 ) ;
#15502 = ORIENTED_EDGE ( 'NONE', *, *, #42715, .F. ) ;
#15503 = CARTESIAN_POINT ( 'NONE',  ( -21.91107887650263564, 40.00000000000000000, 64.54935342160338507 ) ) ;
#15504 = CYLINDRICAL_SURFACE ( 'NONE', #20847, 59.00000000000000000 ) ;
#15505 = AXIS2_PLACEMENT_3D ( 'NONE', #27522, #10711, #10498 ) ;
#15506 = ORIENTED_EDGE ( 'NONE', *, *, #5147, .F. ) ;
#15507 = LINE ( 'NONE', #28801, #14118 ) ;
#15508 = ORIENTED_EDGE ( 'NONE', *, *, #21505, .F. ) ;
#15509 = EDGE_CURVE ( 'NONE', #5216, #33264, #22223, .T. ) ;
#15510 = ORIENTED_EDGE ( 'NONE', *, *, #26099, .T. ) ;
#15511 = LINE ( 'NONE', #42071, #10040 ) ;
#15512 = ORIENTED_EDGE ( 'NONE', *, *, #27711, .T. ) ;
#15513 = DIRECTION ( 'NONE',  ( 1.000000000000000000, 0.000000000000000000, 0.000000000000000000 ) ) ;
#15514 = CARTESIAN_POINT ( 'NONE',  ( 8.999999999999998224, -82.63181128086679905, -81.41243003647058174 ) ) ;
#15515 = CARTESIAN_POINT ( 'NONE',  ( 150.5000000000000284, 1.576403824487674918E-12, 6.999999999999998224 ) ) ;
#15516 = CARTESIAN_POINT ( 'NONE',  ( 18.00000000000000355, -46.11014828289851408, 9.022736828080542892 ) ) ;
#15517 = EDGE_LOOP ( 'NONE', ( #21894, #7242 ) ) ;
#15518 = DIRECTION ( 'NONE',  ( -1.836909530733573776E-16, 1.000000000000000000, 0.000000000000000000 ) ) ;
#15519 = ORIENTED_EDGE ( 'NONE', *, *, #33016, .F. ) ;
#15520 = CIRCLE ( 'NONE', #24590, 18.77999999999999048 ) ;
#15521 = AXIS2_PLACEMENT_3D ( 'NONE', #27328, #889, #4382 ) ;
#15522 = CARTESIAN_POINT ( 'NONE',  ( 0.000000000000000000, 34.78944633786279184, 9.257128253673750251 ) ) ;
#15523 = VERTEX_POINT ( 'NONE', #36704 ) ;
#15524 = DIRECTION ( 'NONE',  ( -1.000000000000000000, 0.000000000000000000, 0.000000000000000000 ) ) ;
#15525 = AXIS2_PLACEMENT_3D ( 'NONE', #9987, #32481, #19010 ) ;
#15526 = EDGE_CURVE ( 'NONE', #34978, #13537, #39542, .T. ) ;
#15527 = CARTESIAN_POINT ( 'NONE',  ( 0.000000000000000000, 0.000000000000000000, 0.000000000000000000 ) ) ;
#15528 = SHAPE_DEFINITION_REPRESENTATION ( #6760, #7878 ) ;
#15529 = DIRECTION ( 'NONE',  ( 0.000000000000000000, 0.000000000000000000, -1.000000000000000000 ) ) ;
#15530 = CARTESIAN_POINT ( 'NONE',  ( 20.73284993368543638, 31.00000000000000355, 42.03655757353646294 ) ) ;
#15531 = CIRCLE ( 'NONE', #21123, 59.00000000000000000 ) ;
#15532 = VERTEX_POINT ( 'NONE', #6180 ) ;
#15533 = DIRECTION ( 'NONE',  ( 0.000000000000000000, -0.7980172272802448230, 0.6026346363792494110 ) ) ;
#15534 = ORIENTED_EDGE ( 'NONE', *, *, #28712, .F. ) ;
#15535 = ADVANCED_FACE ( 'NONE', ( #29760 ), #26479, .T. ) ;
#15536 = CARTESIAN_POINT ( 'NONE',  ( 48.10206620145878276, 40.00000000000000000, -42.20136231105875879 ) ) ;
#15537 = ADVANCED_FACE ( 'NONE', ( #26907 ), #240, .T. ) ;
#15538 = FACE_OUTER_BOUND ( 'NONE', #5992, .T. ) ;
#15539 = EDGE_CURVE ( 'NONE', #29797, #13292, #14539, .T. ) ;
#15540 = DIRECTION ( 'NONE',  ( 0.000000000000000000, 0.8183027759081662467, 0.5747874102144109321 ) ) ;
#15541 = LINE ( 'NONE', #5892, #29505 ) ;
#15542 = FACE_OUTER_BOUND ( 'NONE', #16873, .T. ) ;
#15543 = AXIS2_PLACEMENT_3D ( 'NONE', #19397, #32665, #16313 ) ;
#15544 = ORIENTED_EDGE ( 'NONE', *, *, #26558, .T. ) ;
#15545 = CARTESIAN_POINT ( 'NONE',  ( 26.99674208481366833, 40.00000000000000000, -20.71990538090019029 ) ) ;
#15546 = ORIENTED_EDGE ( 'NONE', *, *, #28532, .T. ) ;
#15547 = DIRECTION ( 'NONE',  ( 0.000000000000000000, 0.000000000000000000, 1.000000000000000000 ) ) ;
#15548 = CARTESIAN_POINT ( 'NONE',  ( 17.99999999999999645, 0.000000000000000000, 0.000000000000000000 ) ) ;
#15549 = EDGE_LOOP ( 'NONE', ( #4957, #9077, #42495, #8442 ) ) ;
#15550 = DIRECTION ( 'NONE',  ( 1.000000000000000000, -0.000000000000000000, -0.000000000000000000 ) ) ;
#15551 = VECTOR ( 'NONE', #40298, 1000.000000000000000 ) ;
#15552 = VERTEX_POINT ( 'NONE', #43035 ) ;
#15553 = DIRECTION ( 'NONE',  ( 1.000000000000000000, 0.000000000000000000, 0.000000000000000000 ) ) ;
#15554 = ORIENTED_EDGE ( 'NONE', *, *, #36160, .F. ) ;
#15555 = ADVANCED_FACE ( 'NONE', ( #13613 ), #39748, .T. ) ;
#15556 = ORIENTED_EDGE ( 'NONE', *, *, #19844, .T. ) ;
#15557 = DIRECTION ( 'NONE',  ( 1.000000000000000000, -3.035766082959410566E-17, 0.000000000000000000 ) ) ;
#15558 = CARTESIAN_POINT ( 'NONE',  ( -10.92011822083620309, 31.00000000000000355, -83.75917815547792600 ) ) ;
#15559 = ORIENTED_EDGE ( 'NONE', *, *, #39262, .T. ) ;
#15560 = CARTESIAN_POINT ( 'NONE',  ( 17.99999999999999645, 31.80866420683990725, 2.997093558041416195 ) ) ;
#15561 = DIRECTION ( 'NONE',  ( -1.000000000000000000, -0.000000000000000000, 0.000000000000000000 ) ) ;
#15562 = ORIENTED_EDGE ( 'NONE', *, *, #15717, .T. ) ;
#15563 = CARTESIAN_POINT ( 'NONE',  ( 18.00000000000000355, 27.79676263918241119, -37.88001506494740056 ) ) ;
#15564 = PRODUCT_DEFINITION_SHAPE ( 'NONE', 'NONE',  #43210 ) ;
#15565 = DIRECTION ( 'NONE',  ( 0.000000000000000000, -0.7164567402983210709, 0.6976315211349786161 ) ) ;
#15566 = CARTESIAN_POINT ( 'NONE',  ( -76.05825820879898913, 40.00000000000000711, 66.55365856249082412 ) ) ;
#15568 = DIRECTION ( 'NONE',  ( 1.000000000000000000, -1.373900992973642263E-15, -4.525365589504737954E-16 ) ) ;
#15567 = DIRECTION ( 'NONE',  ( -1.000000000000000000, 0.000000000000000000, 0.000000000000000000 ) ) ;
#15569 = DIRECTION ( 'NONE',  ( 1.000000000000000000, 0.000000000000000000, 0.000000000000000000 ) ) ;
#15570 = DIRECTION ( 'NONE',  ( -1.000000000000000000, 0.000000000000000000, -0.000000000000000000 ) ) ;
#15571 = ADVANCED_FACE ( 'NONE', ( #40183 ), #19525, .F. ) ;
#15572 = ORIENTED_EDGE ( 'NONE', *, *, #18574, .F. ) ;
#15573 =( NAMED_UNIT ( * ) SI_UNIT ( $, .STERADIAN. ) SOLID_ANGLE_UNIT ( ) );
#15574 = AXIS2_PLACEMENT_3D ( 'NONE', #7761, #4472, #1209 ) ;
#15575 = CYLINDRICAL_SURFACE ( 'NONE', #40803, 59.00000000000000000 ) ;
#15576 = VERTEX_POINT ( 'NONE', #6595 ) ;
#15577 = CYLINDRICAL_SURFACE ( 'NONE', #27561, 116.0000000000000000 ) ;
#15578 = LINE ( 'NONE', #5309, #28674 ) ;
#15579 = ORIENTED_EDGE ( 'NONE', *, *, #18893, .T. ) ;
#15580 = CARTESIAN_POINT ( 'NONE',  ( 11.86982580658625075, 40.00000000000000000, 24.05989836594520526 ) ) ;
#15581 = CARTESIAN_POINT ( 'NONE',  ( -24.78443185004241656, 40.00000000000000000, 32.19086620116434005 ) ) ;
#15582 = EDGE_CURVE ( 'NONE', #41485, #36227, #20127, .T. ) ;
#15583 = AXIS2_PLACEMENT_3D ( 'NONE', #33957, #40916, #11274 ) ;
#15584 = ORIENTED_EDGE ( 'NONE', *, *, #40000, .F. ) ;
#15585 = ORIENTED_EDGE ( 'NONE', *, *, #23264, .T. ) ;
#15586 = FACE_OUTER_BOUND ( 'NONE', #20467, .T. ) ;
#15587 = CARTESIAN_POINT ( 'NONE',  ( 0.000000000000000000, -51.98489025774377126, 108.7109110710159854 ) ) ;
#15588 = DIRECTION ( 'NONE',  ( -1.000000000000000000, 0.000000000000000000, 0.000000000000000000 ) ) ;
#15589 = DIRECTION ( 'NONE',  ( -1.000000000000000000, -0.000000000000000000, -0.000000000000000000 ) ) ;
#15590 = ORIENTED_EDGE ( 'NONE', *, *, #10115, .T. ) ;
#15591 = DIRECTION ( 'NONE',  ( -0.000000000000000000, -0.000000000000000000, -1.000000000000000000 ) ) ;
#15592 = VERTEX_POINT ( 'NONE', #19962 ) ;
#15593 = DIRECTION ( 'NONE',  ( -3.996523416598930318E-16, 2.658563593772947863E-15, 1.000000000000000000 ) ) ;
#15594 = CARTESIAN_POINT ( 'NONE',  ( 1.039096088315723056E-14, -6.912265343809663812E-14, -26.00000000000000355 ) ) ;
#15595 = CARTESIAN_POINT ( 'NONE',  ( 139.5000000000000000, 1.708382284810557841E-14, 9.999999999999998224 ) ) ;
#15596 = CIRCLE ( 'NONE', #39244, 36.00000000000000000 ) ;
#15597 = DIRECTION ( 'NONE',  ( 0.000000000000000000, 0.000000000000000000, 1.000000000000000000 ) ) ;
#15598 = ORIENTED_EDGE ( 'NONE', *, *, #41616, .F. ) ;
#15599 = ORIENTED_EDGE ( 'NONE', *, *, #41457, .T. ) ;
#15600 = CARTESIAN_POINT ( 'NONE',  ( 0.000000000000000000, 150.5000000000000284, 10.00000000000000000 ) ) ;
#15601 = AXIS2_PLACEMENT_3D ( 'NONE', #1336, #5482, #4836 ) ;
#15602 = EDGE_CURVE ( 'NONE', #42205, #2052, #19437, .T. ) ;
#15603 = ORIENTED_EDGE ( 'NONE', *, *, #2076, .T. ) ;
#15605 = VERTEX_POINT ( 'NONE', #29976 ) ;
#15604 = DIRECTION ( 'NONE',  ( 0.000000000000000000, 0.000000000000000000, 1.000000000000000000 ) ) ;
#15606 = CARTESIAN_POINT ( 'NONE',  ( -16.19793102917653371, 31.00000000000000355, 47.43702525407732651 ) ) ;
#15608 = ADVANCED_FACE ( 'NONE', ( #26271 ), #42597, .T. ) ;
#15607 = VERTEX_POINT ( 'NONE', #33441 ) ;
#15609 = CARTESIAN_POINT ( 'NONE',  ( 0.000000000000000000, 30.93515269692163017, -36.04401931830219752 ) ) ;
#15610 = CARTESIAN_POINT ( 'NONE',  ( 17.99999999999999645, -12.43843445475238063, -111.5058645182330963 ) ) ;
#15611 = VERTEX_POINT ( 'NONE', #19316 ) ;
#15613 = CARTESIAN_POINT ( 'NONE',  ( 76.69346925290108175, 39.99999999999999289, 10.21457306974340007 ) ) ;
#15612 = AXIS2_PLACEMENT_3D ( 'NONE', #15625, #19131, #41787 ) ;
#15615 = CARTESIAN_POINT ( 'NONE',  ( -142.5000000000000284, 1.745121688784978386E-14, -25.00000000000000000 ) ) ;
#15614 = DIRECTION ( 'NONE',  ( 0.000000000000000000, 0.9574220383620062336, -0.2886919473396182267 ) ) ;
#15616 = DIRECTION ( 'NONE',  ( -1.000000000000000000, 0.000000000000000000, 0.000000000000000000 ) ) ;
#15617 = ORIENTED_EDGE ( 'NONE', *, *, #23393, .F. ) ;
#15618 = DIRECTION ( 'NONE',  ( 0.000000000000000000, 0.000000000000000000, 1.000000000000000000 ) ) ;
#15619 = CIRCLE ( 'NONE', #933, 52.00000000000000000 ) ;
#15620 = EDGE_CURVE ( 'NONE', #41781, #39732, #32586, .T. ) ;
#15621 = EDGE_LOOP ( 'NONE', ( #17231, #2770, #19607, #37391 ) ) ;
#15622 = DIRECTION ( 'NONE',  ( 0.000000000000000000, 0.000000000000000000, -1.000000000000000000 ) ) ;
#15623 = DIRECTION ( 'NONE',  ( 0.000000000000000000, -1.000000000000000000, 0.000000000000000000 ) ) ;
#15624 = CARTESIAN_POINT ( 'NONE',  ( -4.417864660710832503, 31.00000000000000355, 67.60416666563759236 ) ) ;
#15626 = CARTESIAN_POINT ( 'NONE',  ( 18.00000000000000355, -43.55304910509384797, -28.41006711800031681 ) ) ;
#15625 = CARTESIAN_POINT ( 'NONE',  ( 0.000000000000000000, 0.000000000000000000, 0.000000000000000000 ) ) ;
#15627 = ORIENTED_EDGE ( 'NONE', *, *, #34010, .T. ) ;
#15628 = AXIS2_PLACEMENT_3D ( 'NONE', #40975, #33367, #17032 ) ;
#15629 = DIRECTION ( 'NONE',  ( -1.000000000000000000, -0.000000000000000000, -0.000000000000000000 ) ) ;
#15630 = ADVANCED_FACE ( 'NONE', ( #16032 ), #32793, .T. ) ;
#15631 = AXIS2_PLACEMENT_3D ( 'NONE', #5435, #18799, #2136 ) ;
#15632 = VERTEX_POINT ( 'NONE', #23021 ) ;
#15633 = CYLINDRICAL_SURFACE ( 'NONE', #40963, 59.00000000000000000 ) ;
#15634 = ADVANCED_FACE ( 'NONE', ( #36266, #19738 ), #33000, .T. ) ;
#15635 = DIRECTION ( 'NONE',  ( 0.000000000000000000, 0.000000000000000000, 1.000000000000000000 ) ) ;
#15636 = CARTESIAN_POINT ( 'NONE',  ( -6.060882879309181348, 31.00000000000000355, -94.40013096059719544 ) ) ;
#15637 = CARTESIAN_POINT ( 'NONE',  ( -32.34013556242301490, 40.00000000000000000, 94.87070470178476000 ) ) ;
#15638 = CARTESIAN_POINT ( 'NONE',  ( 0.000000000000000000, -0.6819280456836842585, 115.9979955608738607 ) ) ;
#15639 = EDGE_CURVE ( 'NONE', #39440, #6140, #24318, .T. ) ;
#15640 = AXIS2_PLACEMENT_3D ( 'NONE', #30593, #14449, #23637 ) ;
#15641 = ORIENTED_EDGE ( 'NONE', *, *, #30745, .T. ) ;
#15642 = CARTESIAN_POINT ( 'NONE',  ( 3.349226789952652439, 2.685125164760731487, -0.2236248678334773199 ) ) ;
#15643 = EDGE_LOOP ( 'NONE', ( #15249, #38276, #12633 ) ) ;
#15644 = DIRECTION ( 'NONE',  ( -1.000000000000000000, -0.000000000000000000, -0.000000000000000000 ) ) ;
#15646 = ORIENTED_EDGE ( 'NONE', *, *, #28509, .F. ) ;
#15645 = CARTESIAN_POINT ( 'NONE',  ( 17.99999999999999645, -95.38615066514023511, 59.07414607872794932 ) ) ;
#15647 = CARTESIAN_POINT ( 'NONE',  ( -10.00000000000000000, 0.000000000000000000, 0.000000000000000000 ) ) ;
#15648 = ORIENTED_EDGE ( 'NONE', *, *, #3207, .T. ) ;
#15649 = FACE_BOUND ( 'NONE', #12657, .T. ) ;
#15650 = AXIS2_PLACEMENT_3D ( 'NONE', #32699, #10215, #36175 ) ;
#15651 = CYLINDRICAL_SURFACE ( 'NONE', #7467, 59.00000000000000000 ) ;
#15652 = CIRCLE ( 'NONE', #40702, 20.00000000000000711 ) ;
#15653 = DIRECTION ( 'NONE',  ( -1.734723475976807341E-16, 1.000000000000000000, 0.000000000000000000 ) ) ;
#15654 = CIRCLE ( 'NONE', #39984, 13.40000000000000213 ) ;
#15655 = ORIENTED_EDGE ( 'NONE', *, *, #40623, .F. ) ;
#15656 = ADVANCED_FACE ( 'NONE', ( #30620 ), #27342, .T. ) ;
#15657 = CARTESIAN_POINT ( 'NONE',  ( 0.000000000000000000, 0.000000000000000000, 0.000000000000000000 ) ) ;
#15658 = EDGE_CURVE ( 'NONE', #189, #32209, #33649, .T. ) ;
#15659 = LINE ( 'NONE', #42873, #16956 ) ;
#15660 = EDGE_CURVE ( 'NONE', #36933, #7190, #4178, .T. ) ;
#15661 = EDGE_CURVE ( 'NONE', #42889, #8370, #6841, .T. ) ;
#15662 = EDGE_CURVE ( 'NONE', #42412, #42546, #31039, .T. ) ;
#15663 = AXIS2_PLACEMENT_3D ( 'NONE', #1482, #1699, #22041 ) ;
#15665 = ORIENTED_EDGE ( 'NONE', *, *, #41231, .F. ) ;
#15664 = CARTESIAN_POINT ( 'NONE',  ( 18.00000000000000355, -32.00046193115174731, 34.40241257139675923 ) ) ;
#15666 = AXIS2_PLACEMENT_3D ( 'NONE', #8003, #18099, #7575 ) ;
#15667 = ORIENTED_EDGE ( 'NONE', *, *, #19902, .F. ) ;
#15668 = CARTESIAN_POINT ( 'NONE',  ( 18.00000000000000355, 46.90537658765331486, 2.727856614654470491 ) ) ;
#15669 = DIRECTION ( 'NONE',  ( 0.000000000000000000, 0.000000000000000000, 1.000000000000000000 ) ) ;
#15670 = CARTESIAN_POINT ( 'NONE',  ( 5.928665350384931365, 40.00000000000000000, -44.40877992885556580 ) ) ;
#15671 = CARTESIAN_POINT ( 'NONE',  ( -147.8499999999987438, -2.957510437470159335E-13, 10.00000000000004441 ) ) ;
#15672 = DIRECTION ( 'NONE',  ( 1.000000000000000000, 0.000000000000000000, 0.000000000000000000 ) ) ;
#15673 = FACE_OUTER_BOUND ( 'NONE', #12342, .T. ) ;
#15674 = VERTEX_POINT ( 'NONE', #17112 ) ;
#15675 = FACE_OUTER_BOUND ( 'NONE', #40640, .T. ) ;
#15676 = CIRCLE ( 'NONE', #33078, 116.0000000000000000 ) ;
#15677 = EDGE_LOOP ( 'NONE', ( #4840, #39964, #2283, #30672 ) ) ;
#15678 = DIRECTION ( 'NONE',  ( 1.000000000000000000, -0.000000000000000000, -0.000000000000000000 ) ) ;
#15679 = DIRECTION ( 'NONE',  ( -1.000000000000000000, -0.000000000000000000, 0.000000000000000000 ) ) ;
#15680 = CARTESIAN_POINT ( 'NONE',  ( -39.89583333501392559, 31.00000000000000355, 2.617993869485681468 ) ) ;
#15681 = ORIENTED_EDGE ( 'NONE', *, *, #26928, .T. ) ;
#15682 = LINE ( 'NONE', #38555, #14905 ) ;
#15683 = ORIENTED_EDGE ( 'NONE', *, *, #15390, .F. ) ;
#15684 = CIRCLE ( 'NONE', #12869, 13.59999999999999964 ) ;
#15685 = AXIS2_PLACEMENT_3D ( 'NONE', #813, #20511, #23780 ) ;
#15686 = LINE ( 'NONE', #22901, #33034 ) ;
#15687 = EDGE_CURVE ( 'NONE', #13955, #7485, #35340, .T. ) ;
#15688 = CARTESIAN_POINT ( 'NONE',  ( 57.05379307149791401, 31.00000000000000000, -74.37948018729004218 ) ) ;
#15689 = AXIS2_PLACEMENT_3D ( 'NONE', #23009, #21192, #30555 ) ;
#15690 = EDGE_CURVE ( 'NONE', #20538, #17206, #27707, .T. ) ;
#15691 = CARTESIAN_POINT ( 'NONE',  ( 0.000000000000000000, -37.07968990261405651, -109.9140418541961282 ) ) ;
#15692 = ORIENTED_EDGE ( 'NONE', *, *, #5673, .T. ) ;
#15693 = CARTESIAN_POINT ( 'NONE',  ( 65.23019871247133494, 31.00000000000000000, 17.57949444736449252 ) ) ;
#15694 = COLOUR_RGB ( '', 0.09019608, 0.27058824, 0.51372549) ;
#15695 = FACE_OUTER_BOUND ( 'NONE', #33786, .T. ) ;
#15696 = VECTOR ( 'NONE', #4013, 1000.000000000000000 ) ;
#15697 = ORIENTED_EDGE ( 'NONE', *, *, #30087, .T. ) ;
#15698 = CYLINDRICAL_SURFACE ( 'NONE', #42210, 47.49900000000000233 ) ;
#15699 = DIRECTION ( 'NONE',  ( -1.000000000000000000, 0.000000000000000000, 0.000000000000000000 ) ) ;
#15700 = DIRECTION ( 'NONE',  ( 0.000000000000000000, 0.7525707698561353576, 0.6585113790650422017 ) ) ;
#15702 = ORIENTED_EDGE ( 'NONE', *, *, #4930, .T. ) ;
#15701 = CARTESIAN_POINT ( 'NONE',  ( 0.000000000000000000, -113.8630351447204134, -22.16324045874526405 ) ) ;
#15703 = CARTESIAN_POINT ( 'NONE',  ( 22.90854556226710415, -40.05525454449572464, -74.83297477053821467 ) ) ;
#15704 = CARTESIAN_POINT ( 'NONE',  ( 18.00000000000000355, 0.000000000000000000, 0.000000000000000000 ) ) ;
#15705 = AXIS2_PLACEMENT_3D ( 'NONE', #41938, #12086, #34975 ) ;
#15706 = ORIENTED_EDGE ( 'NONE', *, *, #6177, .F. ) ;
#15707 = CARTESIAN_POINT ( 'NONE',  ( -53.60515337853228601, 40.00000000000000000, -47.01024902908782366 ) ) ;
#15708 = CARTESIAN_POINT ( 'NONE',  ( 19.99999999999990408, -9.415137969927464789E-14, -26.00000000000001066 ) ) ;
#15709 = ORIENTED_EDGE ( 'NONE', *, *, #12622, .T. ) ;
#15710 = EDGE_CURVE ( 'NONE', #23276, #13537, #19372, .T. ) ;
#15711 = CARTESIAN_POINT ( 'NONE',  ( 17.99999999999999645, 109.3506818544110217, 38.70953859161051014 ) ) ;
#15712 = ADVANCED_FACE ( 'NONE', ( #901 ), #13837, .F. ) ;
#15713 = EDGE_CURVE ( 'NONE', #41781, #19147, #34657, .T. ) ;
#15714 = AXIS2_PLACEMENT_3D ( 'NONE', #7963, #40898, #17830 ) ;
#15715 = ORIENTED_EDGE ( 'NONE', *, *, #31113, .F. ) ;
#15716 = AXIS2_PLACEMENT_3D ( 'NONE', #11421, #24754, #38007 ) ;
#15717 = EDGE_CURVE ( 'NONE', #37692, #3781, #11665, .T. ) ;
#15718 = ORIENTED_EDGE ( 'NONE', *, *, #37791, .T. ) ;
#15719 = FACE_OUTER_BOUND ( 'NONE', #37502, .T. ) ;
#15720 = EDGE_LOOP ( 'NONE', ( #16663, #10615 ) ) ;
#15721 = CIRCLE ( 'NONE', #17823, 59.00000000000000000 ) ;
#15722 = CYLINDRICAL_SURFACE ( 'NONE', #13310, 59.00000000000000000 ) ;
#15723 = CARTESIAN_POINT ( 'NONE',  ( 0.000000000000000000, -40.47821179127737423, 32.64221760512745618 ) ) ;
#15724 = DIRECTION ( 'NONE',  ( -1.000000000000000000, 0.000000000000000000, -0.000000000000000000 ) ) ;
#15725 = ADVANCED_FACE ( 'NONE', ( #7684 ), #17999, .F. ) ;
#15726 = DIRECTION ( 'NONE',  ( 0.000000000000000000, 0.000000000000000000, -1.000000000000000000 ) ) ;
#15727 = ORIENTED_EDGE ( 'NONE', *, *, #11342, .T. ) ;
#15728 = DIRECTION ( 'NONE',  ( 0.000000000000000000, 0.000000000000000000, 1.000000000000000000 ) ) ;
#15729 = ORIENTED_EDGE ( 'NONE', *, *, #10619, .F. ) ;
#15730 = DIRECTION ( 'NONE',  ( -1.000000000000000000, 0.000000000000000000, 0.000000000000000000 ) ) ;
#15731 = ORIENTED_EDGE ( 'NONE', *, *, #14492, .F. ) ;
#15732 = DIRECTION ( 'NONE',  ( 1.000000000000000000, 0.000000000000000000, 0.000000000000000000 ) ) ;
#15733 = DIRECTION ( 'NONE',  ( 0.000000000000000000, 0.000000000000000000, 1.000000000000000000 ) ) ;
#15734 = CARTESIAN_POINT ( 'NONE',  ( 4.000000000000000000, -2.309401076758514915, -3.433295621305383349 ) ) ;
#15735 = CARTESIAN_POINT ( 'NONE',  ( 52.68777711438346500, 31.00000000000000355, 17.88338314711659294 ) ) ;
#15736 = AXIS2_PLACEMENT_3D ( 'NONE', #35801, #5929, #36239 ) ;
#15737 = ORIENTED_EDGE ( 'NONE', *, *, #17797, .F. ) ;
#15738 = CYLINDRICAL_SURFACE ( 'NONE', #31048, 59.00000000000000000 ) ;
#15739 = ADVANCED_FACE ( 'NONE', ( #27791 ), #37782, .T. ) ;
#15741 = ORIENTED_EDGE ( 'NONE', *, *, #41190, .T. ) ;
#15740 = AXIS2_PLACEMENT_3D ( 'NONE', #39135, #6620, #36081 ) ;
#15742 = AXIS2_PLACEMENT_3D ( 'NONE', #38612, #22098, #15533 ) ;
#15743 = CARTESIAN_POINT ( 'NONE',  ( -17.60292107714122878, 40.00000000000000000, 65.74579412301164894 ) ) ;
#15744 = AXIS2_PLACEMENT_3D ( 'NONE', #39920, #36226, #9837 ) ;
#15745 = CIRCLE ( 'NONE', #1760, 59.00000000000000000 ) ;
#15746 = AXIS2_PLACEMENT_3D ( 'NONE', #35043, #28322, #41587 ) ;
#15747 = CYLINDRICAL_SURFACE ( 'NONE', #1859, 51.99999999999999289 ) ;
#15748 = AXIS2_PLACEMENT_3D ( 'NONE', #23733, #14125, #11271 ) ;
#15749 = CARTESIAN_POINT ( 'NONE',  ( 0.000000000000000000, 45.89132998248050654, 102.3829004574631512 ) ) ;
#15750 = CIRCLE ( 'NONE', #15083, 20.00000000000000355 ) ;
#15751 = CARTESIAN_POINT ( 'NONE',  ( 17.99999999999999645, 110.0562500189198829, 49.07252625220148445 ) ) ;
#15752 = DIRECTION ( 'NONE',  ( -1.000000000000000000, -0.000000000000000000, -0.000000000000000000 ) ) ;
#15753 = AXIS2_PLACEMENT_3D ( 'NONE', #18207, #1348, #31036 ) ;
#15754 = ORIENTED_EDGE ( 'NONE', *, *, #1152, .F. ) ;
#15755 = CARTESIAN_POINT ( 'NONE',  ( -49.46937513889707105, 40.00000000000000000, 6.524320044134898744 ) ) ;
#15756 = CARTESIAN_POINT ( 'NONE',  ( 18.00000000000000355, -51.85248208264514602, -3.914090171286729980 ) ) ;
#15757 = DIRECTION ( 'NONE',  ( 1.000000000000000000, 0.000000000000000000, 0.000000000000000000 ) ) ;
#15758 = ORIENTED_EDGE ( 'NONE', *, *, #34930, .T. ) ;
#15759 = DIRECTION ( 'NONE',  ( -1.000000000000000000, 0.000000000000000000, 0.000000000000000000 ) ) ;
#15760 = ADVANCED_FACE ( 'NONE', ( #24529 ), #36921, .T. ) ;
#15761 = ORIENTED_EDGE ( 'NONE', *, *, #29885, .T. ) ;
#15762 = DIRECTION ( 'NONE',  ( -1.000000000000000000, 3.942553354492743901E-17, 0.000000000000000000 ) ) ;
#15763 = ORIENTED_EDGE ( 'NONE', *, *, #5348, .T. ) ;
#15764 = ORIENTED_EDGE ( 'NONE', *, *, #9014, .F. ) ;
#15765 = CARTESIAN_POINT ( 'NONE',  ( 17.99999999999999645, 0.000000000000000000, 0.000000000000000000 ) ) ;
#15766 = CARTESIAN_POINT ( 'NONE',  ( 10.26812810425290579, 31.00000000000000355, 78.79123036457541218 ) ) ;
#15767 = ORIENTED_EDGE ( 'NONE', *, *, #36954, .F. ) ;
#15768 = DIRECTION ( 'NONE',  ( 0.000000000000000000, 0.000000000000000000, 1.000000000000000000 ) ) ;
#15769 = CIRCLE ( 'NONE', #33149, 130.0000000000013927 ) ;
#15771 = CARTESIAN_POINT ( 'NONE',  ( 9.000000000000001776, 0.6505223195683029758, 51.99593080916758936 ) ) ;
#15770 = CIRCLE ( 'NONE', #26194, 58.99999999999999289 ) ;
#15772 = VERTEX_POINT ( 'NONE', #7243 ) ;
#15773 = EDGE_CURVE ( 'NONE', #33862, #13871, #10972, .T. ) ;
#15774 = DIRECTION ( 'NONE',  ( 0.000000000000000000, 0.000000000000000000, 1.000000000000000000 ) ) ;
#15775 = CARTESIAN_POINT ( 'NONE',  ( -98.36195137680903144, 40.00000000000000711, 26.22212808230024805 ) ) ;
#15776 = PRESENTATION_LAYER_ASSIGNMENT (  '', '', ( #26913 ) ) ;
#15777 = DIRECTION ( 'NONE',  ( 0.000000000000000000, -0.9407002666710296834, -0.3392388661180402165 ) ) ;
#15778 = EDGE_CURVE ( 'NONE', #12201, #4714, #40896, .T. ) ;
#15780 = DIRECTION ( 'NONE',  ( 0.000000000000000000, 0.000000000000000000, 1.000000000000000000 ) ) ;
#15779 = CYLINDRICAL_SURFACE ( 'NONE', #27315, 20.00000000000000355 ) ;
#15781 = CIRCLE ( 'NONE', #405, 47.49900000000000233 ) ;
#15782 = AXIS2_PLACEMENT_3D ( 'NONE', #23401, #17512, #21013 ) ;
#15783 = DIRECTION ( 'NONE',  ( 0.000000000000000000, 0.000000000000000000, 1.000000000000000000 ) ) ;
#15784 = DIRECTION ( 'NONE',  ( 0.000000000000000000, -0.6736956436465638687, 0.7390089172206529833 ) ) ;
#15785 = ORIENTED_EDGE ( 'NONE', *, *, #41231, .T. ) ;
#15786 = AXIS2_PLACEMENT_3D ( 'NONE', #26333, #42447, #29182 ) ;
#15787 = CARTESIAN_POINT ( 'NONE',  ( 34.56606645648713538, 31.00000000000000355, -4.560848911255810378 ) ) ;
#15788 = ORIENTED_EDGE ( 'NONE', *, *, #5477, .T. ) ;
#15789 = DIRECTION ( 'NONE',  ( 0.000000000000000000, 0.9968120070307497915, 0.07978610555308651708 ) ) ;
#15790 = CARTESIAN_POINT ( 'NONE',  ( 17.99999999999999645, 0.000000000000000000, 0.000000000000000000 ) ) ;
#15791 = VERTEX_POINT ( 'NONE', #15138 ) ;
#15792 = CARTESIAN_POINT ( 'NONE',  ( -30.01493782828161017, 40.00000000000000000, -3.947526014606304035 ) ) ;
#15793 = CARTESIAN_POINT ( 'NONE',  ( -16.82630558382439290, 40.00000000000000000, -29.24196894321155682 ) ) ;
#15794 = EDGE_LOOP ( 'NONE', ( #14042, #21149, #16852, #229 ) ) ;
#15795 = VERTEX_POINT ( 'NONE', #8979 ) ;
#15796 = FILL_AREA_STYLE_COLOUR ( '', #40836 ) ;
#15797 = CARTESIAN_POINT ( 'NONE',  ( -31.75000000000000000, 0.000000000000000000, 0.000000000000000000 ) ) ;
#15798 = VECTOR ( 'NONE', #2212, 1000.000000000000000 ) ;
#15799 = CYLINDRICAL_SURFACE ( 'NONE', #41402, 120.5010000000000190 ) ;
#15800 = AXIS2_PLACEMENT_3D ( 'NONE', #13746, #4091, #13957 ) ;
#15801 = CIRCLE ( 'NONE', #31116, 12.50000000000000000 ) ;
#15802 = CARTESIAN_POINT ( 'NONE',  ( 56.25020680251638083, -2.055254544495725977, 2.972870684497274762 ) ) ;
#15803 = CIRCLE ( 'NONE', #40145, 59.00000000000000000 ) ;
#15804 = DIRECTION ( 'NONE',  ( 0.000000000000000000, 0.4132121857683728749, 0.9106347728549155640 ) ) ;
#15805 = ORIENTED_EDGE ( 'NONE', *, *, #42461, .T. ) ;
#15806 = CARTESIAN_POINT ( 'NONE',  ( -6.259644161404860030E-16, -4.618802153517027165, -5.000000000000000000 ) ) ;
#15807 = ORIENTED_EDGE ( 'NONE', *, *, #40703, .F. ) ;
#15808 = CYLINDRICAL_SURFACE ( 'NONE', #12473, 13.59999999999999964 ) ;
#15809 = DIRECTION ( 'NONE',  ( 7.831767060816205381E-16, -2.691216939431690932E-15, 1.000000000000000000 ) ) ;
#15810 = VECTOR ( 'NONE', #38314, 1000.000000000000000 ) ;
#15811 = DIRECTION ( 'NONE',  ( -1.000000000000000000, -0.000000000000000000, -0.000000000000000000 ) ) ;
#15812 = EDGE_CURVE ( 'NONE', #36979, #20273, #3260, .T. ) ;
#15813 = DIRECTION ( 'NONE',  ( 0.000000000000000000, -0.8747630845319657178, 0.4845508703326421029 ) ) ;
#15814 = VERTEX_POINT ( 'NONE', #24974 ) ;
#15815 = CARTESIAN_POINT ( 'NONE',  ( 61.87885091699251916, 39.99999999999999289, -70.55635664373320992 ) ) ;
#15816 = VERTEX_POINT ( 'NONE', #31477 ) ;
#15817 = EDGE_CURVE ( 'NONE', #39668, #35149, #42979, .T. ) ;
#15818 = DIRECTION ( 'NONE',  ( 0.000000000000000000, 1.000000000000000000, -1.060184893785364939E-15 ) ) ;
#15819 = VERTEX_POINT ( 'NONE', #1990 ) ;
#15821 = ORIENTED_EDGE ( 'NONE', *, *, #16669, .T. ) ;
#15820 = DIRECTION ( 'NONE',  ( 0.000000000000000000, 0.4132121857683791477, -0.9106347728549126774 ) ) ;
#15822 = CIRCLE ( 'NONE', #25014, 120.5010000000000190 ) ;
#15823 = CARTESIAN_POINT ( 'NONE',  ( 6.367266499441480043, 31.00000000000000355, 48.98256792610027333 ) ) ;
#15824 = ORIENTED_EDGE ( 'NONE', *, *, #14351, .T. ) ;
#15825 = CARTESIAN_POINT ( 'NONE',  ( 0.000000000000000000, 28.62203781743003717, -14.19692359621465094 ) ) ;
#15826 = EDGE_CURVE ( 'NONE', #23382, #26511, #36728, .T. ) ;
#15827 = FACE_BOUND ( 'NONE', #16750, .T. ) ;
#15828 = PRODUCT_DEFINITION_SHAPE ( 'NONE', 'NONE',  #27627 ) ;
#15829 = ORIENTED_EDGE ( 'NONE', *, *, #36398, .F. ) ;
#15830 = CARTESIAN_POINT ( 'NONE',  ( 61.98103557012430542, 39.99999999999999289, 47.69015029125304039 ) ) ;
#15831 = EDGE_CURVE ( 'NONE', #39546, #6952, #24961, .T. ) ;
#15832 = CIRCLE ( 'NONE', #26971, 59.00000000000000000 ) ;
#15834 = CARTESIAN_POINT ( 'NONE',  ( 17.99999999999999645, 0.000000000000000000, 0.000000000000000000 ) ) ;
#15833 = CARTESIAN_POINT ( 'NONE',  ( -17.44537629401976631, 31.00000000000000000, -4.261559264950514958 ) ) ;
#15835 = CARTESIAN_POINT ( 'NONE',  ( -12.49999999999991829, -1.009307908086780017E-13, -44.99999999999998579 ) ) ;
#15836 = VERTEX_POINT ( 'NONE', #28848 ) ;
#15837 = CARTESIAN_POINT ( 'NONE',  ( -105.9879088449591933, 17.11489954122026447, -0.3807199291576673361 ) ) ;
#15838 = AXIS2_PLACEMENT_3D ( 'NONE', #8579, #31946, #28887 ) ;
#15839 = VERTEX_POINT ( 'NONE', #22330 ) ;
#15840 = CYLINDRICAL_SURFACE ( 'NONE', #12816, 116.0000000000000000 ) ;
#15841 = CYLINDRICAL_SURFACE ( 'NONE', #6684, 20.00000000000000355 ) ;
#15842 = AXIS2_PLACEMENT_3D ( 'NONE', #24367, #20229, #27392 ) ;
#15843 = CARTESIAN_POINT ( 'NONE',  ( 8.815036365794538753, 31.00000000000000355, 66.85656860134390911 ) ) ;
#15845 = CARTESIAN_POINT ( 'NONE',  ( 0.000000000000000000, 0.000000000000000000, -11.00000000000000000 ) ) ;
#15844 = DIRECTION ( 'NONE',  ( -1.000000000000000000, -0.000000000000000000, -0.000000000000000000 ) ) ;
#15847 = VERTEX_POINT ( 'NONE', #25599 ) ;
#15846 = AXIS2_PLACEMENT_3D ( 'NONE', #27835, #38050, #8380 ) ;
#15848 = AXIS2_PLACEMENT_3D ( 'NONE', #33846, #663, #7009 ) ;
#15849 = EDGE_CURVE ( 'NONE', #23547, #14512, #38638, .T. ) ;
#15851 = CIRCLE ( 'NONE', #33849, 59.00000000000000000 ) ;
#15850 = CYLINDRICAL_SURFACE ( 'NONE', #25450, 20.00000000000000711 ) ;
#15852 = EDGE_CURVE ( 'NONE', #38270, #41456, #1193, .T. ) ;
#15853 = CIRCLE ( 'NONE', #41615, 36.00000000000000000 ) ;
#15854 = ORIENTED_EDGE ( 'NONE', *, *, #29349, .F. ) ;
#15855 = LINE ( 'NONE', #42427, #22761 ) ;
#15856 = EDGE_CURVE ( 'NONE', #30953, #12005, #35378, .T. ) ;
#15857 = CARTESIAN_POINT ( 'NONE',  ( 0.000000000000000000, 0.000000000000000000, 0.000000000000000000 ) ) ;
#15858 = CARTESIAN_POINT ( 'NONE',  ( -91.59543978412355614, 31.00000000000000711, -12.18496625896582231 ) ) ;
#15859 = CARTESIAN_POINT ( 'NONE',  ( 31.77777543000702565, 40.00000000000000000, 93.95825142774114624 ) ) ;
#15860 = DIRECTION ( 'NONE',  ( -3.009274222672345096E-17, -1.000000000000000000, 2.455023325076454960E-18 ) ) ;
#15861 = VERTEX_POINT ( 'NONE', #31911 ) ;
#15862 = CARTESIAN_POINT ( 'NONE',  ( 17.99999999999999645, 112.1427988504407551, 3.502162136923788083 ) ) ;
#15863 = VERTEX_POINT ( 'NONE', #5496 ) ;
#15864 = DIRECTION ( 'NONE',  ( -1.000000000000000000, 0.000000000000000000, -0.000000000000000000 ) ) ;
#15865 = CIRCLE ( 'NONE', #38139, 120.5010000000000190 ) ;
#15866 = DIRECTION ( 'NONE',  ( 1.000000000000000000, 0.000000000000000000, 0.000000000000000000 ) ) ;
#15867 = CARTESIAN_POINT ( 'NONE',  ( 17.99999999999999645, 15.21076497709711184, 119.5371223922155792 ) ) ;
#15868 = ORIENTED_EDGE ( 'NONE', *, *, #33951, .F. ) ;
#15869 = CARTESIAN_POINT ( 'NONE',  ( 0.000000000000000000, -108.8880088604273766, -39.99251838046071583 ) ) ;
#15870 = CIRCLE ( 'NONE', #40210, 0.7500000000000006661 ) ;
#15871 = EDGE_CURVE ( 'NONE', #28956, #29146, #24335, .T. ) ;
#15872 = DIRECTION ( 'NONE',  ( -1.000000000000000000, -0.000000000000000000, 0.000000000000000000 ) ) ;
#15873 = AXIS2_PLACEMENT_3D ( 'NONE', #2192, #11853, #42116 ) ;
#15874 = LINE ( 'NONE', #26744, #28523 ) ;
#15875 = AXIS2_PLACEMENT_3D ( 'NONE', #16420, #5180, #6357 ) ;
#15876 = AXIS2_PLACEMENT_3D ( 'NONE', #15241, #41799, #8636 ) ;
#15877 = AXIS2_PLACEMENT_3D ( 'NONE', #4901, #38273, #28056 ) ;
#15878 = ORIENTED_EDGE ( 'NONE', *, *, #22140, .F. ) ;
#15879 = CARTESIAN_POINT ( 'NONE',  ( 102.9999999999993321, -2.372200916521104037E-13, -32.00000000000000000 ) ) ;
#15880 = FACE_OUTER_BOUND ( 'NONE', #498, .T. ) ;
#15881 = AXIS2_PLACEMENT_3D ( 'NONE', #29971, #13390, #40394 ) ;
#15882 = EDGE_CURVE ( 'NONE', #7958, #7274, #8875, .T. ) ;
#15884 = ORIENTED_EDGE ( 'NONE', *, *, #21035, .F. ) ;
#15883 = CARTESIAN_POINT ( 'NONE',  ( -105.9879088449591933, 40.00000000000000000, -0.3807199291576673361 ) ) ;
#15885 = ORIENTED_EDGE ( 'NONE', *, *, #34113, .F. ) ;
#15886 = CARTESIAN_POINT ( 'NONE',  ( 0.000000000000000000, -49.25004636492376875, -16.68630974939812006 ) ) ;
#15887 = DIRECTION ( 'NONE',  ( 0.000000000000000000, 0.000000000000000000, -1.000000000000000000 ) ) ;
#15888 = CARTESIAN_POINT ( 'NONE',  ( 46.89194940766294906, 40.00000000000000000, 6.259973086888630078 ) ) ;
#15889 = DIRECTION ( 'NONE',  ( 0.000000000000000000, -0.5963673585385078635, 0.8027116379309587879 ) ) ;
#15890 = CIRCLE ( 'NONE', #28445, 2.041999999999999815 ) ;
#15891 = EDGE_CURVE ( 'NONE', #39546, #7856, #5696, .T. ) ;
#15892 = CYLINDRICAL_SURFACE ( 'NONE', #516, 18.77999999999999403 ) ;
#15893 = ADVANCED_FACE ( 'NONE', ( #31683 ), #14469, .T. ) ;
#15894 = CARTESIAN_POINT ( 'NONE',  ( 0.000000000000000000, 0.000000000000000000, -25.00000000000000000 ) ) ;
#15895 = ORIENTED_EDGE ( 'NONE', *, *, #32402, .T. ) ;
#15896 = DIRECTION ( 'NONE',  ( -1.000000000000000000, -0.000000000000000000, -0.000000000000000000 ) ) ;
#15897 = ORIENTED_EDGE ( 'NONE', *, *, #33479, .T. ) ;
#15898 = DIRECTION ( 'NONE',  ( 1.000000000000000000, 0.000000000000000000, 0.000000000000000000 ) ) ;
#15899 = DIRECTION ( 'NONE',  ( -1.000000000000000000, -0.000000000000000000, 0.000000000000000000 ) ) ;
#15900 = CARTESIAN_POINT ( 'NONE',  ( 34.89583333524210218, 31.00000000000000355, -2.290744634698907767 ) ) ;
#15901 = AXIS2_PLACEMENT_3D ( 'NONE', #8588, #21950, #5332 ) ;
#15902 = CARTESIAN_POINT ( 'NONE',  ( 0.000000000000000000, -17.77780072541623113, -114.6296200873377842 ) ) ;
#15903 = ORIENTED_EDGE ( 'NONE', *, *, #27935, .T. ) ;
#15904 = AXIS2_PLACEMENT_3D ( 'NONE', #20115, #33585, #9811 ) ;
#15905 = AXIS2_PLACEMENT_3D ( 'NONE', #24479, #7633, #11147 ) ;
#15906 = CARTESIAN_POINT ( 'NONE',  ( 9.000000000000001776, 42.87700105098753056, -107.7847984684000551 ) ) ;
#15907 = CARTESIAN_POINT ( 'NONE',  ( -11.47416535668642723, 31.00000000000000355, 87.14428777381637303 ) ) ;
#15908 = VECTOR ( 'NONE', #34705, 1000.000000000000000 ) ;
#15909 = AXIS2_PLACEMENT_3D ( 'NONE', #30444, #11029, #23911 ) ;
#15910 = EDGE_CURVE ( 'NONE', #41773, #29952, #29100, .T. ) ;
#15911 = DIRECTION ( 'NONE',  ( 1.058513553088275437E-16, 1.000000000000000000, -8.813324511995299047E-17 ) ) ;
#15912 = ORIENTED_EDGE ( 'NONE', *, *, #13244, .F. ) ;
#15914 = CARTESIAN_POINT ( 'NONE',  ( -59.29355402628473115, 31.00000000000000355, -20.23837177251482800 ) ) ;
#15913 = CIRCLE ( 'NONE', #40249, 36.00000000000000000 ) ;
#15915 = PRODUCT_RELATED_PRODUCT_CATEGORY ( 'part', '', ( #29058 ) ) ;
#15916 = CARTESIAN_POINT ( 'NONE',  ( -53.44803860755722269, 40.00000000000000000, 46.73995993581220176 ) ) ;
#15917 = CARTESIAN_POINT ( 'NONE',  ( 147.8500000000000227, 1.576728355889448963E-12, 9.999999999999998224 ) ) ;
#15918 = ORIENTED_EDGE ( 'NONE', *, *, #38694, .T. ) ;
#15919 = DIRECTION ( 'NONE',  ( 1.000000000000000000, 0.000000000000000000, 0.000000000000000000 ) ) ;
#15920 = DIRECTION ( 'NONE',  ( 0.000000000000000000, 0.2113826236296184047, 0.9774033898178678959 ) ) ;
#15922 = VERTEX_POINT ( 'NONE', #8121 ) ;
#15921 = DIRECTION ( 'NONE',  ( 1.000000000000000000, 0.000000000000000000, 0.000000000000000000 ) ) ;
#15923 = LINE ( 'NONE', #9566, #7246 ) ;
#15924 = CARTESIAN_POINT ( 'NONE',  ( 9.000000000000000000, 31.94619804602787738, -16.59639811537322984 ) ) ;
#15925 = EDGE_CURVE ( 'NONE', #7262, #27181, #21477, .T. ) ;
#15926 = ORIENTED_EDGE ( 'NONE', *, *, #18370, .T. ) ;
#15927 = CARTESIAN_POINT ( 'NONE',  ( -23.19911330973958030, 40.00000000000000000, -68.30030121463531145 ) ) ;
#15928 = FACE_OUTER_BOUND ( 'NONE', #37494, .T. ) ;
#15929 = ORIENTED_EDGE ( 'NONE', *, *, #26695, .T. ) ;
#15930 = CYLINDRICAL_SURFACE ( 'NONE', #2467, 51.99999999999999289 ) ;
#15931 = AXIS2_PLACEMENT_3D ( 'NONE', #15347, #15133, #18850 ) ;
#15932 = DIRECTION ( 'NONE',  ( -0.000000000000000000, -0.000000000000000000, -1.000000000000000000 ) ) ;
#15933 = AXIS2_PLACEMENT_3D ( 'NONE', #37080, #30127, #184 ) ;
#15934 = VERTEX_POINT ( 'NONE', #1565 ) ;
#15935 = CIRCLE ( 'NONE', #29853, 13.59999999999999964 ) ;
#15936 = AXIS2_PLACEMENT_3D ( 'NONE', #9711, #26512, #39787 ) ;
#15937 = EDGE_CURVE ( 'NONE', #11201, #38985, #6624, .T. ) ;
#15938 = EDGE_LOOP ( 'NONE', ( #23174, #20713, #18805, #18131 ) ) ;
#15939 = AXIS2_PLACEMENT_3D ( 'NONE', #709, #40424, #7263 ) ;
#15940 = DIRECTION ( 'NONE',  ( -1.000000000000000000, 0.000000000000000000, 0.000000000000000000 ) ) ;
#15941 = ORIENTED_EDGE ( 'NONE', *, *, #8317, .T. ) ;
#15942 = FACE_OUTER_BOUND ( 'NONE', #33044, .T. ) ;
#15943 = LINE ( 'NONE', #29236, #31130 ) ;
#15944 = ADVANCED_FACE ( 'NONE', ( #29928 ), #33172, .T. ) ;
#15945 = LINE ( 'NONE', #2784, #27507 ) ;
#15946 = DIRECTION ( 'NONE',  ( 0.000000000000000000, 0.000000000000000000, 1.000000000000000000 ) ) ;
#15947 = ORIENTED_EDGE ( 'NONE', *, *, #9040, .T. ) ;
#15948 = CARTESIAN_POINT ( 'NONE',  ( 0.000000000000000000, -80.74349901498355564, -77.90224541347362219 ) ) ;
#15949 = UNCERTAINTY_MEASURE_WITH_UNIT (LENGTH_MEASURE( 1.000000000000000082E-05 ), #20629, 'distance_accuracy_value', 'NONE');
#15950 = EDGE_LOOP ( 'NONE', ( #18477, #6497, #42784, #28753 ) ) ;
#15951 = CARTESIAN_POINT ( 'NONE',  ( 17.99999999999999645, 112.5220807139887853, -28.19186676675730752 ) ) ;
#15952 = EDGE_LOOP ( 'NONE', ( #34993, #37847, #2885, #13447 ) ) ;
#15953 = CARTESIAN_POINT ( 'NONE',  ( 17.99999999999999645, 67.32409792376505209, 89.75376489259387824 ) ) ;
#15954 = DIRECTION ( 'NONE',  ( 0.8191520442889875797, 0.000000000000000000, 0.5735764363510522656 ) ) ;
#15955 = CONTEXT_DEPENDENT_SHAPE_REPRESENTATION ( #28723, #42964 ) ;
#15956 = FACE_OUTER_BOUND ( 'NONE', #21914, .T. ) ;
#15957 = CARTESIAN_POINT ( 'NONE',  ( 42.05404839982585941, 31.00000000000000355, -47.95475229022623864 ) ) ;
#15958 = CARTESIAN_POINT ( 'NONE',  ( 31.80287614962791665, -40.05525454449572464, 69.29271901957253021 ) ) ;
#15959 = ADVANCED_FACE ( 'NONE', ( #12908 ), #26641, .T. ) ;
#15961 = EDGE_CURVE ( 'NONE', #41712, #41179, #6129, .T. ) ;
#15960 = VECTOR ( 'NONE', #31628, 1000.000000000000000 ) ;
#15962 = VERTEX_POINT ( 'NONE', #28905 ) ;
#15963 = CIRCLE ( 'NONE', #40299, 47.49899999999999523 ) ;
#15964 = CARTESIAN_POINT ( 'NONE',  ( -31.99444157862340532, 31.00000000000000355, -4.262017635501121227 ) ) ;
#15965 = EDGE_CURVE ( 'NONE', #235, #15791, #16186, .T. ) ;
#15966 = EDGE_CURVE ( 'NONE', #30619, #16491, #24334, .T. ) ;
#15967 = CARTESIAN_POINT ( 'NONE',  ( 4.745113895470035814, 40.00000000000000000, -72.60416666572081112 ) ) ;
#15968 = CIRCLE ( 'NONE', #6866, 59.00000000000001421 ) ;
#15969 = DIRECTION ( 'NONE',  ( 0.000000000000000000, 0.000000000000000000, 1.000000000000000000 ) ) ;
#15970 = CARTESIAN_POINT ( 'NONE',  ( 18.00000000000000355, 31.08872492060013926, -41.68322423723066805 ) ) ;
#15971 = DIRECTION ( 'NONE',  ( 0.000000000000000000, 0.000000000000000000, 1.000000000000000000 ) ) ;
#15972 = CARTESIAN_POINT ( 'NONE',  ( 0.000000000000000000, 0.000000000000000000, 0.000000000000000000 ) ) ;
#15973 = EDGE_LOOP ( 'NONE', ( #4254, #26899 ) ) ;
#15974 = CARTESIAN_POINT ( 'NONE',  ( -32.14164714139042189, 40.00000000000000000, 36.65395011347077059 ) ) ;
#15975 = CARTESIAN_POINT ( 'NONE',  ( -91.96080130434580724, -40.05525454449572464, 14.45886780445738218 ) ) ;
#15976 = CARTESIAN_POINT ( 'NONE',  ( 0.000000000000000000, -66.49630760163542220, -90.36876423296052963 ) ) ;
#15977 = ORIENTED_EDGE ( 'NONE', *, *, #27198, .T. ) ;
#15978 = DIRECTION ( 'NONE',  ( 0.000000000000000000, 0.6845471059286847293, 0.7289686274214153272 ) ) ;
#15979 = CARTESIAN_POINT ( 'NONE',  ( 17.99999999999999645, -47.58001226230465619, -110.7096808509488284 ) ) ;
#15980 = ORIENTED_EDGE ( 'NONE', *, *, #32583, .F. ) ;
#15981 = DIRECTION ( 'NONE',  ( -1.000000000000000000, -0.000000000000000000, -0.000000000000000000 ) ) ;
#15982 = ORIENTED_EDGE ( 'NONE', *, *, #31090, .F. ) ;
#15983 = ORIENTED_EDGE ( 'NONE', *, *, #3317, .F. ) ;
#15984 = DIRECTION ( 'NONE',  ( 0.000000000000000000, -0.05322217484218560307, 0.9985826956767616114 ) ) ;
#15985 = CARTESIAN_POINT ( 'NONE',  ( -71.82650799747224823, 31.00000000000000711, -41.60779115368423220 ) ) ;
#15986 = EDGE_LOOP ( 'NONE', ( #10519, #22040, #41423, #3032 ) ) ;
#15987 = LINE ( 'NONE', #12702, #9841 ) ;
#15988 = VECTOR ( 'NONE', #24144, 1000.000000000000000 ) ;
#15989 = AXIS2_PLACEMENT_3D ( 'NONE', #31576, #1668, #8441 ) ;
#15990 = DIRECTION ( 'NONE',  ( 0.000000000000000000, -0.9957341762950334685, -0.09226835946331306271 ) ) ;
#15991 = EDGE_CURVE ( 'NONE', #41139, #23382, #20133, .T. ) ;
#15992 = DIRECTION ( 'NONE',  ( 1.000000000000000000, 0.000000000000000000, 0.000000000000000000 ) ) ;
#15993 = AXIS2_PLACEMENT_3D ( 'NONE', #3306, #23862, #26471 ) ;
#15994 = ORIENTED_EDGE ( 'NONE', *, *, #28713, .F. ) ;
#15995 = FACE_OUTER_BOUND ( 'NONE', #24505, .T. ) ;
#15996 = CARTESIAN_POINT ( 'NONE',  ( -101.9959696149863788, 40.00000000000000711, -0.1269066430510139010 ) ) ;
#15997 = LINE ( 'NONE', #42563, #8170 ) ;
#15999 = DIRECTION ( 'NONE',  ( -1.000000000000000000, -0.000000000000000000, -0.000000000000000000 ) ) ;
#15998 = CARTESIAN_POINT ( 'NONE',  ( 17.99999999999999645, -114.8812324315174038, -16.07179003769265080 ) ) ;
#16000 = CARTESIAN_POINT ( 'NONE',  ( 17.99999999999999645, -61.59243992711522964, 93.77976230226020959 ) ) ;
#16001 = ORIENTED_EDGE ( 'NONE', *, *, #17827, .T. ) ;
#16002 = CARTESIAN_POINT ( 'NONE',  ( -14.19360040536685830, 31.00000000000000355, 24.59234967646941783 ) ) ;
#16003 = VERTEX_POINT ( 'NONE', #13348 ) ;
#16004 = CYLINDRICAL_SURFACE ( 'NONE', #17841, 120.5010000000000190 ) ;
#16005 = FACE_OUTER_BOUND ( 'NONE', #37396, .T. ) ;
#16006 = ORIENTED_EDGE ( 'NONE', *, *, #38657, .F. ) ;
#16007 = EDGE_CURVE ( 'NONE', #9120, #9695, #36004, .T. ) ;
#16008 = EDGE_CURVE ( 'NONE', #30643, #3236, #22834, .T. ) ;
#16009 = CARTESIAN_POINT ( 'NONE',  ( -4.929261580875707871, 40.00000000000000000, 37.46659216873931797 ) ) ;
#16010 = CARTESIAN_POINT ( 'NONE',  ( 23.59836588144746017, 40.00000000000000000, -26.81698947917456621 ) ) ;
#16011 = EDGE_CURVE ( 'NONE', #25635, #40989, #28402, .T. ) ;
#16012 = AXIS2_PLACEMENT_3D ( 'NONE', #1258, #34205, #27909 ) ;
#16013 = ORIENTED_EDGE ( 'NONE', *, *, #11175, .T. ) ;
#16014 = ORIENTED_EDGE ( 'NONE', *, *, #27431, .F. ) ;
#16015 = DIRECTION ( 'NONE',  ( -1.000000000000000000, -0.000000000000000000, -0.000000000000000000 ) ) ;
#16016 = CARTESIAN_POINT ( 'NONE',  ( 0.000000000000000000, -107.2703412112697094, 32.88383143828427535 ) ) ;
#16017 = AXIS2_PLACEMENT_3D ( 'NONE', #17348, #30625, #37361 ) ;
#16018 = VECTOR ( 'NONE', #957, 1000.000000000000000 ) ;
#16019 = LINE ( 'NONE', #39303, #28918 ) ;
#16020 = AXIS2_PLACEMENT_3D ( 'NONE', #20125, #6763, #414 ) ;
#16021 = DIRECTION ( 'NONE',  ( -1.000000000000000000, 0.000000000000000000, 0.000000000000000000 ) ) ;
#16022 = DIRECTION ( 'NONE',  ( -1.000000000000000000, -0.000000000000000000, -0.000000000000000000 ) ) ;
#16023 = ORIENTED_EDGE ( 'NONE', *, *, #32823, .T. ) ;
#16024 = DIRECTION ( 'NONE',  ( 1.000000000000000000, 0.000000000000000000, 0.000000000000000000 ) ) ;
#16025 = ORIENTED_EDGE ( 'NONE', *, *, #36626, .T. ) ;
#16026 = DIRECTION ( 'NONE',  ( -1.000000000000000000, -0.000000000000000000, -0.000000000000000000 ) ) ;
#16027 = DIRECTION ( 'NONE',  ( 0.000000000000000000, 0.9510565162951544194, -0.3090169943749447312 ) ) ;
#16028 = ADVANCED_FACE ( 'NONE', ( #13137 ), #26428, .T. ) ;
#16029 = DIRECTION ( 'NONE',  ( 0.000000000000000000, -0.3612416661871404866, -0.9324722294043605864 ) ) ;
#16030 = DIRECTION ( 'NONE',  ( 0.000000000000000000, 3.198947698072485022E-14, -1.000000000000000000 ) ) ;
#16031 = VERTEX_POINT ( 'NONE', #16853 ) ;
#16032 = FACE_OUTER_BOUND ( 'NONE', #38835, .T. ) ;
#16033 = VERTEX_POINT ( 'NONE', #19683 ) ;
#16034 = DIRECTION ( 'NONE',  ( -1.000000000000000000, -0.000000000000000000, -0.000000000000000000 ) ) ;
#16035 = ORIENTED_EDGE ( 'NONE', *, *, #36401, .T. ) ;
#16037 = ORIENTED_EDGE ( 'NONE', *, *, #11851, .F. ) ;
#16036 = CARTESIAN_POINT ( 'NONE',  ( 0.000000000000000000, 91.51415974874592507, 64.91094698989330425 ) ) ;
#16038 = CARTESIAN_POINT ( 'NONE',  ( 15.70068437845899290, 31.00000000000000355, 46.50252577710988078 ) ) ;
#16039 = ORIENTED_EDGE ( 'NONE', *, *, #35981, .F. ) ;
#16040 = DIRECTION ( 'NONE',  ( 1.000000000000000000, 0.000000000000000000, 0.000000000000000000 ) ) ;
#16041 = ORIENTED_EDGE ( 'NONE', *, *, #37947, .F. ) ;
#16042 = DIRECTION ( 'NONE',  ( -1.000000000000000000, -0.000000000000000000, 0.000000000000000000 ) ) ;
#16043 = ORIENTED_EDGE ( 'NONE', *, *, #31312, .F. ) ;
#16044 = CARTESIAN_POINT ( 'NONE',  ( -4.761419979751499554, 40.00000000000000000, -74.40007767863900767 ) ) ;
#16045 = AXIS2_PLACEMENT_3D ( 'NONE', #18895, #25421, #42586 ) ;
#16046 = CIRCLE ( 'NONE', #20960, 59.00000000000000000 ) ;
#16047 = CIRCLE ( 'NONE', #37597, 59.00000000000000711 ) ;
#16049 = LINE ( 'NONE', #29555, #35986 ) ;
#16048 = CARTESIAN_POINT ( 'NONE',  ( 0.000000000000000000, 31.81777574834305966, 10.70123563439457293 ) ) ;
#16050 = DIRECTION ( 'NONE',  ( 0.000000000000000000, 0.000000000000000000, 1.000000000000000000 ) ) ;
#16051 = ORIENTED_EDGE ( 'NONE', *, *, #10027, .F. ) ;
#16052 = CARTESIAN_POINT ( 'NONE',  ( 155.7547826636224499, -2.055254544495727309, 15.74958860255448734 ) ) ;
#16053 = ORIENTED_EDGE ( 'NONE', *, *, #10369, .T. ) ;
#16054 = DIRECTION ( 'NONE',  ( 0.000000000000000000, 0.000000000000000000, 1.000000000000000000 ) ) ;
#16055 = CARTESIAN_POINT ( 'NONE',  ( 8.999999999999998224, 91.65951123222482977, 71.09524597798119316 ) ) ;
#16056 = CARTESIAN_POINT ( 'NONE',  ( 65.81435062899562638, 31.00000000000000000, 37.99825742654716976 ) ) ;
#16058 = DIRECTION ( 'NONE',  ( 0.000000000000000000, 0.1062934856473589651, 0.9943348002101377592 ) ) ;
#16057 = DIRECTION ( 'NONE',  ( 0.000000000000000000, 0.000000000000000000, 1.000000000000000000 ) ) ;
#16059 = ORIENTED_EDGE ( 'NONE', *, *, #27178, .T. ) ;
#16060 = ADVANCED_FACE ( 'NONE', ( #3029 ), #30135, .F. ) ;
#16061 = DIRECTION ( 'NONE',  ( -1.000000000000000000, -0.000000000000000000, -0.000000000000000000 ) ) ;
#16062 = ORIENTED_EDGE ( 'NONE', *, *, #885, .T. ) ;
#16063 = CARTESIAN_POINT ( 'NONE',  ( 18.00000000000000355, -22.43957647427189528, 41.27978878573620847 ) ) ;
#16064 = DIRECTION ( 'NONE',  ( 1.000000000000000000, -0.000000000000000000, -0.000000000000000000 ) ) ;
#16065 = CARTESIAN_POINT ( 'NONE',  ( -80.50242771303932443, 31.00000000000000711, -46.62292012068298419 ) ) ;
#16066 = CARTESIAN_POINT ( 'NONE',  ( -6.638544827991895048, 40.00000000000000000, 99.59190654106264162 ) ) ;
#16067 = EDGE_CURVE ( 'NONE', #1664, #14989, #1886, .T. ) ;
#16068 = CARTESIAN_POINT ( 'NONE',  ( -31.75000000000000000, 18.77999999999999403, 0.000000000000000000 ) ) ;
#16069 = EDGE_CURVE ( 'NONE', #21133, #27409, #7459, .T. ) ;
#16070 = ORIENTED_EDGE ( 'NONE', *, *, #33144, .T. ) ;
#16071 = CARTESIAN_POINT ( 'NONE',  ( 18.00000000000000355, -47.22458491092822896, 5.098390039074067737 ) ) ;
#16072 = VERTEX_POINT ( 'NONE', #5904 ) ;
#16073 = CIRCLE ( 'NONE', #8388, 116.0000000000000000 ) ;
#16074 = FACE_OUTER_BOUND ( 'NONE', #28252, .T. ) ;
#16075 = CIRCLE ( 'NONE', #25828, 1.399999999999998579 ) ;
#16076 = ADVANCED_FACE ( 'NONE', ( #6338 ), #6538, .T. ) ;
#16077 = AXIS2_PLACEMENT_3D ( 'NONE', #32491, #5229, #38591 ) ;
#16078 = CARTESIAN_POINT ( 'NONE',  ( -105.0363123600777442, 31.00000000000000355, -2.692529638013756443 ) ) ;
#16079 = VECTOR ( 'NONE', #30973, 1000.000000000000000 ) ;
#16080 = CYLINDRICAL_SURFACE ( 'NONE', #1740, 36.00000000000000000 ) ;
#16081 = ORIENTED_EDGE ( 'NONE', *, *, #32483, .F. ) ;
#16082 = DIRECTION ( 'NONE',  ( 0.000000000000000000, -0.1590634960190788760, 0.9872683547213435551 ) ) ;
#16083 = DIRECTION ( 'NONE',  ( 0.000000000000000000, -1.000000000000000000, 1.224646799147353207E-16 ) ) ;
#16084 = CARTESIAN_POINT ( 'NONE',  ( 0.000000000000000000, 0.000000000000000000, 0.000000000000000000 ) ) ;
#16086 = ORIENTED_EDGE ( 'NONE', *, *, #17738, .T. ) ;
#16085 = DIRECTION ( 'NONE',  ( 0.000000000000000000, 0.000000000000000000, 1.000000000000000000 ) ) ;
#16087 = CARTESIAN_POINT ( 'NONE',  ( -11.85532105537472525, 31.00000000000000355, -20.54123584193516550 ) ) ;
#16088 = CARTESIAN_POINT ( 'NONE',  ( -9.000000000000005329, 0.000000000000000000, 0.000000000000000000 ) ) ;
#16089 = EDGE_CURVE ( 'NONE', #3149, #26591, #23178, .T. ) ;
#16091 = EDGE_LOOP ( 'NONE', ( #35619, #28006, #7905, #13751 ) ) ;
#16090 = DIRECTION ( 'NONE',  ( 0.000000000000000000, -0.8443279255020199603, 0.5358267949789887741 ) ) ;
#16092 = EDGE_LOOP ( 'NONE', ( #37684, #16436, #36258, #8637 ) ) ;
#16093 = CARTESIAN_POINT ( 'NONE',  ( 17.99999999999999645, -112.1702510623870239, -2.471285140323770335 ) ) ;
#16094 = EDGE_CURVE ( 'NONE', #41377, #6181, #38846, .T. ) ;
#16095 = DIRECTION ( 'NONE',  ( -1.000000000000000000, -0.000000000000000000, -0.000000000000000000 ) ) ;
#16096 = CARTESIAN_POINT ( 'NONE',  ( -39.38196478160931946, 40.00000000000000000, 13.29643045357694753 ) ) ;
#16097 = DIRECTION ( 'NONE',  ( -1.000000000000000000, 0.000000000000000000, 0.000000000000000000 ) ) ;
#16098 = AXIS2_PLACEMENT_3D ( 'NONE', #22090, #32285, #35747 ) ;
#16099 = CYLINDRICAL_SURFACE ( 'NONE', #43028, 13.40000000000000213 ) ;
#16100 = DIRECTION ( 'NONE',  ( 0.000000000000000000, 0.000000000000000000, 1.000000000000000000 ) ) ;
#16101 = AXIS2_PLACEMENT_3D ( 'NONE', #39185, #2947, #42032 ) ;
#16102 = ORIENTED_EDGE ( 'NONE', *, *, #16651, .T. ) ;
#16103 = CARTESIAN_POINT ( 'NONE',  ( 17.99999999999999645, -34.45183346761142928, 10.44371441202643247 ) ) ;
#16104 = VERTEX_POINT ( 'NONE', #24034 ) ;
#16105 = AXIS2_PLACEMENT_3D ( 'NONE', #24150, #10821, #30464 ) ;
#16106 = DIRECTION ( 'NONE',  ( 0.000000000000000000, 0.000000000000000000, 1.000000000000000000 ) ) ;
#16107 = CARTESIAN_POINT ( 'NONE',  ( 17.99999999999999645, 118.8387007424473580, -19.94628303336373065 ) ) ;
#16108 = AXIS2_PLACEMENT_3D ( 'NONE', #22182, #2884, #29132 ) ;
#16109 = CARTESIAN_POINT ( 'NONE',  ( -38.53741714288415210, 31.00000000000000355, -33.79371401777069650 ) ) ;
#16110 = CARTESIAN_POINT ( 'NONE',  ( 17.99999999999999645, -23.79363200506935527, -27.01597816121672224 ) ) ;
#16111 = ORIENTED_EDGE ( 'NONE', *, *, #19051, .F. ) ;
#16112 = CIRCLE ( 'NONE', #34900, 31.49900000000000588 ) ;
#16113 = FACE_OUTER_BOUND ( 'NONE', #894, .T. ) ;
#16114 = CARTESIAN_POINT ( 'NONE',  ( 41.30831894254264824, 31.00000000000000355, -83.80005689411834169 ) ) ;
#16115 = AXIS2_PLACEMENT_3D ( 'NONE', #16816, #40524, #36611 ) ;
#16116 = DIRECTION ( 'NONE',  ( -1.000000000000000000, -0.000000000000000000, 0.000000000000000000 ) ) ;
#16117 = ORIENTED_EDGE ( 'NONE', *, *, #21705, .T. ) ;
#16118 = CARTESIAN_POINT ( 'NONE',  ( 17.81064159971323946, 31.00000000000000355, 66.89829513328324140 ) ) ;
#16119 = CARTESIAN_POINT ( 'NONE',  ( -69.31868535678037802, 40.00000000000000711, 18.45717643660483986 ) ) ;
#16120 = CARTESIAN_POINT ( 'NONE',  ( -25.38139813252123034, 40.00000000000000000, 94.78629358389331117 ) ) ;
#16121 = EDGE_CURVE ( 'NONE', #4402, #39721, #30777, .T. ) ;
#16122 = ORIENTED_EDGE ( 'NONE', *, *, #27351, .F. ) ;
#16123 = CARTESIAN_POINT ( 'NONE',  ( 0.000000000000000000, 42.03146605346785947, 22.12489237027331512 ) ) ;
#16124 = DIRECTION ( 'NONE',  ( 0.000000000000000000, -1.000000000000000000, 5.297542245118643184E-16 ) ) ;
#16125 = DIRECTION ( 'NONE',  ( 0.3211947320043982423, 1.004009057038134257E-15, 0.9470131699890044219 ) ) ;
#16127 = EDGE_LOOP ( 'NONE', ( #17251, #906, #13288, #12693 ) ) ;
#16126 = CARTESIAN_POINT ( 'NONE',  ( 8.999999999999998224, 115.9387338813861419, 3.769613505536451026 ) ) ;
#16128 = DIRECTION ( 'NONE',  ( -1.000000000000000000, -0.000000000000000000, -0.000000000000000000 ) ) ;
#16129 = VECTOR ( 'NONE', #5128, 1000.000000000000000 ) ;
#16130 = CARTESIAN_POINT ( 'NONE',  ( 0.000000000000000000, -114.6488492393077081, -37.09625815500128709 ) ) ;
#16131 = CARTESIAN_POINT ( 'NONE',  ( 23.52215716829092074, 40.00000000000000000, -69.29398394448777765 ) ) ;
#16132 = LINE ( 'NONE', #10203, #11766 ) ;
#16133 = CIRCLE ( 'NONE', #11968, 31.49899999999999523 ) ;
#16134 = VECTOR ( 'NONE', #4517, 1000.000000000000000 ) ;
#16135 = EDGE_LOOP ( 'NONE', ( #36597, #27286 ) ) ;
#16136 = CARTESIAN_POINT ( 'NONE',  ( 146.1418929693599580, -2.055254544495727309, -53.89157828313137344 ) ) ;
#16137 = FACE_OUTER_BOUND ( 'NONE', #1253, .T. ) ;
#16138 = AXIS2_PLACEMENT_3D ( 'NONE', #8872, #20228, #3369 ) ;
#16139 = ORIENTED_EDGE ( 'NONE', *, *, #38151, .T. ) ;
#16140 = VERTEX_POINT ( 'NONE', #10696 ) ;
#16141 = FACE_BOUND ( 'NONE', #42568, .T. ) ;
#16143 = ORIENTED_EDGE ( 'NONE', *, *, #9643, .F. ) ;
#16142 = EDGE_CURVE ( 'NONE', #36864, #27480, #7849, .T. ) ;
#16144 = AXIS2_PLACEMENT_3D ( 'NONE', #7488, #37375, #493 ) ;
#16145 = DIRECTION ( 'NONE',  ( -1.000000000000000000, 0.000000000000000000, 0.000000000000000000 ) ) ;
#16146 = DIRECTION ( 'NONE',  ( 1.000000000000000000, -3.009274222672345096E-17, 0.000000000000000000 ) ) ;
#16147 = ADVANCED_FACE ( 'NONE', ( #17713 ), #37305, .F. ) ;
#16148 = CARTESIAN_POINT ( 'NONE',  ( 0.000000000000000000, 98.69720329640956891, 60.94966826379944536 ) ) ;
#16149 = CARTESIAN_POINT ( 'NONE',  ( 0.000000000000000000, 108.8880088604276608, 39.99251838045997687 ) ) ;
#16150 = ORIENTED_EDGE ( 'NONE', *, *, #10319, .T. ) ;
#16151 = DIRECTION ( 'NONE',  ( -1.000000000000000000, -0.000000000000000000, -0.000000000000000000 ) ) ;
#16152 = ORIENTED_EDGE ( 'NONE', *, *, #21157, .T. ) ;
#16153 = CIRCLE ( 'NONE', #5664, 47.49900000000000233 ) ;
#16154 = DIRECTION ( 'NONE',  ( 0.000000000000000000, 0.000000000000000000, 1.000000000000000000 ) ) ;
#16155 = VERTEX_POINT ( 'NONE', #34458 ) ;
#16156 = DIRECTION ( 'NONE',  ( -1.000000000000000000, -0.000000000000000000, 0.000000000000000000 ) ) ;
#16157 = DIRECTION ( 'NONE',  ( -1.000000000000000000, -0.000000000000000000, -0.000000000000000000 ) ) ;
#16158 = APPLICATION_PROTOCOL_DEFINITION ( 'draft international standard', 'automotive_design', 1998, #25675 ) ;
#16159 = ADVANCED_FACE ( 'NONE', ( #17289 ), #4568, .F. ) ;
#16160 = DIRECTION ( 'NONE',  ( -3.009274222672345096E-17, -1.000000000000000000, 2.455023325076454960E-18 ) ) ;
#16161 = CARTESIAN_POINT ( 'NONE',  ( -25.79802671946675474, 31.00000000000000355, 52.34090327860478453 ) ) ;
#16162 = CIRCLE ( 'NONE', #1493, 16.00000000000023448 ) ;
#16163 = DIRECTION ( 'NONE',  ( 0.000000000000000000, 0.000000000000000000, 1.000000000000000000 ) ) ;
#16164 = EDGE_CURVE ( 'NONE', #6044, #1782, #39521, .T. ) ;
#16165 = AXIS2_PLACEMENT_3D ( 'NONE', #38125, #14603, #31812 ) ;
#16166 = ORIENTED_EDGE ( 'NONE', *, *, #42085, .F. ) ;
#16167 = CARTESIAN_POINT ( 'NONE',  ( 11.33656872182281816, 31.00000000000000355, -33.21392199183605243 ) ) ;
#16168 = CIRCLE ( 'NONE', #12676, 13.59999999999999787 ) ;
#16169 = CARTESIAN_POINT ( 'NONE',  ( 55.63593431945896839, 39.99999999999999289, -48.80962981700470493 ) ) ;
#16170 = EDGE_CURVE ( 'NONE', #31963, #21287, #27049, .T. ) ;
#16171 = AXIS2_PLACEMENT_3D ( 'NONE', #33019, #29994, #22606 ) ;
#16172 = CARTESIAN_POINT ( 'NONE',  ( 0.000000000000000000, 45.78515115856043138, 12.64416602183680993 ) ) ;
#16173 = DIRECTION ( 'NONE',  ( -1.000000000000000000, 0.000000000000000000, 0.000000000000000000 ) ) ;
#16174 = ADVANCED_FACE ( 'NONE', ( #4128 ), #20998, .F. ) ;
#16175 = DIRECTION ( 'NONE',  ( -1.000000000000000000, 0.000000000000000000, -0.000000000000000000 ) ) ;
#16176 = DIRECTION ( 'NONE',  ( 0.000000000000000000, 0.000000000000000000, 1.000000000000000000 ) ) ;
#16177 = PRODUCT ( 'housing left', 'housing left', '', ( #1531 ) ) ;
#16178 = ORIENTED_EDGE ( 'NONE', *, *, #11244, .T. ) ;
#16179 = CARTESIAN_POINT ( 'NONE',  ( -36.61132647064156487, 40.00000000000000000, -18.04288060775211378 ) ) ;
#16180 = DIRECTION ( 'NONE',  ( 1.000000000000000000, 0.000000000000000000, 0.000000000000000000 ) ) ;
#16181 = FACE_OUTER_BOUND ( 'NONE', #36526, .T. ) ;
#16182 = ORIENTED_EDGE ( 'NONE', *, *, #24949, .F. ) ;
#16183 = DIRECTION ( 'NONE',  ( 1.000000000000000000, 0.000000000000000000, 0.000000000000000000 ) ) ;
#16184 = DIRECTION ( 'NONE',  ( -1.000000000000000000, -0.000000000000000000, -0.000000000000000000 ) ) ;
#16185 = ORIENTED_EDGE ( 'NONE', *, *, #5828, .F. ) ;
#16186 = LINE ( 'NONE', #16400, #41595 ) ;
#16187 = ORIENTED_EDGE ( 'NONE', *, *, #15494, .F. ) ;
#16188 = VERTEX_POINT ( 'NONE', #636 ) ;
#16189 = DIRECTION ( 'NONE',  ( -1.000000000000000000, 0.000000000000000000, 0.000000000000000000 ) ) ;
#16190 = VECTOR ( 'NONE', #19302, 1000.000000000000000 ) ;
#16191 = ADVANCED_FACE ( 'NONE', ( #7421 ), #34042, .F. ) ;
#16192 = CARTESIAN_POINT ( 'NONE',  ( -6.060882879309181348, 31.00000000000000355, -94.40013096059719544 ) ) ;
#16193 = ORIENTED_EDGE ( 'NONE', *, *, #27421, .F. ) ;
#16194 = DIRECTION ( 'NONE',  ( 0.000000000000000000, 0.000000000000000000, -1.000000000000000000 ) ) ;
#16195 = EDGE_CURVE ( 'NONE', #26550, #8083, #37451, .T. ) ;
#16196 = ADVANCED_FACE ( 'NONE', ( #34250 ), #41002, .T. ) ;
#16197 = EDGE_CURVE ( 'NONE', #13177, #12248, #38175, .T. ) ;
#16198 = CIRCLE ( 'NONE', #99, 59.00000000000001421 ) ;
#16199 = DIRECTION ( 'NONE',  ( -1.058513553088275437E-16, -1.000000000000000000, 8.813324511995299047E-17 ) ) ;
#16200 = CARTESIAN_POINT ( 'NONE',  ( -12.49999999999998401, -9.428438182424557364E-14, -40.00000000000000711 ) ) ;
#16201 = ORIENTED_EDGE ( 'NONE', *, *, #21611, .T. ) ;
#16202 = DIRECTION ( 'NONE',  ( 0.000000000000000000, 0.000000000000000000, 1.000000000000000000 ) ) ;
#16203 = CARTESIAN_POINT ( 'NONE',  ( -10.00000000000000000, 0.000000000000000000, 0.000000000000000000 ) ) ;
#16204 = LINE ( 'NONE', #36229, #38054 ) ;
#16206 = DIRECTION ( 'NONE',  ( -1.000000000000000000, 0.000000000000000000, -0.000000000000000000 ) ) ;
#16205 = DIRECTION ( 'NONE',  ( -1.000000000000000000, -0.000000000000000000, 0.000000000000000000 ) ) ;
#16207 = DIRECTION ( 'NONE',  ( -0.000000000000000000, 0.000000000000000000, -1.000000000000000000 ) ) ;
#16208 = ORIENTED_EDGE ( 'NONE', *, *, #9698, .F. ) ;
#16209 = CARTESIAN_POINT ( 'NONE',  ( 0.000000000000000000, 0.000000000000000000, 0.000000000000000000 ) ) ;
#16210 = CARTESIAN_POINT ( 'NONE',  ( -29.89583333557403222, 31.00000000000000355, 1.963495399902740690 ) ) ;
#16211 = VERTEX_POINT ( 'NONE', #40560 ) ;
#16212 = CARTESIAN_POINT ( 'NONE',  ( -91.96080130434583566, -2.055254544495720648, 14.45886780445738395 ) ) ;
#16213 = DIRECTION ( 'NONE',  ( 1.000000000000000000, 0.000000000000000000, 0.000000000000000000 ) ) ;
#16214 = VERTEX_POINT ( 'NONE', #14206 ) ;
#16215 = CARTESIAN_POINT ( 'NONE',  ( 0.000000000000000000, 22.82995208772688756, 41.06517797613672371 ) ) ;
#16216 = CARTESIAN_POINT ( 'NONE',  ( 26.55430347651023837, 40.00000000000000000, -34.62409890758566178 ) ) ;
#16217 = CARTESIAN_POINT ( 'NONE',  ( -22.00208165626150603, 40.00000000000000000, -25.16137218361809857 ) ) ;
#16218 = ADVANCED_FACE ( 'NONE', ( #40348 ), #40778, .F. ) ;
#16219 = AXIS2_PLACEMENT_3D ( 'NONE', #35700, #36138, #22665 ) ;
#16220 = VERTEX_POINT ( 'NONE', #10264 ) ;
#16221 = AXIS2_PLACEMENT_3D ( 'NONE', #21249, #41250, #11396 ) ;
#16222 = VERTEX_POINT ( 'NONE', #37526 ) ;
#16223 = DIRECTION ( 'NONE',  ( 1.000000000000000000, 0.000000000000000000, 0.000000000000000000 ) ) ;
#16224 = DIRECTION ( 'NONE',  ( 0.000000000000000000, 0.4817536741017102164, 0.8763066800438664705 ) ) ;
#16225 = ADVANCED_FACE ( 'NONE', ( #23614 ), #6981, .T. ) ;
#16226 = CIRCLE ( 'NONE', #24595, 0.08000000000000020983 ) ;
#16227 = LINE ( 'NONE', #19513, #30311 ) ;
#16228 = EDGE_CURVE ( 'NONE', #6410, #821, #33599, .T. ) ;
#16229 = FACE_OUTER_BOUND ( 'NONE', #5708, .T. ) ;
#16230 = CYLINDRICAL_SURFACE ( 'NONE', #13269, 59.00000000000000000 ) ;
#16231 = EDGE_LOOP ( 'NONE', ( #26276, #422, #19519, #9425 ) ) ;
#16232 = CARTESIAN_POINT ( 'NONE',  ( 0.000000000000000000, 0.000000000000000000, 0.000000000000000000 ) ) ;
#16233 = ORIENTED_EDGE ( 'NONE', *, *, #22519, .T. ) ;
#16234 = FACE_OUTER_BOUND ( 'NONE', #4762, .T. ) ;
#16235 = AXIS2_PLACEMENT_3D ( 'NONE', #27307, #40577, #24282 ) ;
#16236 = DIRECTION ( 'NONE',  ( 0.000000000000000000, -0.4610925014493144625, -0.8873520750565775383 ) ) ;
#16237 = CARTESIAN_POINT ( 'NONE',  ( 0.000000000000000000, 93.26762629039527042, -76.29967815892260319 ) ) ;
#16238 = DIRECTION ( 'NONE',  ( 1.000000000000000000, -1.058513553088275437E-16, 0.000000000000000000 ) ) ;
#16239 = VERTEX_POINT ( 'NONE', #41210 ) ;
#16240 = CARTESIAN_POINT ( 'NONE',  ( 0.000000000000000000, 0.000000000000000000, 0.000000000000000000 ) ) ;
#16241 = ORIENTED_EDGE ( 'NONE', *, *, #18892, .T. ) ;
#16242 = CARTESIAN_POINT ( 'NONE',  ( 17.99999999999999645, 0.000000000000000000, 0.000000000000000000 ) ) ;
#16243 = ORIENTED_EDGE ( 'NONE', *, *, #8607, .T. ) ;
#16245 = EDGE_LOOP ( 'NONE', ( #39533, #4424, #19124, #40822 ) ) ;
#16244 = DIRECTION ( 'NONE',  ( 1.000000000000000000, 0.000000000000000000, 0.000000000000000000 ) ) ;
#16246 = CARTESIAN_POINT ( 'NONE',  ( 45.08926718328532246, 31.00000000000000355, 51.56349680124436219 ) ) ;
#16247 = ORIENTED_EDGE ( 'NONE', *, *, #38354, .T. ) ;
#16248 = DIRECTION ( 'NONE',  ( 1.000000000000000000, 0.000000000000000000, 0.000000000000000000 ) ) ;
#16249 = EDGE_CURVE ( 'NONE', #41828, #33958, #18590, .T. ) ;
#16250 = EDGE_CURVE ( 'NONE', #29621, #31163, #18368, .T. ) ;
#16251 = EDGE_LOOP ( 'NONE', ( #28222, #27180, #27648, #1935 ) ) ;
#16252 = DIRECTION ( 'NONE',  ( -1.000000000000000000, 0.000000000000000000, 0.000000000000000000 ) ) ;
#16253 = EDGE_CURVE ( 'NONE', #20877, #14699, #1916, .T. ) ;
#16254 = VERTEX_POINT ( 'NONE', #11356 ) ;
#16255 = CIRCLE ( 'NONE', #42705, 116.0000000000000000 ) ;
#16256 = CARTESIAN_POINT ( 'NONE',  ( -54.99468034528496929, 40.00000000000000000, -62.86974495748533087 ) ) ;
#16258 = CARTESIAN_POINT ( 'NONE',  ( 0.000000000000000000, 3.803237743092368284, -31.26855263151010789 ) ) ;
#16257 = DIRECTION ( 'NONE',  ( 0.000000000000000000, 0.000000000000000000, 1.000000000000000000 ) ) ;
#16259 = ADVANCED_FACE ( 'NONE', ( #28596 ), #1725, .F. ) ;
#16260 = CARTESIAN_POINT ( 'NONE',  ( 0.000000000000000000, 99.97660604679964536, 67.26937820704921478 ) ) ;
#16261 = ORIENTED_EDGE ( 'NONE', *, *, #39576, .T. ) ;
#16262 = DIRECTION ( 'NONE',  ( -1.000000000000000000, 0.000000000000000000, -0.000000000000000000 ) ) ;
#16263 = EDGE_LOOP ( 'NONE', ( #23410, #41937, #25983, #13146 ) ) ;
#16264 = AXIS2_PLACEMENT_3D ( 'NONE', #39234, #22948, #39456 ) ;
#16265 = DIRECTION ( 'NONE',  ( -0.9396926207859138680, 0.000000000000000000, -0.3420201433256536139 ) ) ;
#16266 = DIRECTION ( 'NONE',  ( 1.000000000000000000, 0.000000000000000000, 0.000000000000000000 ) ) ;
#16267 = EDGE_CURVE ( 'NONE', #41658, #25259, #11807, .T. ) ;
#16268 = CARTESIAN_POINT ( 'NONE',  ( -77.84600223180727596, 31.00000000000000711, -20.84395318355897686 ) ) ;
#16270 = CARTESIAN_POINT ( 'NONE',  ( 0.000000000000000000, 6.486220790509957368, -112.0098273076986715 ) ) ;
#16269 = FACE_OUTER_BOUND ( 'NONE', #35696, .T. ) ;
#16271 = ORIENTED_EDGE ( 'NONE', *, *, #3005, .T. ) ;
#16272 = ORIENTED_EDGE ( 'NONE', *, *, #27875, .F. ) ;
#16273 = CARTESIAN_POINT ( 'NONE',  ( 0.000000000000000000, -117.6086855750632765, -26.24286718912224003 ) ) ;
#16274 = CYLINDRICAL_SURFACE ( 'NONE', #42233, 116.0000000000000000 ) ;
#16275 = CARTESIAN_POINT ( 'NONE',  ( -82.08563009789774867, 31.00000000000000711, 40.34115885382633593 ) ) ;
#16276 = CARTESIAN_POINT ( 'NONE',  ( 96.56285295106285105, 39.99999999999999289, 12.84127866192819312 ) ) ;
#16277 = AXIS2_PLACEMENT_3D ( 'NONE', #11166, #37109, #40581 ) ;
#16278 = DIRECTION ( 'NONE',  ( -1.000000000000000000, 0.000000000000000000, -0.000000000000000000 ) ) ;
#16279 = ADVANCED_FACE ( 'NONE', ( #5445 ), #41428, .T. ) ;
#16280 = FACE_OUTER_BOUND ( 'NONE', #15137, .T. ) ;
#16281 = ORIENTED_EDGE ( 'NONE', *, *, #4490, .T. ) ;
#16282 = LINE ( 'NONE', #39365, #36729 ) ;
#16283 = VERTEX_POINT ( 'NONE', #22066 ) ;
#16284 = DIRECTION ( 'NONE',  ( 1.000000000000000000, 0.000000000000000000, 0.000000000000000000 ) ) ;
#16285 = DIRECTION ( 'NONE',  ( 1.000000000000000000, -0.000000000000000000, -0.000000000000000000 ) ) ;
#16286 = DIRECTION ( 'NONE',  ( -1.000000000000000000, 3.942553354492743901E-17, 0.000000000000000000 ) ) ;
#16287 = ORIENTED_EDGE ( 'NONE', *, *, #14322, .T. ) ;
#16288 = DIRECTION ( 'NONE',  ( 1.000000000000000000, 0.000000000000000000, 0.000000000000000000 ) ) ;
#16289 = DIRECTION ( 'NONE',  ( 0.000000000000000000, 0.000000000000000000, 1.000000000000000000 ) ) ;
#16290 = DIRECTION ( 'NONE',  ( -1.000000000000000000, -0.000000000000000000, 0.000000000000000000 ) ) ;
#16291 = AXIS2_PLACEMENT_3D ( 'NONE', #23948, #13055, #20254 ) ;
#16293 = VERTEX_POINT ( 'NONE', #18807 ) ;
#16292 = CARTESIAN_POINT ( 'NONE',  ( 0.000000000000000000, 0.000000000000000000, 0.000000000000000000 ) ) ;
#16294 = CARTESIAN_POINT ( 'NONE',  ( 22.71825314374493487, 31.00000000000000355, -13.09499307598873585 ) ) ;
#16295 = DIRECTION ( 'NONE',  ( 1.000000000000000000, 0.000000000000000000, 0.000000000000000000 ) ) ;
#16296 = EDGE_CURVE ( 'NONE', #29484, #1556, #32062, .T. ) ;
#16297 = CIRCLE ( 'NONE', #33680, 59.00000000000000000 ) ;
#16299 = ORIENTED_EDGE ( 'NONE', *, *, #6856, .F. ) ;
#16298 = DIRECTION ( 'NONE',  ( 0.000000000000000000, 0.000000000000000000, 1.000000000000000000 ) ) ;
#16300 = ORIENTED_EDGE ( 'NONE', *, *, #43051, .T. ) ;
#16301 = CARTESIAN_POINT ( 'NONE',  ( 18.00000000000000355, 24.72041153920732981, 40.55929306992697292 ) ) ;
#16302 = CARTESIAN_POINT ( 'NONE',  ( 0.000000000000000000, 29.02167576844250618, -108.3790330702166926 ) ) ;
#16303 = CARTESIAN_POINT ( 'NONE',  ( -5.720710522143956034, 40.00000000000000000, -44.01410879001467436 ) ) ;
#16304 = CARTESIAN_POINT ( 'NONE',  ( 5.991979999999993645, 0.000000000000000000, 19.11697999999999809 ) ) ;
#16305 = VECTOR ( 'NONE', #21078, 999.9999999999998863 ) ;
#16306 = DIRECTION ( 'NONE',  ( -1.000000000000000000, 0.000000000000000000, -0.000000000000000000 ) ) ;
#16307 = CARTESIAN_POINT ( 'NONE',  ( 0.000000000000000000, 112.5120133921107737, 43.14554256761054063 ) ) ;
#16308 = ORIENTED_EDGE ( 'NONE', *, *, #35830, .F. ) ;
#16309 = CARTESIAN_POINT ( 'NONE',  ( 0.000000000000000000, 0.000000000000000000, 0.000000000000000000 ) ) ;
#16310 = EDGE_CURVE ( 'NONE', #39322, #34186, #10302, .T. ) ;
#16311 = ORIENTED_EDGE ( 'NONE', *, *, #15483, .T. ) ;
#16312 = CIRCLE ( 'NONE', #3733, 2.649999999999971934 ) ;
#16313 = DIRECTION ( 'NONE',  ( 0.000000000000000000, 0.000000000000000000, 1.000000000000000000 ) ) ;
#16314 = DIRECTION ( 'NONE',  ( -3.996523416598930318E-16, 2.658563593772947863E-15, 1.000000000000000000 ) ) ;
#16315 = ADVANCED_FACE ( 'NONE', ( #31430 ), #5221, .F. ) ;
#16316 = CARTESIAN_POINT ( 'NONE',  ( -38.92335646797288717, 31.00000000000000355, 29.86975225897632313 ) ) ;
#16317 = DIRECTION ( 'NONE',  ( 1.000000000000000000, 0.000000000000000000, 0.000000000000000000 ) ) ;
#16318 = ORIENTED_EDGE ( 'NONE', *, *, #21810, .F. ) ;
#16319 = DIRECTION ( 'NONE',  ( -1.847415842360817484E-16, 1.000000000000000000, 0.000000000000000000 ) ) ;
#16320 = CARTESIAN_POINT ( 'NONE',  ( 82.68608547523962216, 31.00000000000000000, 22.14036602612658200 ) ) ;
#16321 = AXIS2_PLACEMENT_3D ( 'NONE', #28302, #1641, #20688 ) ;
#16322 = FACE_OUTER_BOUND ( 'NONE', #42441, .T. ) ;
#16323 = ORIENTED_EDGE ( 'NONE', *, *, #15817, .T. ) ;
#16324 = CARTESIAN_POINT ( 'NONE',  ( -18.22940504111061344, 31.00000000000000355, 67.64968002090884625 ) ) ;
#16325 = CARTESIAN_POINT ( 'NONE',  ( 17.81064159970942384, 40.00000000000000000, 66.89829513328324140 ) ) ;
#16326 = CARTESIAN_POINT ( 'NONE',  ( -78.67873774631718220, 40.00000000000000711, 60.36924185307643143 ) ) ;
#16327 = VECTOR ( 'NONE', #27037, 1000.000000000000000 ) ;
#16328 = VERTEX_POINT ( 'NONE', #31214 ) ;
#16329 = EDGE_CURVE ( 'NONE', #27480, #39452, #6803, .T. ) ;
#16330 = DIRECTION ( 'NONE',  ( -1.000000000000000000, -0.000000000000000000, 0.000000000000000000 ) ) ;
#16331 = CARTESIAN_POINT ( 'NONE',  ( -10.00000000000000000, 0.000000000000000000, 0.000000000000000000 ) ) ;
#16332 = CARTESIAN_POINT ( 'NONE',  ( 17.99999999999999645, -111.9370513079666409, -44.61600100275288838 ) ) ;
#16333 = CIRCLE ( 'NONE', #972, 1.399999999999998579 ) ;
#16335 = ORIENTED_EDGE ( 'NONE', *, *, #1706, .F. ) ;
#16334 = CARTESIAN_POINT ( 'NONE',  ( 42.80287614962790599, -40.05525454449572464, 69.29271901957253021 ) ) ;
#16336 = CYLINDRICAL_SURFACE ( 'NONE', #41376, 11.00000000000023448 ) ;
#16337 = ORIENTED_EDGE ( 'NONE', *, *, #36514, .T. ) ;
#16338 = CARTESIAN_POINT ( 'NONE',  ( 4.203833317240879275, 1.627343821129582979, -3.597273115243889929 ) ) ;
#16339 = CIRCLE ( 'NONE', #27453, 58.99999999999999289 ) ;
#16340 = CARTESIAN_POINT ( 'NONE',  ( -25.13323546007955045, 40.00000000000000000, 74.03861446737784036 ) ) ;
#16341 = CARTESIAN_POINT ( 'NONE',  ( 0.000000000000000000, 35.72777019205667415, 106.3569410558018404 ) ) ;
#16342 = ORIENTED_EDGE ( 'NONE', *, *, #18809, .F. ) ;
#16343 = CARTESIAN_POINT ( 'NONE',  ( -105.9879088449591933, 17.11489954122026447, -0.3807199291576673361 ) ) ;
#16344 = DIRECTION ( 'NONE',  ( -1.000000000000000000, 0.000000000000000000, 0.000000000000000000 ) ) ;
#16345 = ORIENTED_EDGE ( 'NONE', *, *, #25056, .T. ) ;
#16346 = CARTESIAN_POINT ( 'NONE',  ( 0.000000000000000000, -3.840921266750155993, 47.34345070675168188 ) ) ;
#16347 = EDGE_CURVE ( 'NONE', #14447, #12013, #7494, .T. ) ;
#16348 = AXIS2_PLACEMENT_3D ( 'NONE', #17085, #13812, #30802 ) ;
#16349 = ORIENTED_EDGE ( 'NONE', *, *, #29266, .F. ) ;
#16350 = CARTESIAN_POINT ( 'NONE',  ( -132.0000507999999968, 0.000000000000000000, -11.00000000000000000 ) ) ;
#16351 = AXIS2_PLACEMENT_3D ( 'NONE', #1327, #4079, #20944 ) ;
#16352 = ORIENTED_EDGE ( 'NONE', *, *, #7898, .F. ) ;
#16353 = CARTESIAN_POINT ( 'NONE',  ( 0.000000000000000000, 6.486220790508443912, 112.0098273076987567 ) ) ;
#16354 = CARTESIAN_POINT ( 'NONE',  ( 0.000000000000000000, 36.06787431788676912, 37.45808914225499819 ) ) ;
#16355 = DIRECTION ( 'NONE',  ( -1.000000000000000000, 0.000000000000000000, 0.000000000000000000 ) ) ;
#16356 = CIRCLE ( 'NONE', #19862, 116.0000000000000000 ) ;
#16357 = DIRECTION ( 'NONE',  ( -1.000000000000000000, 0.000000000000000000, 0.000000000000000000 ) ) ;
#16359 = VERTEX_POINT ( 'NONE', #27955 ) ;
#16358 = AXIS2_PLACEMENT_3D ( 'NONE', #15463, #15264, #18967 ) ;
#16360 = CARTESIAN_POINT ( 'NONE',  ( 17.99999999999999645, 109.4038418350903470, 50.51029986767587587 ) ) ;
#16361 = EDGE_CURVE ( 'NONE', #27530, #3449, #11010, .T. ) ;
#16362 = AXIS2_PLACEMENT_3D ( 'NONE', #12655, #16596, #39226 ) ;
#16363 = EDGE_LOOP ( 'NONE', ( #38122, #30804, #10876, #33386 ) ) ;
#16364 = CIRCLE ( 'NONE', #34465, 51.99999999999999289 ) ;
#16365 = DIRECTION ( 'NONE',  ( -1.000000000000000000, -0.000000000000000000, -0.000000000000000000 ) ) ;
#16366 = ADVANCED_FACE ( 'NONE', ( #18160 ), #28159, .F. ) ;
#16367 = ORIENTED_EDGE ( 'NONE', *, *, #13436, .F. ) ;
#16368 = LINE ( 'NONE', #29674, #37813 ) ;
#16369 = AXIS2_PLACEMENT_3D ( 'NONE', #25888, #9060, #35460 ) ;
#16370 = ADVANCED_FACE ( 'NONE', ( #5013 ), #10408, .F. ) ;
#16371 = DIRECTION ( 'NONE',  ( 0.000000000000000000, -0.1590634960190789038, 0.9872683547213435551 ) ) ;
#16372 = CONTEXT_DEPENDENT_SHAPE_REPRESENTATION ( #20909, #13059 ) ;
#16374 = VECTOR ( 'NONE', #13719, 1000.000000000000000 ) ;
#16373 = CARTESIAN_POINT ( 'NONE',  ( 67.80287614962797704, -2.055254544495724645, 69.29271901957280022 ) ) ;
#16375 = CARTESIAN_POINT ( 'NONE',  ( -57.67632858778466698, 31.00000000000000711, 15.45560639130400205 ) ) ;
#16376 = VERTEX_POINT ( 'NONE', #23743 ) ;
#16377 = CARTESIAN_POINT ( 'NONE',  ( 2.511863649308172519, 31.00000000000000355, 39.39933062586388957 ) ) ;
#16378 = CARTESIAN_POINT ( 'NONE',  ( -23.19911330973958030, 40.00000000000000000, -68.30030121463531145 ) ) ;
#16379 = AXIS2_PLACEMENT_3D ( 'NONE', #30426, #24113, #269 ) ;
#16380 = ADVANCED_FACE ( 'NONE', ( #24180 ), #37866, .T. ) ;
#16381 = CARTESIAN_POINT ( 'NONE',  ( 0.000000000000000000, -110.3490479609633752, 20.28201389785361641 ) ) ;
#16382 = CARTESIAN_POINT ( 'NONE',  ( 17.99999999999999645, 68.61497464550731706, -99.05794392877534449 ) ) ;
#16383 = EDGE_CURVE ( 'NONE', #10188, #37671, #41629, .T. ) ;
#16384 = CIRCLE ( 'NONE', #8024, 13.59999999999999964 ) ;
#16385 = PLANE ( 'NONE',  #31621 ) ;
#16386 = CIRCLE ( 'NONE', #9415, 58.99999999999999289 ) ;
#16387 = CARTESIAN_POINT ( 'NONE',  ( 18.00000000000000355, 47.22458491092820765, 5.098390039074388369 ) ) ;
#16388 = VERTEX_POINT ( 'NONE', #14344 ) ;
#16389 = CARTESIAN_POINT ( 'NONE',  ( -21.36651465564686703, 40.00000000000000000, 43.35257367405362317 ) ) ;
#16390 = CARTESIAN_POINT ( 'NONE',  ( 17.99999999999999645, 0.000000000000000000, 0.000000000000000000 ) ) ;
#16391 = DIRECTION ( 'NONE',  ( 1.000000000000000000, 0.000000000000000000, 0.000000000000000000 ) ) ;
#16392 = AXIS2_PLACEMENT_3D ( 'NONE', #32682, #2762, #42692 ) ;
#16393 = EDGE_CURVE ( 'NONE', #34831, #14549, #571, .T. ) ;
#16394 = VERTEX_POINT ( 'NONE', #33737 ) ;
#16395 = AXIS2_PLACEMENT_3D ( 'NONE', #19922, #17076, #6998 ) ;
#16396 = CARTESIAN_POINT ( 'NONE',  ( 0.000000000000000000, 0.000000000000000000, 0.000000000000000000 ) ) ;
#16397 = LINE ( 'NONE', #188, #42390 ) ;
#16398 = AXIS2_PLACEMENT_3D ( 'NONE', #30058, #16979, #40042 ) ;
#16399 = VERTEX_POINT ( 'NONE', #17426 ) ;
#16400 = CARTESIAN_POINT ( 'NONE',  ( 9.000000000000001776, -51.85248208264520287, 3.914090171286016773 ) ) ;
#16401 = ORIENTED_EDGE ( 'NONE', *, *, #31966, .F. ) ;
#16402 = ADVANCED_FACE ( 'NONE', ( #34173 ), #4271, .F. ) ;
#16403 = AXIS2_PLACEMENT_3D ( 'NONE', #9286, #6014, #1883 ) ;
#16404 = VERTEX_POINT ( 'NONE', #23956 ) ;
#16405 = CARTESIAN_POINT ( 'NONE',  ( 2.500000000000000000, -2.357898499370432166, 3.035766082959412415E-15 ) ) ;
#16406 = CARTESIAN_POINT ( 'NONE',  ( -87.75478321338633236, 31.00000000000000711, -29.92102470462889130 ) ) ;
#16407 = VERTEX_POINT ( 'NONE', #27427 ) ;
#16408 = CARTESIAN_POINT ( 'NONE',  ( 17.99999999999999645, 6.854627147198713466, 115.7972974066013734 ) ) ;
#16409 = CARTESIAN_POINT ( 'NONE',  ( -15.99999999999997691, 17.11489954122026447, 5.571627607371296764E-15 ) ) ;
#16410 = DIRECTION ( 'NONE',  ( 0.000000000000000000, -0.5963673585385078635, 0.8027116379309587879 ) ) ;
#16411 = VERTEX_POINT ( 'NONE', #17642 ) ;
#16412 = CYLINDRICAL_SURFACE ( 'NONE', #37064, 47.49900000000000233 ) ;
#16413 = ADVANCED_FACE ( 'NONE', ( #10624 ), #7987, .T. ) ;
#16414 = AXIS2_PLACEMENT_3D ( 'NONE', #13160, #6362, #19287 ) ;
#16415 = DIRECTION ( 'NONE',  ( 0.000000000000000000, 0.000000000000000000, 1.000000000000000000 ) ) ;
#16416 = ADVANCED_FACE ( 'NONE', ( #7776 ), #7120, .F. ) ;
#16417 = AXIS2_PLACEMENT_3D ( 'NONE', #21564, #31543, #41561 ) ;
#16419 = CARTESIAN_POINT ( 'NONE',  ( 0.000000000000000000, 115.6826031496112392, 8.575274253897841703 ) ) ;
#16418 = DIRECTION ( 'NONE',  ( -1.000000000000000000, -0.000000000000000000, -0.000000000000000000 ) ) ;
#16420 = CARTESIAN_POINT ( 'NONE',  ( -79.93711883401132923, -12.05525454449572109, -145.8806300090334673 ) ) ;
#16421 = AXIS2_PLACEMENT_3D ( 'NONE', #37956, #34697, #4354 ) ;
#16422 = ORIENTED_EDGE ( 'NONE', *, *, #35589, .T. ) ;
#16423 = CIRCLE ( 'NONE', #23407, 59.00000000000000000 ) ;
#16424 = SURFACE_STYLE_USAGE ( .BOTH. , #39929 ) ;
#16425 = CARTESIAN_POINT ( 'NONE',  ( -15.87544005811639458, 31.00000000000000355, -27.47754625559162989 ) ) ;
#16426 = VERTEX_POINT ( 'NONE', #4482 ) ;
#16427 = CIRCLE ( 'NONE', #31745, 59.00000000000000711 ) ;
#16428 = DIRECTION ( 'NONE',  ( 1.000000000000000000, 0.000000000000000000, 0.000000000000000000 ) ) ;
#16429 = FACE_OUTER_BOUND ( 'NONE', #33776, .T. ) ;
#16430 = ORIENTED_EDGE ( 'NONE', *, *, #29509, .F. ) ;
#16431 = VECTOR ( 'NONE', #37393, 1000.000000000000000 ) ;
#16432 = CARTESIAN_POINT ( 'NONE',  ( -8.920000000000003482, 0.000000000000000000, 0.000000000000000000 ) ) ;
#16433 = CARTESIAN_POINT ( 'NONE',  ( -39.12533628356670334, 40.00000000000000000, -10.47265044290268499 ) ) ;
#16434 = CARTESIAN_POINT ( 'NONE',  ( -5.720710522143956034, 40.00000000000000000, -44.01410879001467436 ) ) ;
#16435 = CIRCLE ( 'NONE', #42868, 59.00000000000000711 ) ;
#16436 = ORIENTED_EDGE ( 'NONE', *, *, #27985, .T. ) ;
#16437 = EDGE_CURVE ( 'NONE', #17206, #4224, #18054, .T. ) ;
#16438 = ORIENTED_EDGE ( 'NONE', *, *, #34743, .F. ) ;
#16439 = FACE_OUTER_BOUND ( 'NONE', #15499, .T. ) ;
#16440 = EDGE_CURVE ( 'NONE', #19537, #24676, #40696, .T. ) ;
#16441 = EDGE_CURVE ( 'NONE', #20431, #38699, #24299, .T. ) ;
#16442 = EDGE_CURVE ( 'NONE', #18211, #41769, #27216, .T. ) ;
#16443 = DIRECTION ( 'NONE',  ( 0.000000000000000000, 0.000000000000000000, 1.000000000000000000 ) ) ;
#16444 = DIRECTION ( 'NONE',  ( 1.000000000000000000, -0.000000000000000000, -0.000000000000000000 ) ) ;
#16445 = DIRECTION ( 'NONE',  ( 0.000000000000000000, 0.000000000000000000, 1.000000000000000000 ) ) ;
#16446 = VERTEX_POINT ( 'NONE', #3823 ) ;
#16447 = DIRECTION ( 'NONE',  ( 0.000000000000000000, 0.9911528310040066403, 0.1327255272837255529 ) ) ;
#16448 = VERTEX_POINT ( 'NONE', #11281 ) ;
#16449 = DIRECTION ( 'NONE',  ( -1.000000000000000000, -0.000000000000000000, 0.000000000000000000 ) ) ;
#16450 = DIRECTION ( 'NONE',  ( -1.000000000000000000, -0.000000000000000000, 0.000000000000000000 ) ) ;
#16451 = ORIENTED_EDGE ( 'NONE', *, *, #41033, .T. ) ;
#16452 = VECTOR ( 'NONE', #34533, 1000.000000000000000 ) ;
#16453 = DIRECTION ( 'NONE',  ( -3.009274222672345096E-17, -1.000000000000000000, 2.455023325076454960E-18 ) ) ;
#16454 = CARTESIAN_POINT ( 'NONE',  ( 18.00000000000000355, -24.72041153920704204, -40.55929306992713634 ) ) ;
#16455 = EDGE_LOOP ( 'NONE', ( #35786, #23136 ) ) ;
#16456 = CARTESIAN_POINT ( 'NONE',  ( 17.99999999999999645, 13.22719389142019608, -28.58720592780581882 ) ) ;
#16457 = AXIS2_PLACEMENT_3D ( 'NONE', #28555, #41608, #38328 ) ;
#16458 = VERTEX_POINT ( 'NONE', #10847 ) ;
#16459 = CARTESIAN_POINT ( 'NONE',  ( 17.99999999999999645, 109.1131968883995000, 26.12628443612074847 ) ) ;
#16460 = CIRCLE ( 'NONE', #3850, 36.00000000000000000 ) ;
#16461 = ORIENTED_EDGE ( 'NONE', *, *, #16829, .T. ) ;
#16462 = CIRCLE ( 'NONE', #42204, 116.0000000000000000 ) ;
#16464 = VERTEX_POINT ( 'NONE', #24614 ) ;
#16463 = DIRECTION ( 'NONE',  ( -1.000000000000000000, 0.000000000000000000, 0.000000000000000000 ) ) ;
#16465 = CARTESIAN_POINT ( 'NONE',  ( 21.04585062970478759, 31.00000000000000355, -61.66509230325024049 ) ) ;
#16466 = AXIS2_PLACEMENT_3D ( 'NONE', #38501, #14993, #5359 ) ;
#16467 = ORIENTED_EDGE ( 'NONE', *, *, #2465, .F. ) ;
#16468 = CARTESIAN_POINT ( 'NONE',  ( 5.991980000000000750, 0.000000000000000000, 0.000000000000000000 ) ) ;
#16469 = CIRCLE ( 'NONE', #33131, 59.00000000000000000 ) ;
#16470 = CIRCLE ( 'NONE', #36633, 59.00000000000000000 ) ;
#16471 = VERTEX_POINT ( 'NONE', #21351 ) ;
#16472 = DIRECTION ( 'NONE',  ( 0.000000000000000000, -0.6382441836448261574, 0.7698339834299011697 ) ) ;
#16473 = CIRCLE ( 'NONE', #3177, 15.08402000000000065 ) ;
#16474 = EDGE_CURVE ( 'NONE', #31337, #40745, #34604, .T. ) ;
#16475 = ORIENTED_EDGE ( 'NONE', *, *, #301, .T. ) ;
#16476 = CARTESIAN_POINT ( 'NONE',  ( 78.79907178679739843, 39.99999999999999289, 38.97904116291323362 ) ) ;
#16477 = EDGE_CURVE ( 'NONE', #27385, #1786, #18086, .T. ) ;
#16479 = CARTESIAN_POINT ( 'NONE',  ( -102.4608013043457362, -35.35525454449571470, 14.45886780445633946 ) ) ;
#16478 = DIRECTION ( 'NONE',  ( -1.000000000000000000, 0.000000000000000000, 0.000000000000000000 ) ) ;
#16480 = LINE ( 'NONE', #15835, #8768 ) ;
#16481 = ORIENTED_EDGE ( 'NONE', *, *, #30150, .T. ) ;
#16482 = CARTESIAN_POINT ( 'NONE',  ( 17.99999999999999645, 80.74349901498408144, 77.90224541347306797 ) ) ;
#16483 = ORIENTED_EDGE ( 'NONE', *, *, #30083, .T. ) ;
#16484 = PRESENTATION_STYLE_ASSIGNMENT (( #29786 ) ) ;
#16485 = CYLINDRICAL_SURFACE ( 'NONE', #38543, 11.00000000000000000 ) ;
#16486 = DIRECTION ( 'NONE',  ( 0.000000000000000000, 0.000000000000000000, 1.000000000000000000 ) ) ;
#16487 = CARTESIAN_POINT ( 'NONE',  ( -79.69263343296167079, 31.00000000000000711, -10.49242979028127820 ) ) ;
#16489 = CARTESIAN_POINT ( 'NONE',  ( 0.000000000000000000, -110.1579703617967567, 21.29539948940213634 ) ) ;
#16488 = LINE ( 'NONE', #41453, #8672 ) ;
#16490 = CIRCLE ( 'NONE', #37348, 120.5010000000000332 ) ;
#16491 = VERTEX_POINT ( 'NONE', #1432 ) ;
#16492 = VECTOR ( 'NONE', #382, 1000.000000000000000 ) ;
#16493 = CIRCLE ( 'NONE', #22091, 2.649999999999985700 ) ;
#16494 = AXIS2_PLACEMENT_3D ( 'NONE', #17376, #37171, #16724 ) ;
#16495 = CARTESIAN_POINT ( 'NONE',  ( 18.00000000000000355, -44.75336757549789013, 14.30704879393590012 ) ) ;
#16496 = AXIS2_PLACEMENT_3D ( 'NONE', #2023, #28886, #38254 ) ;
#16497 = ADVANCED_FACE ( 'NONE', ( #27005 ), #40277, .T. ) ;
#16498 = ORIENTED_EDGE ( 'NONE', *, *, #14701, .F. ) ;
#16500 = AXIS2_PLACEMENT_3D ( 'NONE', #12290, #19703, #15780 ) ;
#16499 = CARTESIAN_POINT ( 'NONE',  ( 0.000000000000000000, 109.3506818544110217, 38.70953859161051014 ) ) ;
#16501 = FACE_OUTER_BOUND ( 'NONE', #8544, .T. ) ;
#16502 = ADVANCED_FACE ( 'NONE', ( #42206 ), #15633, .F. ) ;
#16503 = CARTESIAN_POINT ( 'NONE',  ( 76.36627019853398224, 31.00000000000000000, -58.43797548692494814 ) ) ;
#16504 = AXIS2_PLACEMENT_3D ( 'NONE', #18354, #28141, #21632 ) ;
#16505 = EDGE_CURVE ( 'NONE', #252, #10316, #2070, .T. ) ;
#16506 = EDGE_CURVE ( 'NONE', #19749, #16458, #15239, .T. ) ;
#16507 = CARTESIAN_POINT ( 'NONE',  ( 0.000000000000000000, 5.822172717930266472, 31.41458249383143198 ) ) ;
#16508 = EDGE_CURVE ( 'NONE', #42137, #1326, #39556, .T. ) ;
#16509 = AXIS2_PLACEMENT_3D ( 'NONE', #43145, #13294, #26592 ) ;
#16510 = FACE_OUTER_BOUND ( 'NONE', #37940, .T. ) ;
#16511 = ORIENTED_EDGE ( 'NONE', *, *, #39033, .T. ) ;
#16512 = FACE_OUTER_BOUND ( 'NONE', #11620, .T. ) ;
#16513 = ORIENTED_EDGE ( 'NONE', *, *, #33215, .F. ) ;
#16514 = CARTESIAN_POINT ( 'NONE',  ( 17.99999999999999645, 0.000000000000000000, 0.000000000000000000 ) ) ;
#16515 = DIRECTION ( 'NONE',  ( 0.000000000000000000, 0.3641605752528230266, -0.9313361774523380987 ) ) ;
#16516 = DIRECTION ( 'NONE',  ( 0.000000000000000000, 0.6845471059286847293, 0.7289686274214153272 ) ) ;
#16517 = ORIENTED_EDGE ( 'NONE', *, *, #18377, .F. ) ;
#16518 = CARTESIAN_POINT ( 'NONE',  ( 0.000000000000000000, -104.2166695095708349, -60.49278301857916063 ) ) ;
#16519 = DIRECTION ( 'NONE',  ( 1.000000000000000000, -0.000000000000000000, -0.000000000000000000 ) ) ;
#16520 = FACE_OUTER_BOUND ( 'NONE', #26963, .T. ) ;
#16522 = ORIENTED_EDGE ( 'NONE', *, *, #31324, .F. ) ;
#16521 = CYLINDRICAL_SURFACE ( 'NONE', #27098, 13.60000000000000142 ) ;
#16523 = CARTESIAN_POINT ( 'NONE',  ( -28.12618851199096781, 31.00000000000000355, 13.81902982503210708 ) ) ;
#16524 = CARTESIAN_POINT ( 'NONE',  ( 109.0695705685734254, 106.4195705685780524, 10.00000000000025224 ) ) ;
#16525 = CIRCLE ( 'NONE', #35997, 116.0000000000000000 ) ;
#16526 = CIRCLE ( 'NONE', #37283, 52.00000000000000000 ) ;
#16527 = AXIS2_PLACEMENT_3D ( 'NONE', #39946, #40166, #6165 ) ;
#16529 = VERTEX_POINT ( 'NONE', #31556 ) ;
#16528 = CARTESIAN_POINT ( 'NONE',  ( 9.000000000000001776, -115.9387338813861277, -3.769613505537241949 ) ) ;
#16530 = ORIENTED_EDGE ( 'NONE', *, *, #39694, .T. ) ;
#16531 = FACE_OUTER_BOUND ( 'NONE', #39297, .T. ) ;
#16532 = DIRECTION ( 'NONE',  ( 0.000000000000000000, 0.000000000000000000, 1.000000000000000000 ) ) ;
#16533 = CARTESIAN_POINT ( 'NONE',  ( -45.80426865613544862, 40.00000000000000000, -26.55377233850569141 ) ) ;
#16534 = CIRCLE ( 'NONE', #26980, 120.5010000000000332 ) ;
#16535 = DIRECTION ( 'NONE',  ( -1.000000000000000000, 0.000000000000000000, -0.000000000000000000 ) ) ;
#16536 = EDGE_CURVE ( 'NONE', #27165, #8980, #22218, .T. ) ;
#16537 = VECTOR ( 'NONE', #6913, 1000.000000000000000 ) ;
#16538 = CARTESIAN_POINT ( 'NONE',  ( 17.99999999999999645, 0.000000000000000000, 0.000000000000000000 ) ) ;
#16539 = CARTESIAN_POINT ( 'NONE',  ( 17.99999999999999645, -109.4038418350900059, -50.51029986767660773 ) ) ;
#16540 = VERTEX_POINT ( 'NONE', #12366 ) ;
#16541 = CARTESIAN_POINT ( 'NONE',  ( 18.00000000000000355, 0.000000000000000000, 0.000000000000000000 ) ) ;
#16543 = ORIENTED_EDGE ( 'NONE', *, *, #2752, .T. ) ;
#16542 = AXIS2_PLACEMENT_3D ( 'NONE', #11155, #21213, #24484 ) ;
#16544 = DIRECTION ( 'NONE',  ( 0.000000000000000000, 0.000000000000000000, 1.000000000000000000 ) ) ;
#16545 = DIRECTION ( 'NONE',  ( 0.000000000000000000, 0.7865515558026396903, 0.6175246149461955936 ) ) ;
#16546 = CIRCLE ( 'NONE', #5367, 59.00000000000001421 ) ;
#16547 = CARTESIAN_POINT ( 'NONE',  ( -46.94946386092573221, 31.00000000000000355, 15.94926099647653928 ) ) ;
#16548 = CARTESIAN_POINT ( 'NONE',  ( -99.91857577502598531, 40.00000000000000000, -1.280628618496984839 ) ) ;
#16549 = ORIENTED_EDGE ( 'NONE', *, *, #26610, .F. ) ;
#16550 = PRODUCT_DEFINITION_SHAPE ( 'NONE', 'NONE',  #4380 ) ;
#16551 = DIRECTION ( 'NONE',  ( -1.000000000000000000, 0.000000000000000000, -0.000000000000000000 ) ) ;
#16552 = ORIENTED_EDGE ( 'NONE', *, *, #15023, .T. ) ;
#16553 = CARTESIAN_POINT ( 'NONE',  ( -9.654069774896838041, 40.00000000000000000, -19.56573356436190636 ) ) ;
#16554 = ORIENTED_EDGE ( 'NONE', *, *, #7738, .F. ) ;
#16555 = CARTESIAN_POINT ( 'NONE',  ( -4.197393957002303999, -7.773935952363655451E-14, -3.503767560748929810 ) ) ;
#16557 = ORIENTED_EDGE ( 'NONE', *, *, #21778, .F. ) ;
#16556 = AXIS2_PLACEMENT_3D ( 'NONE', #30226, #13445, #27176 ) ;
#16558 = CARTESIAN_POINT ( 'NONE',  ( -31.81746463534672387, 31.00000000000000355, -55.29958784370775504 ) ) ;
#16559 = CARTESIAN_POINT ( 'NONE',  ( 64.47787635702036368, 39.99999999999999289, -17.16423577040998438 ) ) ;
#16560 = ADVANCED_FACE ( 'NONE', ( #21985 ), #5782, .F. ) ;
#16561 = EDGE_CURVE ( 'NONE', #2432, #37344, #5142, .T. ) ;
#16562 = CARTESIAN_POINT ( 'NONE',  ( -99.99999999999997158, 40.00000000000000711, 2.428179185498535730E-12 ) ) ;
#16563 = AXIS2_PLACEMENT_3D ( 'NONE', #31666, #5043, #15336 ) ;
#16564 = AXIS2_PLACEMENT_3D ( 'NONE', #34510, #10532, #7031 ) ;
#16565 = EDGE_CURVE ( 'NONE', #37962, #28053, #20816, .T. ) ;
#16566 = ORIENTED_EDGE ( 'NONE', *, *, #33381, .T. ) ;
#16567 = VERTEX_POINT ( 'NONE', #28732 ) ;
#16568 = AXIS2_PLACEMENT_3D ( 'NONE', #11739, #31998, #28320 ) ;
#16569 = CARTESIAN_POINT ( 'NONE',  ( 33.40854556226729954, -35.35525454449573601, -74.83297477053802993 ) ) ;
#16570 = AXIS2_PLACEMENT_3D ( 'NONE', #36758, #23712, #40240 ) ;
#16571 = CARTESIAN_POINT ( 'NONE',  ( 0.000000000000000000, -34.45183346761128718, -10.44371441202691564 ) ) ;
#16572 = CARTESIAN_POINT ( 'NONE',  ( 17.99999999999999645, 0.000000000000000000, 0.000000000000000000 ) ) ;
#16573 = AXIS2_PLACEMENT_3D ( 'NONE', #19784, #33048, #42218 ) ;
#16575 = ORIENTED_EDGE ( 'NONE', *, *, #24304, .F. ) ;
#16574 = DIRECTION ( 'NONE',  ( 1.000000000000000000, 0.000000000000000000, 0.000000000000000000 ) ) ;
#16576 = FACE_OUTER_BOUND ( 'NONE', #3420, .T. ) ;
#16577 = VERTEX_POINT ( 'NONE', #35462 ) ;
#16578 = CYLINDRICAL_SURFACE ( 'NONE', #38379, 116.0000000000000000 ) ;
#16579 = EDGE_CURVE ( 'NONE', #11572, #24177, #36793, .T. ) ;
#16580 = CARTESIAN_POINT ( 'NONE',  ( 48.66231590555653241, 39.99999999999999289, -55.48862040801123641 ) ) ;
#16581 = CARTESIAN_POINT ( 'NONE',  ( -12.50000000000000000, 1.530808498934191521E-15, -25.00000000000000000 ) ) ;
#16582 = AXIS2_PLACEMENT_3D ( 'NONE', #3337, #40625, #7489 ) ;
#16583 = ORIENTED_EDGE ( 'NONE', *, *, #14351, .F. ) ;
#16584 = EDGE_CURVE ( 'NONE', #27244, #4304, #18504, .T. ) ;
#16585 = CYLINDRICAL_SURFACE ( 'NONE', #16509, 59.00000000000000000 ) ;
#16586 = CYLINDRICAL_SURFACE ( 'NONE', #30116, 20.00000000000001066 ) ;
#16587 =( BOUNDED_SURFACE ( )  B_SPLINE_SURFACE ( 3, 2, ( 
 ( #31033, #11845, #4615 ),
 ( #35151, #11403, #25172 ),
 ( #34292, #1342, #14906 ),
 ( #24967, #27785, #41041 ),
 ( #38215, #11193, #4842 ),
 ( #37775, #38420, #34735 ) ),
 .UNSPECIFIED., .F., .F., .T. ) 
 B_SPLINE_SURFACE_WITH_KNOTS ( ( 4, 2, 4 ),
 ( 3, 3 ),
 ( 0.02032853247518125531, 0.02278863295364820865, 0.02524873343211516200 ),
 ( 0.000000000000000000, 1.000000000000000000 ),
 .UNSPECIFIED. ) 
 GEOMETRIC_REPRESENTATION_ITEM ( )  RATIONAL_B_SPLINE_SURFACE ( (
 ( 1.000000000000000000, 0.8047781615896836271, 1.000000000000000000),
 ( 1.000000000000000000, 0.8123767586289967202, 1.000000000000000000),
 ( 1.000000000000000000, 0.8190662415563443322, 1.000000000000000000),
 ( 1.000000000000000000, 0.8192361015669982205, 1.000000000000000000),
 ( 1.000000000000000000, 0.8126135807103181952, 1.000000000000000000),
 ( 1.000000000000000000, 0.8047712338318587788, 1.000000000000000000) ) ) 
 REPRESENTATION_ITEM ( '' )  SURFACE ( )  );
#16588 = ORIENTED_EDGE ( 'NONE', *, *, #10666, .T. ) ;
#16589 = ORIENTED_EDGE ( 'NONE', *, *, #12479, .F. ) ;
#16590 = CARTESIAN_POINT ( 'NONE',  ( -97.01392236320388918, -12.05525454449572109, 76.75426063221412676 ) ) ;
#16591 = ORIENTED_EDGE ( 'NONE', *, *, #4100, .T. ) ;
#16592 = CARTESIAN_POINT ( 'NONE',  ( -7.718844055051848230, 40.00000000000000000, -22.75659427661715384 ) ) ;
#16593 = CARTESIAN_POINT ( 'NONE',  ( 33.90854556226734218, -34.05525454449573175, -74.83297477053821467 ) ) ;
#16594 = CARTESIAN_POINT ( 'NONE',  ( 5.560781378645575757, 0.000000000000000000, -4.000000000000000000 ) ) ;
#16595 = VECTOR ( 'NONE', #5744, 1000.000000000000000 ) ;
#16596 = DIRECTION ( 'NONE',  ( 1.000000000000000000, 0.000000000000000000, 0.000000000000000000 ) ) ;
#16597 = ADVANCED_FACE ( 'NONE', ( #8218 ), #21578, .T. ) ;
#16598 = CARTESIAN_POINT ( 'NONE',  ( 18.00000000000000355, 32.32520163883584274, 34.09746168776050013 ) ) ;
#16599 = EDGE_LOOP ( 'NONE', ( #16672, #28839, #5720, #37028 ) ) ;
#16600 = VECTOR ( 'NONE', #22960, 1000.000000000000000 ) ;
#16601 = DIRECTION ( 'NONE',  ( 0.000000000000000000, 0.9510565162951544194, -0.3090169943749447867 ) ) ;
#16602 = VECTOR ( 'NONE', #15307, 1000.000000000000000 ) ;
#16603 = ORIENTED_EDGE ( 'NONE', *, *, #28532, .F. ) ;
#16604 = CIRCLE ( 'NONE', #19374, 58.99999999999998579 ) ;
#16605 = CIRCLE ( 'NONE', #9620, 23.00000000000000000 ) ;
#16606 = CARTESIAN_POINT ( 'NONE',  ( 17.99999999999999645, 31.80866420683990725, 16.59709355804141495 ) ) ;
#16607 = CARTESIAN_POINT ( 'NONE',  ( 18.00000000000000355, 0.000000000000000000, 0.000000000000000000 ) ) ;
#16608 = ORIENTED_EDGE ( 'NONE', *, *, #22930, .F. ) ;
#16609 = LINE ( 'NONE', #29902, #30175 ) ;
#16610 = AXIS2_PLACEMENT_3D ( 'NONE', #13607, #34083, #40175 ) ;
#16611 = DIRECTION ( 'NONE',  ( 0.000000000000000000, -1.152562038276115876E-14, -1.000000000000000000 ) ) ;
#16612 = PRODUCT_CONTEXT ( 'NONE', #39502, 'mechanical' ) ;
#16613 = CARTESIAN_POINT ( 'NONE',  ( 17.99999999999999645, -78.75547124681429523, 91.20343606296975736 ) ) ;
#16614 = CARTESIAN_POINT ( 'NONE',  ( 7.506055610550203205, 31.00000000000000355, 56.92102948000351148 ) ) ;
#16615 = VECTOR ( 'NONE', #37902, 1000.000000000000000 ) ;
#16616 = ORIENTED_EDGE ( 'NONE', *, *, #30450, .T. ) ;
#16617 = CARTESIAN_POINT ( 'NONE',  ( -16.82630558382797403, 31.00000000000000355, -29.24196894321154971 ) ) ;
#16618 = EDGE_CURVE ( 'NONE', #16033, #13299, #18734, .T. ) ;
#16619 = CARTESIAN_POINT ( 'NONE',  ( 9.510694223897102617, 40.00000000000000000, -72.24097909213479340 ) ) ;
#16620 = DIRECTION ( 'NONE',  ( 0.000000000000000000, 0.9407002666710319039, 0.3392388661180341658 ) ) ;
#16621 = FACE_OUTER_BOUND ( 'NONE', #5746, .T. ) ;
#16622 = CIRCLE ( 'NONE', #22926, 20.00000000000000711 ) ;
#16623 = EDGE_CURVE ( 'NONE', #41127, #28999, #28463, .T. ) ;
#16624 = DIRECTION ( 'NONE',  ( -3.009274222672345096E-17, -1.000000000000000000, 2.455023325076455345E-18 ) ) ;
#16625 = CARTESIAN_POINT ( 'NONE',  ( 9.000000000000000000, 29.09613215194512748, -21.19941258140292106 ) ) ;
#16626 = VECTOR ( 'NONE', #15699, 1000.000000000000000 ) ;
#16627 = EDGE_CURVE ( 'NONE', #36886, #21959, #1946, .T. ) ;
#16628 = VECTOR ( 'NONE', #7335, 1000.000000000000000 ) ;
#16629 = EDGE_LOOP ( 'NONE', ( #37865, #30082, #20609, #18365 ) ) ;
#16630 = CARTESIAN_POINT ( 'NONE',  ( 39.78947517253659072, 40.00000000000000000, -19.62497191778171413 ) ) ;
#16631 = AXIS2_PLACEMENT_3D ( 'NONE', #11871, #32553, #29296 ) ;
#16632 = DIRECTION ( 'NONE',  ( 3.996523416598930318E-16, -2.658563593772947863E-15, -1.000000000000000000 ) ) ;
#16633 = CARTESIAN_POINT ( 'NONE',  ( 17.99999999999999645, 54.09091620264857880, -102.6166301549512525 ) ) ;
#16634 = AXIS2_PLACEMENT_3D ( 'NONE', #33222, #32991, #39738 ) ;
#16635 = ORIENTED_EDGE ( 'NONE', *, *, #43076, .T. ) ;
#16636 = ADVANCED_FACE ( 'NONE', ( #12146 ), #19138, .T. ) ;
#16637 = LINE ( 'NONE', #39058, #28730 ) ;
#16638 = CIRCLE ( 'NONE', #33942, 10.99999999999998934 ) ;
#16639 = DIRECTION ( 'NONE',  ( -1.000000000000000000, -0.000000000000000000, 0.000000000000000000 ) ) ;
#16640 = ORIENTED_EDGE ( 'NONE', *, *, #29729, .F. ) ;
#16641 = CARTESIAN_POINT ( 'NONE',  ( 18.00000000000000355, 9.744342220504043084, -46.48873837489787064 ) ) ;
#16642 = ORIENTED_EDGE ( 'NONE', *, *, #15332, .T. ) ;
#16643 = VERTEX_POINT ( 'NONE', #11498 ) ;
#16644 = CARTESIAN_POINT ( 'NONE',  ( 17.99999999999999645, 0.000000000000000000, 0.000000000000000000 ) ) ;
#16645 = CARTESIAN_POINT ( 'NONE',  ( 93.52153384689862037, 31.00000000000000000, -24.92737483788710406 ) ) ;
#16646 = ORIENTED_EDGE ( 'NONE', *, *, #21960, .T. ) ;
#16647 = LINE ( 'NONE', #29934, #14055 ) ;
#16648 = CARTESIAN_POINT ( 'NONE',  ( 9.000000000000001776, -46.77034588191319386, 22.72740077717214291 ) ) ;
#16649 = DIRECTION ( 'NONE',  ( 1.000000000000000000, 0.000000000000000000, 0.000000000000000000 ) ) ;
#16650 = ORIENTED_EDGE ( 'NONE', *, *, #25649, .T. ) ;
#16651 = EDGE_CURVE ( 'NONE', #37143, #31287, #40271, .T. ) ;
#16652 = CARTESIAN_POINT ( 'NONE',  ( 0.000000000000000000, 114.1157422997283248, 20.82300072952973480 ) ) ;
#16653 = EDGE_CURVE ( 'NONE', #36927, #10297, #11042, .T. ) ;
#16654 = DIRECTION ( 'NONE',  ( -1.000000000000000000, -0.000000000000000000, -0.000000000000000000 ) ) ;
#16655 = EDGE_CURVE ( 'NONE', #39631, #30103, #33315, .T. ) ;
#16656 = VECTOR ( 'NONE', #18582, 1000.000000000000000 ) ;
#16658 = CARTESIAN_POINT ( 'NONE',  ( 0.000000000000000000, 15.21076497709875852, -119.5371223922153519 ) ) ;
#16657 = CARTESIAN_POINT ( 'NONE',  ( 18.00000000000000355, 49.65209126885784485, -15.44894276735498195 ) ) ;
#16659 = CARTESIAN_POINT ( 'NONE',  ( 0.000000000000000000, 75.03166794516801019, 94.29071961951534320 ) ) ;
#16660 = AXIS2_PLACEMENT_3D ( 'NONE', #17811, #31519, #31087 ) ;
#16661 = VERTEX_POINT ( 'NONE', #6216 ) ;
#16662 = CARTESIAN_POINT ( 'NONE',  ( -18.92511213055653130, 31.00000000000000355, 21.58621387822740090 ) ) ;
#16663 = ORIENTED_EDGE ( 'NONE', *, *, #17023, .F. ) ;
#16664 = DIRECTION ( 'NONE',  ( -1.000000000000000000, 0.000000000000000000, 0.000000000000000000 ) ) ;
#16665 = CARTESIAN_POINT ( 'NONE',  ( 17.99999999999999645, 11.58753559615527529, -29.77419532459249751 ) ) ;
#16666 = ORIENTED_EDGE ( 'NONE', *, *, #7767, .T. ) ;
#16667 = DIRECTION ( 'NONE',  ( 0.000000000000000000, 0.000000000000000000, 1.000000000000000000 ) ) ;
#16668 = CARTESIAN_POINT ( 'NONE',  ( 4.888094100070568437, 40.00000000000000000, 37.04995123692341252 ) ) ;
#16669 = EDGE_CURVE ( 'NONE', #16830, #10533, #14537, .T. ) ;
#16670 = CARTESIAN_POINT ( 'NONE',  ( 36.21668514975058173, 40.00000000000000000, 31.87730689759005287 ) ) ;
#16671 = VERTEX_POINT ( 'NONE', #64 ) ;
#16672 = ORIENTED_EDGE ( 'NONE', *, *, #39181, .F. ) ;
#16673 = CYLINDRICAL_SURFACE ( 'NONE', #24165, 19.19999999999999574 ) ;
#16674 = CARTESIAN_POINT ( 'NONE',  ( 17.99999999999999645, -100.6739960869721102, 49.52796165323228195 ) ) ;
#16675 = DIRECTION ( 'NONE',  ( 1.000000000000000000, 1.836909530733573776E-16, 0.000000000000000000 ) ) ;
#16676 = CARTESIAN_POINT ( 'NONE',  ( 17.99999999999999645, -72.00556975657760006, 86.04342158279364128 ) ) ;
#16677 = EDGE_CURVE ( 'NONE', #566, #18966, #34722, .T. ) ;
#16678 = CARTESIAN_POINT ( 'NONE',  ( 17.99999999999999645, -30.01658535635337444, 108.1077105353196970 ) ) ;
#16679 = VERTEX_POINT ( 'NONE', #16273 ) ;
#16680 = CARTESIAN_POINT ( 'NONE',  ( 17.99999999999999645, -30.71634675606060227, 8.790889055186445589 ) ) ;
#16681 = VERTEX_POINT ( 'NONE', #23480 ) ;
#16682 = CARTESIAN_POINT ( 'NONE',  ( 9.000000000000001776, 113.8630351447208824, -22.16324045874292636 ) ) ;
#16683 = DIRECTION ( 'NONE',  ( -1.000000000000000000, -0.000000000000000000, 0.000000000000000000 ) ) ;
#16684 = ORIENTED_EDGE ( 'NONE', *, *, #35697, .T. ) ;
#16685 = AXIS2_PLACEMENT_3D ( 'NONE', #18267, #14971, #18059 ) ;
#16686 = CIRCLE ( 'NONE', #22272, 47.49900000000000233 ) ;
#16687 = LINE ( 'NONE', #23660, #30529 ) ;
#16688 = CARTESIAN_POINT ( 'NONE',  ( 17.99999999999999645, 0.000000000000000000, 0.000000000000000000 ) ) ;
#16689 = ORIENTED_EDGE ( 'NONE', *, *, #12641, .F. ) ;
#16690 = DIRECTION ( 'NONE',  ( -1.000000000000000000, 0.000000000000000000, -0.000000000000000000 ) ) ;
#16691 = ORIENTED_EDGE ( 'NONE', *, *, #7648, .T. ) ;
#16692 = AXIS2_PLACEMENT_3D ( 'NONE', #4387, #17759, #17990 ) ;
#16693 = DIRECTION ( 'NONE',  ( 0.000000000000000000, -0.9213119778704086382, -0.3888241754733307021 ) ) ;
#16694 = ORIENTED_EDGE ( 'NONE', *, *, #8320, .T. ) ;
#16696 = ORIENTED_EDGE ( 'NONE', *, *, #17408, .F. ) ;
#16695 = DIRECTION ( 'NONE',  ( 1.000000000000000000, 0.000000000000000000, 0.000000000000000000 ) ) ;
#16697 = CARTESIAN_POINT ( 'NONE',  ( -47.50570208456527155, 31.00000000000000355, -41.80188021843024160 ) ) ;
#16698 = ORIENTED_EDGE ( 'NONE', *, *, #28737, .T. ) ;
#16699 = CARTESIAN_POINT ( 'NONE',  ( 0.000000000000000000, -111.9370513079672520, 44.61600100275137493 ) ) ;
#16700 = ORIENTED_EDGE ( 'NONE', *, *, #3878, .T. ) ;
#16701 = CARTESIAN_POINT ( 'NONE',  ( 21.00000000000000355, 0.000000000000000000, 2.055000000000000160 ) ) ;
#16702 = EDGE_LOOP ( 'NONE', ( #29126, #7811, #9758, #33442 ) ) ;
#16703 = CARTESIAN_POINT ( 'NONE',  ( -73.09555549758189841, 40.00000000000000711, 35.91380138263622257 ) ) ;
#16704 = EDGE_CURVE ( 'NONE', #24321, #39186, #9913, .T. ) ;
#16705 = EDGE_CURVE ( 'NONE', #1839, #25006, #41660, .T. ) ;
#16707 = DIRECTION ( 'NONE',  ( 0.000000000000000000, 0.000000000000000000, 1.000000000000000000 ) ) ;
#16706 = DIRECTION ( 'NONE',  ( 1.000000000000000000, -0.000000000000000000, -0.000000000000000000 ) ) ;
#16708 = DIRECTION ( 'NONE',  ( 0.000000000000000000, 0.000000000000000000, 1.000000000000000000 ) ) ;
#16709 = ORIENTED_EDGE ( 'NONE', *, *, #11179, .T. ) ;
#16710 = CARTESIAN_POINT ( 'NONE',  ( 0.000000000000000000, 0.000000000000000000, 0.000000000000000000 ) ) ;
#16711 = VERTEX_POINT ( 'NONE', #19559 ) ;
#16712 = DIRECTION ( 'NONE',  ( 0.000000000000000000, 0.000000000000000000, 1.000000000000000000 ) ) ;
#16713 = CARTESIAN_POINT ( 'NONE',  ( 18.89933391970155085, 31.00000000000000355, -70.58587736658564893 ) ) ;
#16714 = CIRCLE ( 'NONE', #10420, 59.00000000000002132 ) ;
#16716 = CARTESIAN_POINT ( 'NONE',  ( 42.80287614962790599, -12.05525454449572464, 69.29271901957253021 ) ) ;
#16715 = DIRECTION ( 'NONE',  ( -0.000000000000000000, -0.000000000000000000, 1.000000000000000000 ) ) ;
#16717 = CIRCLE ( 'NONE', #29248, 20.00000000000000355 ) ;
#16718 = VERTEX_POINT ( 'NONE', #39995 ) ;
#16719 = CIRCLE ( 'NONE', #1352, 2.799122904894268959 ) ;
#16720 = EDGE_CURVE ( 'NONE', #10939, #22195, #32622, .T. ) ;
#16721 = CARTESIAN_POINT ( 'NONE',  ( -22.10416666678001718, 40.00000000000000000, -1.441157586896875564 ) ) ;
#16722 = ORIENTED_EDGE ( 'NONE', *, *, #28640, .T. ) ;
#16723 = DIRECTION ( 'NONE',  ( 0.000000000000000000, 0.000000000000000000, 1.000000000000000000 ) ) ;
#16724 = DIRECTION ( 'NONE',  ( 0.000000000000000000, 0.000000000000000000, 1.000000000000000000 ) ) ;
#16725 = CARTESIAN_POINT ( 'NONE',  ( -96.33078216555148288, 31.00000000000000711, 32.58251675337926656 ) ) ;
#16726 = CARTESIAN_POINT ( 'NONE',  ( 0.000000000000000000, -46.11014828289851408, 9.022736828080542892 ) ) ;
#16727 = EDGE_CURVE ( 'NONE', #8913, #36864, #6678, .T. ) ;
#16728 = VERTEX_POINT ( 'NONE', #16499 ) ;
#16729 = CARTESIAN_POINT ( 'NONE',  ( 18.00000000000000355, 0.000000000000000000, 0.000000000000000000 ) ) ;
#16730 = VERTEX_POINT ( 'NONE', #23056 ) ;
#16731 = DIRECTION ( 'NONE',  ( -0.000000000000000000, -0.000000000000000000, -1.000000000000000000 ) ) ;
#16732 = EDGE_CURVE ( 'NONE', #37953, #21211, #29574, .T. ) ;
#16733 = DIRECTION ( 'NONE',  ( 1.000000000000000000, 0.000000000000000000, 0.000000000000000000 ) ) ;
#16734 = DIRECTION ( 'NONE',  ( -1.000000000000000000, -0.000000000000000000, -0.000000000000000000 ) ) ;
#16735 = ORIENTED_EDGE ( 'NONE', *, *, #36548, .F. ) ;
#16736 = VERTEX_POINT ( 'NONE', #22627 ) ;
#16737 = CARTESIAN_POINT ( 'NONE',  ( 0.000000000000000000, 0.000000000000000000, 0.000000000000000000 ) ) ;
#16738 = CARTESIAN_POINT ( 'NONE',  ( -10.00000000000000000, 0.000000000000000000, 0.000000000000000000 ) ) ;
#16739 = LINE ( 'NONE', #12590, #5505 ) ;
#16740 = AXIS2_PLACEMENT_3D ( 'NONE', #22578, #35820, #8582 ) ;
#16742 = VERTEX_POINT ( 'NONE', #6423 ) ;
#16741 = CARTESIAN_POINT ( 'NONE',  ( 17.99999999999999645, -24.22031524825905890, -109.5520369638039710 ) ) ;
#16743 = AXIS2_PLACEMENT_3D ( 'NONE', #31139, #11502, #21138 ) ;
#16744 = CARTESIAN_POINT ( 'NONE',  ( -18.66214908251421534, 31.00000000000000355, 24.25811346063288454 ) ) ;
#16745 = VECTOR ( 'NONE', #20556, 1000.000000000000000 ) ;
#16746 = DIRECTION ( 'NONE',  ( 0.000000000000000000, 0.000000000000000000, 1.000000000000000000 ) ) ;
#16747 = EDGE_CURVE ( 'NONE', #30532, #31353, #28307, .T. ) ;
#16749 = ORIENTED_EDGE ( 'NONE', *, *, #38185, .F. ) ;
#16748 = DIRECTION ( 'NONE',  ( -1.000000000000000000, -0.000000000000000000, -0.000000000000000000 ) ) ;
#16750 = EDGE_LOOP ( 'NONE', ( #30579, #38153 ) ) ;
#16751 = CYLINDRICAL_SURFACE ( 'NONE', #34460, 58.99999999999999289 ) ;
#16752 = FACE_OUTER_BOUND ( 'NONE', #40928, .T. ) ;
#16753 = CARTESIAN_POINT ( 'NONE',  ( 57.09498703527649610, 40.00000000000000000, 3.831922229401318880 ) ) ;
#16754 = FACE_OUTER_BOUND ( 'NONE', #41549, .T. ) ;
#16755 =( REPRESENTATION_RELATIONSHIP ('NONE','NONE', #330, #16840 ) REPRESENTATION_RELATIONSHIP_WITH_TRANSFORMATION ( #37702 )SHAPE_REPRESENTATION_RELATIONSHIP( ) );
#16756 = ADVANCED_FACE ( 'NONE', ( #29157 ), #39398, .F. ) ;
#16757 = EDGE_CURVE ( 'NONE', #30050, #34978, #17191, .T. ) ;
#16758 = CARTESIAN_POINT ( 'NONE',  ( -31.37281731866679024, 40.00000000000002842, 27.62913683693880174 ) ) ;
#16759 = EDGE_CURVE ( 'NONE', #20222, #2394, #41526, .T. ) ;
#16760 = EDGE_CURVE ( 'NONE', #13115, #41773, #15855, .T. ) ;
#16761 = CARTESIAN_POINT ( 'NONE',  ( 106.4195705685763471, -106.4195705685744855, 6.999999999999998224 ) ) ;
#16762 = VERTEX_POINT ( 'NONE', #25891 ) ;
#16763 = DIRECTION ( 'NONE',  ( 0.000000000000000000, 0.9618256431728180456, 0.2736629900720866648 ) ) ;
#16764 = ORIENTED_EDGE ( 'NONE', *, *, #12331, .T. ) ;
#16765 = CARTESIAN_POINT ( 'NONE',  ( 0.000000000000000000, 0.000000000000000000, 0.000000000000000000 ) ) ;
#16766 = CYLINDRICAL_SURFACE ( 'NONE', #375, 59.00000000000000000 ) ;
#16767 = CARTESIAN_POINT ( 'NONE',  ( 26.55430347651023837, 31.00000000000000355, -34.62409890758566178 ) ) ;
#16768 = CARTESIAN_POINT ( 'NONE',  ( -10.00000000000000000, 0.000000000000000000, 0.000000000000000000 ) ) ;
#16769 = ORIENTED_EDGE ( 'NONE', *, *, #11051, .T. ) ;
#16770 = DIRECTION ( 'NONE',  ( 0.000000000000000000, 0.000000000000000000, 1.000000000000000000 ) ) ;
#16771 = EDGE_LOOP ( 'NONE', ( #33350, #15204, #19256, #25798 ) ) ;
#16772 = CARTESIAN_POINT ( 'NONE',  ( -74.47060461443528823, 31.00000000000000711, 65.33029858165178894 ) ) ;
#16773 = CIRCLE ( 'NONE', #29991, 58.99999999999998579 ) ;
#16774 = AXIS2_PLACEMENT_3D ( 'NONE', #17176, #23502, #13672 ) ;
#16775 = ORIENTED_EDGE ( 'NONE', *, *, #24111, .F. ) ;
#16776 = AXIS2_PLACEMENT_3D ( 'NONE', #1732, #41006, #4573 ) ;
#16777 = DIRECTION ( 'NONE',  ( 3.009274222672345096E-17, 1.000000000000000000, -2.455023325076455345E-18 ) ) ;
#16778 = CARTESIAN_POINT ( 'NONE',  ( 9.885896071376816252, 31.00000000000000355, -74.20985814147174153 ) ) ;
#16779 = CARTESIAN_POINT ( 'NONE',  ( -9.616483412535155040, 40.00000000000000000, -73.82325415887568454 ) ) ;
#16780 = CIRCLE ( 'NONE', #24447, 13.59999999999999964 ) ;
#16781 = DIRECTION ( 'NONE',  ( -1.000000000000000000, -0.000000000000000000, 0.000000000000000000 ) ) ;
#16782 = ORIENTED_EDGE ( 'NONE', *, *, #15856, .T. ) ;
#16783 = ORIENTED_EDGE ( 'NONE', *, *, #18111, .T. ) ;
#16784 = CARTESIAN_POINT ( 'NONE',  ( 18.00000000000000355, -3.840921266750155993, 47.34345070675168188 ) ) ;
#16785 = CARTESIAN_POINT ( 'NONE',  ( -3.239593890920906993, -13.56862304811759223, -1.199999999999999956 ) ) ;
#16786 = CARTESIAN_POINT ( 'NONE',  ( 0.000000000000000000, -35.89808275599443022, -2.706964063997605141 ) ) ;
#16787 = EDGE_CURVE ( 'NONE', #29580, #3569, #12781, .T. ) ;
#16789 = EDGE_LOOP ( 'NONE', ( #41836, #9650, #7610, #34032 ) ) ;
#16788 = LINE ( 'NONE', #10422, #39454 ) ;
#16790 = FACE_OUTER_BOUND ( 'NONE', #7041, .T. ) ;
#16791 = ORIENTED_EDGE ( 'NONE', *, *, #2285, .F. ) ;
#16792 = CARTESIAN_POINT ( 'NONE',  ( 18.00000000000000355, 47.49120266317495265, 0.8606222198176843863 ) ) ;
#16793 = CARTESIAN_POINT ( 'NONE',  ( -79.69263343296167079, 40.00000000000000711, -10.49242979028127820 ) ) ;
#16794 = CARTESIAN_POINT ( 'NONE',  ( -10.00000000000000000, 0.000000000000000000, 0.000000000000000000 ) ) ;
#16795 = ORIENTED_EDGE ( 'NONE', *, *, #8495, .F. ) ;
#16796 = CIRCLE ( 'NONE', #26510, 11.00000000000000000 ) ;
#16797 = DIRECTION ( 'NONE',  ( 0.000000000000000000, 0.9957341762950348008, -0.09226835946329869920 ) ) ;
#16798 = DIRECTION ( 'NONE',  ( -1.000000000000000000, -0.000000000000000000, 0.000000000000000000 ) ) ;
#16799 = VERTEX_POINT ( 'NONE', #35870 ) ;
#16800 = CIRCLE ( 'NONE', #18905, 31.49900000000000588 ) ;
#16801 = ORIENTED_EDGE ( 'NONE', *, *, #12311, .F. ) ;
#16802 = CARTESIAN_POINT ( 'NONE',  ( 18.00000000000000355, -24.72041153920759982, 40.55929306992680949 ) ) ;
#16804 = ORIENTED_EDGE ( 'NONE', *, *, #19770, .F. ) ;
#16803 = CIRCLE ( 'NONE', #39720, 59.00000000000000711 ) ;
#16805 = CARTESIAN_POINT ( 'NONE',  ( -6.237032369604346371, 40.00000000000000000, -23.31551866006812901 ) ) ;
#16806 = DIRECTION ( 'NONE',  ( 0.000000000000000000, 0.5264321628773568351, -0.8502171357296134380 ) ) ;
#16807 = CIRCLE ( 'NONE', #4934, 15.00000000000000178 ) ;
#16808 = DIRECTION ( 'NONE',  ( 0.000000000000000000, 0.000000000000000000, 1.000000000000000000 ) ) ;
#16809 = AXIS2_PLACEMENT_3D ( 'NONE', #8021, #21165, #14605 ) ;
#16810 = CARTESIAN_POINT ( 'NONE',  ( 18.00000000000000355, 0.000000000000000000, 0.000000000000000000 ) ) ;
#16811 = EDGE_CURVE ( 'NONE', #12162, #31530, #6000, .T. ) ;
#16812 = EDGE_CURVE ( 'NONE', #39427, #1993, #5995, .T. ) ;
#16813 = AXIS2_PLACEMENT_3D ( 'NONE', #13082, #26379, #39645 ) ;
#16814 = CARTESIAN_POINT ( 'NONE',  ( 17.99999999999999645, 11.49545354908979888, -29.80986809967247453 ) ) ;
#16815 = ORIENTED_EDGE ( 'NONE', *, *, #13528, .T. ) ;
#16816 = CARTESIAN_POINT ( 'NONE',  ( 0.000000000000000000, 11.58753559615527529, -29.77419532459249751 ) ) ;
#16817 = EDGE_CURVE ( 'NONE', #7190, #20690, #11599, .T. ) ;
#16818 = VERTEX_POINT ( 'NONE', #16984 ) ;
#16819 = DIRECTION ( 'NONE',  ( 1.000000000000000000, 0.000000000000000000, 0.000000000000000000 ) ) ;
#16820 = DIRECTION ( 'NONE',  ( 1.000000000000000000, 0.000000000000000000, -0.000000000000000000 ) ) ;
#16821 = DIRECTION ( 'NONE',  ( -1.000000000000000000, 0.000000000000000000, 0.000000000000000000 ) ) ;
#16822 = EDGE_LOOP ( 'NONE', ( #12543, #35524, #15401, #14864 ) ) ;
#16823 = CARTESIAN_POINT ( 'NONE',  ( 17.99999999999999645, 28.35267316522815406, -22.18391138608678048 ) ) ;
#16824 = EDGE_CURVE ( 'NONE', #3775, #8700, #26568, .T. ) ;
#16825 = CARTESIAN_POINT ( 'NONE',  ( 0.000000000000000000, -112.5120133921110295, 43.14554256760978745 ) ) ;
#16826 = ITEM_DEFINED_TRANSFORMATION ( 'NONE', 'NONE', #18472,  #13552 ) ;
#16827 = CARTESIAN_POINT ( 'NONE',  ( -103.7695705685742240, -106.4195705685773135, 9.999999999999749534 ) ) ;
#16828 = CARTESIAN_POINT ( 'NONE',  ( 74.30822294231431613, 31.00000000000000000, -9.796771932235298408 ) ) ;
#16829 = EDGE_CURVE ( 'NONE', #32698, #37380, #8089, .T. ) ;
#16830 = VERTEX_POINT ( 'NONE', #7337 ) ;
#16831 = CARTESIAN_POINT ( 'NONE',  ( 4.597210615069569961, 31.00000000000000355, -34.47704375836577384 ) ) ;
#16832 = CARTESIAN_POINT ( 'NONE',  ( -26.42126989340051324, 40.00000000000000000, -77.78956226056263290 ) ) ;
#16833 = VECTOR ( 'NONE', #1419, 1000.000000000000000 ) ;
#16834 = CIRCLE ( 'NONE', #4966, 13.59999999999999787 ) ;
#16835 = LINE ( 'NONE', #20321, #37332 ) ;
#16836 = AXIS2_PLACEMENT_3D ( 'NONE', #18426, #4188, #7910 ) ;
#16837 = CARTESIAN_POINT ( 'NONE',  ( 2.027755760259328333E-13, -150.5000000000013642, 9.999999999999587885 ) ) ;
#16838 = AXIS2_PLACEMENT_3D ( 'NONE', #29177, #9512, #9288 ) ;
#16839 = ORIENTED_EDGE ( 'NONE', *, *, #41036, .T. ) ;
#16840 = SHAPE_REPRESENTATION ( 'circlip for shafts normal_din_Circlip DIN 471 - 22 x 1.2', ( #13552 ), #1623 ) ;
#16841 = DIRECTION ( 'NONE',  ( -1.000000000000000000, 0.000000000000000000, -0.000000000000000000 ) ) ;
#16842 = ADVANCED_FACE ( 'NONE', ( #27006 ), #36357, .T. ) ;
#16843 = DIRECTION ( 'NONE',  ( -3.009274222672345096E-17, -1.000000000000000000, 2.455023325076454960E-18 ) ) ;
#16844 = EDGE_LOOP ( 'NONE', ( #38319, #17839, #4685, #28738 ) ) ;
#16845 = CARTESIAN_POINT ( 'NONE',  ( 17.07784400123870938, 40.00000000000000000, -50.31546185293520779 ) ) ;
#16846 = DIRECTION ( 'NONE',  ( 0.000000000000000000, 0.3612416661871538093, -0.9324722294043554793 ) ) ;
#16847 = DIRECTION ( 'NONE',  ( 0.000000000000000000, 0.7164567402983115230, 0.6976315211349884970 ) ) ;
#16848 = ORIENTED_EDGE ( 'NONE', *, *, #130, .T. ) ;
#16849 = LINE ( 'NONE', #11144, #34266 ) ;
#16850 = CARTESIAN_POINT ( 'NONE',  ( -10.00000000000000000, 0.000000000000000000, 0.000000000000000000 ) ) ;
#16851 = AXIS2_PLACEMENT_3D ( 'NONE', #26242, #36031, #6156 ) ;
#16852 = ORIENTED_EDGE ( 'NONE', *, *, #23452, .F. ) ;
#16853 = CARTESIAN_POINT ( 'NONE',  ( 17.99999999999999645, -120.2856157092987388, 7.201503623196430226 ) ) ;
#16854 = ORIENTED_EDGE ( 'NONE', *, *, #4580, .T. ) ;
#16855 = CIRCLE ( 'NONE', #22434, 116.0000000000000000 ) ;
#16856 = ORIENTED_EDGE ( 'NONE', *, *, #4082, .F. ) ;
#16857 = CARTESIAN_POINT ( 'NONE',  ( 2.500000000000000000, -1.178949249685214307, 2.042000000000001592 ) ) ;
#16858 = CARTESIAN_POINT ( 'NONE',  ( -70.09526419939506070, 31.00000000000000711, -61.63891210113990837 ) ) ;
#16859 = ORIENTED_EDGE ( 'NONE', *, *, #1466, .F. ) ;
#16860 = CARTESIAN_POINT ( 'NONE',  ( 17.99999999999999645, 0.000000000000000000, 0.000000000000000000 ) ) ;
#16861 = DIRECTION ( 'NONE',  ( 0.000000000000000000, -0.4999999999999993339, 0.8660254037844390407 ) ) ;
#16862 = EDGE_CURVE ( 'NONE', #5549, #23636, #38724, .T. ) ;
#16863 = FACE_OUTER_BOUND ( 'NONE', #34501, .T. ) ;
#16864 = ORIENTED_EDGE ( 'NONE', *, *, #6289, .F. ) ;
#16865 = CARTESIAN_POINT ( 'NONE',  ( 0.000000000000000000, 0.000000000000000000, -25.00000000000000000 ) ) ;
#16866 = CIRCLE ( 'NONE', #11973, 120.5010000000000190 ) ;
#16867 = CARTESIAN_POINT ( 'NONE',  ( 17.99999999999999645, 0.000000000000000000, 0.000000000000000000 ) ) ;
#16869 = DIRECTION ( 'NONE',  ( -1.000000000000000000, 3.469446951953615421E-17, 0.000000000000000000 ) ) ;
#16868 = CARTESIAN_POINT ( 'NONE',  ( 8.919999999999999929, 1.356908653455267209E-15, -11.08000000000000007 ) ) ;
#16870 = EDGE_CURVE ( 'NONE', #3942, #15086, #20647, .T. ) ;
#16871 = AXIS2_PLACEMENT_3D ( 'NONE', #34138, #21542, #30876 ) ;
#16872 = LINE ( 'NONE', #209, #32565 ) ;
#16873 = EDGE_LOOP ( 'NONE', ( #6086, #6644, #14243, #39014 ) ) ;
#16874 = EDGE_CURVE ( 'NONE', #41968, #7568, #9963, .T. ) ;
#16875 = CARTESIAN_POINT ( 'NONE',  ( -25.53337963587170023, 31.00000000000000355, 29.12008199578403023 ) ) ;
#16876 = AXIS2_PLACEMENT_3D ( 'NONE', #33458, #17359, #20622 ) ;
#16877 = EDGE_LOOP ( 'NONE', ( #34000, #4655, #2450, #16928 ) ) ;
#16878 = DIRECTION ( 'NONE',  ( 0.000000000000000000, -0.5963673585384914322, -0.8027116379309711114 ) ) ;
#16879 = EDGE_CURVE ( 'NONE', #24620, #27149, #40107, .T. ) ;
#16880 = FACE_OUTER_BOUND ( 'NONE', #42399, .T. ) ;
#16881 = ORIENTED_EDGE ( 'NONE', *, *, #37959, .F. ) ;
#16882 = DIRECTION ( 'NONE',  ( -1.000000000000000000, 0.000000000000000000, -0.000000000000000000 ) ) ;
#16883 = CARTESIAN_POINT ( 'NONE',  ( 13.85568741775851542, 40.00000000000000000, -40.82620080729295609 ) ) ;
#16884 = CARTESIAN_POINT ( 'NONE',  ( 41.46880187714432253, 40.00000000000000000, 24.04226233541896107 ) ) ;
#16885 = ORIENTED_EDGE ( 'NONE', *, *, #36752, .F. ) ;
#16886 = CARTESIAN_POINT ( 'NONE',  ( -15.99999999999997691, 31.00000000000000355, 5.571627607371296764E-15 ) ) ;
#16887 = DIRECTION ( 'NONE',  ( 1.000000000000000000, 0.000000000000000000, 0.000000000000000000 ) ) ;
#16888 = LINE ( 'NONE', #20589, #37776 ) ;
#16889 = ORIENTED_EDGE ( 'NONE', *, *, #26192, .T. ) ;
#16890 = CARTESIAN_POINT ( 'NONE',  ( 23.79574588541966662, 40.00000000000000000, -6.380716493563439506 ) ) ;
#16891 = ORIENTED_EDGE ( 'NONE', *, *, #9634, .T. ) ;
#16892 = LINE ( 'NONE', #19, #8309 ) ;
#16894 = EDGE_CURVE ( 'NONE', #21531, #11261, #29013, .T. ) ;
#16893 = AXIS2_PLACEMENT_3D ( 'NONE', #7861, #5022, #21219 ) ;
#16895 = CYLINDRICAL_SURFACE ( 'NONE', #16610, 36.00000000000000000 ) ;
#16896 = CIRCLE ( 'NONE', #7067, 20.00000000000000355 ) ;
#16897 = EDGE_LOOP ( 'NONE', ( #9781, #676, #36067, #21454 ) ) ;
#16898 = LINE ( 'NONE', #39956, #24260 ) ;
#16899 = CIRCLE ( 'NONE', #24567, 47.49900000000000233 ) ;
#16900 = FACE_OUTER_BOUND ( 'NONE', #31050, .T. ) ;
#16901 = ORIENTED_EDGE ( 'NONE', *, *, #10236, .T. ) ;
#16902 = CARTESIAN_POINT ( 'NONE',  ( -100.0000000000000568, 40.00000000000000000, 2.687954026026062593E-12 ) ) ;
#16903 = ORIENTED_EDGE ( 'NONE', *, *, #32355, .F. ) ;
#16904 = DIRECTION ( 'NONE',  ( 1.000000000000000000, 0.000000000000000000, -6.546126324440832913E-16 ) ) ;
#16905 = VECTOR ( 'NONE', #12713, 1000.000000000000000 ) ;
#16906 = ORIENTED_EDGE ( 'NONE', *, *, #35064, .F. ) ;
#16908 = ORIENTED_EDGE ( 'NONE', *, *, #30506, .F. ) ;
#16907 = DIRECTION ( 'NONE',  ( 0.000000000000000000, 0.000000000000000000, 1.000000000000000000 ) ) ;
#16909 = CARTESIAN_POINT ( 'NONE',  ( 54.03410584561684260, 31.00000000000000355, 41.58544482236945328 ) ) ;
#16910 = ORIENTED_EDGE ( 'NONE', *, *, #4100, .F. ) ;
#16911 = DIRECTION ( 'NONE',  ( -1.000000000000000000, 0.000000000000000000, 0.000000000000000000 ) ) ;
#16912 = EDGE_CURVE ( 'NONE', #9577, #9442, #13274, .T. ) ;
#16913 = VERTEX_POINT ( 'NONE', #20055 ) ;
#16914 = CYLINDRICAL_SURFACE ( 'NONE', #29393, 36.00000000000000000 ) ;
#16915 = ORIENTED_EDGE ( 'NONE', *, *, #29664, .T. ) ;
#16916 = CARTESIAN_POINT ( 'NONE',  ( 87.09251733236553150, 39.99999999999999289, 5.815661930448016825 ) ) ;
#16918 = CARTESIAN_POINT ( 'NONE',  ( 0.000000000000000000, 84.62908780824871258, 85.78116633471321961 ) ) ;
#16917 = CARTESIAN_POINT ( 'NONE',  ( -150.5000000000000284, -5.254679414958916394E-13, 9.999999999999998224 ) ) ;
#16919 = CARTESIAN_POINT ( 'NONE',  ( 0.000000000000000000, 0.000000000000000000, 0.000000000000000000 ) ) ;
#16920 = ORIENTED_EDGE ( 'NONE', *, *, #5442, .F. ) ;
#16921 = DIRECTION ( 'NONE',  ( -1.000000000000000000, -0.000000000000000000, -0.000000000000000000 ) ) ;
#16922 = ORIENTED_EDGE ( 'NONE', *, *, #8683, .T. ) ;
#16923 = ADVANCED_FACE ( 'NONE', ( #30492 ), #3180, .T. ) ;
#16924 = CIRCLE ( 'NONE', #29421, 52.00000000000000000 ) ;
#16925 = CARTESIAN_POINT ( 'NONE',  ( 0.000000000000000000, -79.94368240339366594, -90.16373242487986772 ) ) ;
#16926 = CARTESIAN_POINT ( 'NONE',  ( -28.35539204363714205, 31.00000000000000355, 83.52787551312086123 ) ) ;
#16927 = CARTESIAN_POINT ( 'NONE',  ( 0.000000000000000000, 11.41303419185120482, -111.6154788735834700 ) ) ;
#16928 = ORIENTED_EDGE ( 'NONE', *, *, #6160, .T. ) ;
#16929 = AXIS2_PLACEMENT_3D ( 'NONE', #23767, #37037, #7143 ) ;
#16930 = EDGE_CURVE ( 'NONE', #36754, #34450, #2486, .T. ) ;
#16931 = CARTESIAN_POINT ( 'NONE',  ( 0.000000000000000000, -29.03409033315590904, 12.21509719675380623 ) ) ;
#16932 = AXIS2_PLACEMENT_3D ( 'NONE', #3924, #30589, #20798 ) ;
#16933 = ORIENTED_EDGE ( 'NONE', *, *, #1222, .F. ) ;
#16934 = LINE ( 'NONE', #33683, #29017 ) ;
#16935 = CARTESIAN_POINT ( 'NONE',  ( 18.00000000000000355, 7.162210897275733679, 51.50439529848829068 ) ) ;
#16936 = LINE ( 'NONE', #939, #31752 ) ;
#16937 = CARTESIAN_POINT ( 'NONE',  ( 0.000000000000000000, -44.25018368420762016, 27.31155879685165999 ) ) ;
#16938 = ORIENTED_EDGE ( 'NONE', *, *, #34577, .F. ) ;
#16939 = DIRECTION ( 'NONE',  ( -1.000000000000000000, 0.000000000000000000, 0.000000000000000000 ) ) ;
#16940 = ORIENTED_EDGE ( 'NONE', *, *, #30810, .F. ) ;
#16941 = EDGE_CURVE ( 'NONE', #24177, #10039, #40487, .T. ) ;
#16942 = LINE ( 'NONE', #30225, #20037 ) ;
#16943 = EDGE_CURVE ( 'NONE', #6569, #6210, #20990, .T. ) ;
#16944 = DIRECTION ( 'NONE',  ( -1.000000000000000000, 0.000000000000000000, 0.000000000000000000 ) ) ;
#16945 = CARTESIAN_POINT ( 'NONE',  ( 17.99999999999999645, 115.9387338813862129, -3.769613505534868736 ) ) ;
#16946 = VERTEX_POINT ( 'NONE', #30065 ) ;
#16947 = ORIENTED_EDGE ( 'NONE', *, *, #31292, .T. ) ;
#16948 = DIRECTION ( 'NONE',  ( 1.000000000000000000, -0.000000000000000000, -0.000000000000000000 ) ) ;
#16949 = CARTESIAN_POINT ( 'NONE',  ( -7.000000000000002665, 19.59999999999999787, 0.000000000000000000 ) ) ;
#16950 = CIRCLE ( 'NONE', #3654, 59.00000000000002132 ) ;
#16951 = DIRECTION ( 'NONE',  ( 1.000000000000000000, 0.000000000000000000, 0.000000000000000000 ) ) ;
#16953 = ORIENTED_EDGE ( 'NONE', *, *, #28347, .F. ) ;
#16952 = DIRECTION ( 'NONE',  ( -1.000000000000000000, 0.000000000000000000, -0.000000000000000000 ) ) ;
#16954 = CARTESIAN_POINT ( 'NONE',  ( -30.84436395684956977, 31.00000000000000355, -10.52363363425319243 ) ) ;
#16955 = DIRECTION ( 'NONE',  ( 2.731800627175558911E-17, 1.000000000000000000, -3.170996607629411740E-18 ) ) ;
#16956 = VECTOR ( 'NONE', #6445, 1000.000000000000000 ) ;
#16957 = EDGE_CURVE ( 'NONE', #39148, #2987, #20476, .T. ) ;
#16959 = ORIENTED_EDGE ( 'NONE', *, *, #17722, .F. ) ;
#16958 = DIRECTION ( 'NONE',  ( -1.000000000000000000, 0.000000000000000000, -0.000000000000000000 ) ) ;
#16960 = VERTEX_POINT ( 'NONE', #29861 ) ;
#16961 = LINE ( 'NONE', #28227, #19889 ) ;
#16962 = PLANE ( 'NONE',  #20350 ) ;
#16964 = CARTESIAN_POINT ( 'NONE',  ( -47.35250803175856049, 40.00000000000000000, -23.44639516808875257 ) ) ;
#16963 = AXIS2_PLACEMENT_3D ( 'NONE', #30748, #13752, #10665 ) ;
#16965 = DIRECTION ( 'NONE',  ( -1.000000000000000000, 0.000000000000000000, 0.000000000000000000 ) ) ;
#16966 = UNCERTAINTY_MEASURE_WITH_UNIT (LENGTH_MEASURE( 1.000000000000000082E-05 ), #5131, 'distance_accuracy_value', 'NONE');
#16967 = DIRECTION ( 'NONE',  ( 1.000000000000000000, 0.000000000000000000, 0.000000000000000000 ) ) ;
#16968 = VERTEX_POINT ( 'NONE', #17208 ) ;
#16969 = DIRECTION ( 'NONE',  ( 0.000000000000000000, -0.9714298932647074114, -0.2373266998711251186 ) ) ;
#16970 = ORIENTED_EDGE ( 'NONE', *, *, #26448, .F. ) ;
#16971 = EDGE_CURVE ( 'NONE', #15422, #18374, #118, .T. ) ;
#16972 = CARTESIAN_POINT ( 'NONE',  ( 0.000000000000000000, 111.2559044912529345, -32.83479428644565701 ) ) ;
#16973 = FACE_OUTER_BOUND ( 'NONE', #7844, .T. ) ;
#16974 = EDGE_CURVE ( 'NONE', #10211, #20449, #19272, .T. ) ;
#16975 = CARTESIAN_POINT ( 'NONE',  ( 15.14372185054182651, 31.00000000000000355, 44.57714859939663654 ) ) ;
#16976 = FACE_OUTER_BOUND ( 'NONE', #39656, .T. ) ;
#16977 = ORIENTED_EDGE ( 'NONE', *, *, #42044, .T. ) ;
#16978 = ADVANCED_FACE ( 'NONE', ( #6904 ), #3614, .F. ) ;
#16979 = DIRECTION ( 'NONE',  ( 1.000000000000000000, 0.000000000000000000, 0.000000000000000000 ) ) ;
#16980 = ORIENTED_EDGE ( 'NONE', *, *, #28352, .F. ) ;
#16981 = AXIS2_PLACEMENT_3D ( 'NONE', #32817, #39139, #5770 ) ;
#16982 = CARTESIAN_POINT ( 'NONE',  ( -43.52407497442469264, 31.00000000000000355, 88.29422169633753015 ) ) ;
#16983 = ORIENTED_EDGE ( 'NONE', *, *, #1847, .F. ) ;
#16984 = CARTESIAN_POINT ( 'NONE',  ( 17.99999999999999645, 116.0452958106484971, -32.46506308663343532 ) ) ;
#16985 = CARTESIAN_POINT ( 'NONE',  ( 20.39742982868580157, 31.00000000000000355, 76.57971376064386959 ) ) ;
#16986 = CARTESIAN_POINT ( 'NONE',  ( 39.32569335900156915, 40.00000000000000000, 68.32161714264680086 ) ) ;
#16987 = DIRECTION ( 'NONE',  ( 0.000000000000000000, 0.000000000000000000, 1.000000000000000000 ) ) ;
#16988 = VERTEX_POINT ( 'NONE', #17860 ) ;
#16989 = ORIENTED_EDGE ( 'NONE', *, *, #37793, .T. ) ;
#16990 = AXIS2_PLACEMENT_3D ( 'NONE', #35294, #22897, #22257 ) ;
#16991 = DIRECTION ( 'NONE',  ( -1.000000000000000000, -0.000000000000000000, 0.000000000000000000 ) ) ;
#16992 = EDGE_CURVE ( 'NONE', #41473, #24259, #16460, .T. ) ;
#16993 = FACE_OUTER_BOUND ( 'NONE', #20136, .T. ) ;
#16994 = EDGE_CURVE ( 'NONE', #13070, #14175, #11499, .T. ) ;
#16995 = EDGE_CURVE ( 'NONE', #21974, #26598, #13686, .T. ) ;
#16996 = EDGE_CURVE ( 'NONE', #20507, #25590, #34175, .T. ) ;
#16998 = ORIENTED_EDGE ( 'NONE', *, *, #29129, .F. ) ;
#16997 = LINE ( 'NONE', #30921, #24928 ) ;
#16999 = DIRECTION ( 'NONE',  ( 1.000000000000000000, 0.000000000000000000, 0.000000000000000000 ) ) ;
#17000 = ORIENTED_EDGE ( 'NONE', *, *, #28095, .T. ) ;
#17001 = DIRECTION ( 'NONE',  ( 0.000000000000000000, 0.000000000000000000, 1.000000000000000000 ) ) ;
#17002 = CARTESIAN_POINT ( 'NONE',  ( -77.84600223180727596, 40.00000000000000711, -20.84395318355897686 ) ) ;
#17003 = DIRECTION ( 'NONE',  ( 1.000000000000000000, -0.000000000000000000, 0.000000000000000000 ) ) ;
#17004 = ORIENTED_EDGE ( 'NONE', *, *, #4760, .T. ) ;
#17005 = DIRECTION ( 'NONE',  ( -1.000000000000000000, 0.000000000000000000, -0.000000000000000000 ) ) ;
#17006 = CIRCLE ( 'NONE', #13506, 59.00000000000000000 ) ;
#17007 = CARTESIAN_POINT ( 'NONE',  ( 17.99999999999999645, 0.000000000000000000, 0.000000000000000000 ) ) ;
#17008 = VECTOR ( 'NONE', #25880, 1000.000000000000000 ) ;
#17009 = VERTEX_POINT ( 'NONE', #37867 ) ;
#17010 = CIRCLE ( 'NONE', #25364, 2.649999999999979039 ) ;
#17011 = ORIENTED_EDGE ( 'NONE', *, *, #25911, .F. ) ;
#17012 = CARTESIAN_POINT ( 'NONE',  ( 0.000000000000000000, 0.000000000000000000, 0.000000000000000000 ) ) ;
#17013 = VERTEX_POINT ( 'NONE', #18088 ) ;
#17014 = CARTESIAN_POINT ( 'NONE',  ( 25.73918080462997082, 40.00000000000000000, -6.871072672212912735 ) ) ;
#17015 = CARTESIAN_POINT ( 'NONE',  ( 17.99999999999999645, 11.65176648921033298, 115.4133282497342918 ) ) ;
#17016 = CARTESIAN_POINT ( 'NONE',  ( 0.000000000000000000, 0.000000000000000000, 0.000000000000000000 ) ) ;
#17017 = DIRECTION ( 'NONE',  ( 1.000000000000000000, -3.336006684570784581E-17, 0.000000000000000000 ) ) ;
#17018 = CARTESIAN_POINT ( 'NONE',  ( -4.121423858225412573, -12.61643262889541184, -1.199999999999999956 ) ) ;
#17019 = VERTEX_POINT ( 'NONE', #4938 ) ;
#17021 = DIRECTION ( 'NONE',  ( -1.000000000000000000, -0.000000000000000000, 0.000000000000000000 ) ) ;
#17020 = DIRECTION ( 'NONE',  ( -1.000000000000000000, 0.000000000000000000, -0.000000000000000000 ) ) ;
#17022 = ORIENTED_EDGE ( 'NONE', *, *, #11394, .F. ) ;
#17023 = EDGE_CURVE ( 'NONE', #14989, #1664, #399, .T. ) ;
#17024 = AXIS2_PLACEMENT_3D ( 'NONE', #34596, #27417, #37435 ) ;
#17025 = DIRECTION ( 'NONE',  ( -1.000000000000000000, -0.000000000000000000, -0.000000000000000000 ) ) ;
#17026 = ADVANCED_FACE ( 'NONE', ( #8425 ), #41133, .T. ) ;
#17027 = FACE_OUTER_BOUND ( 'NONE', #16251, .T. ) ;
#17028 = ORIENTED_EDGE ( 'NONE', *, *, #13958, .T. ) ;
#17029 = CARTESIAN_POINT ( 'NONE',  ( 18.00000000000000355, 44.75336757549779776, 14.30704879393622164 ) ) ;
#17030 = CARTESIAN_POINT ( 'NONE',  ( 9.000000000000000000, -7.220349212960190499, -35.26849241522671718 ) ) ;
#17031 = CIRCLE ( 'NONE', #41365, 2.649999999999971934 ) ;
#17032 = DIRECTION ( 'NONE',  ( 0.000000000000000000, 0.1590634960190723812, -0.9872683547213445543 ) ) ;
#17033 = CARTESIAN_POINT ( 'NONE',  ( -69.75709431192164800, 31.00000000000000711, -9.183449035091399537 ) ) ;
#17034 = CIRCLE ( 'NONE', #41369, 120.5010000000000190 ) ;
#17035 = VERTEX_POINT ( 'NONE', #14573 ) ;
#17036 = CARTESIAN_POINT ( 'NONE',  ( -26.44890248586417414, 31.00000000000000355, -34.59877114778963403 ) ) ;
#17037 = AXIS2_PLACEMENT_3D ( 'NONE', #6104, #25979, #3232 ) ;
#17038 = CARTESIAN_POINT ( 'NONE',  ( 74.30822294231431613, 39.99999999999999289, -9.796771932235298408 ) ) ;
#17039 = DIRECTION ( 'NONE',  ( 0.000000000000000000, 0.000000000000000000, 1.000000000000000000 ) ) ;
#17040 = DIRECTION ( 'NONE',  ( 0.000000000000000000, 0.1590634960190655534, 0.9872683547213456645 ) ) ;
#17041 = EDGE_CURVE ( 'NONE', #16762, #11045, #24127, .T. ) ;
#17042 = EDGE_CURVE ( 'NONE', #26006, #12305, #22056, .T. ) ;
#17043 = EDGE_CURVE ( 'NONE', #16913, #42436, #21579, .T. ) ;
#17044 = ORIENTED_EDGE ( 'NONE', *, *, #11977, .T. ) ;
#17045 = CARTESIAN_POINT ( 'NONE',  ( 17.99999999999999645, 5.919241748380035695, -31.39643714728450163 ) ) ;
#17046 = CARTESIAN_POINT ( 'NONE',  ( 9.000000000000001776, -43.55304910509384797, -28.41006711800032036 ) ) ;
#17047 = AXIS2_PLACEMENT_3D ( 'NONE', #7440, #37543, #36893 ) ;
#17048 = EDGE_CURVE ( 'NONE', #1360, #2586, #24838, .T. ) ;
#17049 = ORIENTED_EDGE ( 'NONE', *, *, #15509, .T. ) ;
#17050 = CARTESIAN_POINT ( 'NONE',  ( -6.851565232941113415, 40.00000000000000000, -51.95325991929587417 ) ) ;
#17051 = CARTESIAN_POINT ( 'NONE',  ( 0.000000000000000000, 0.000000000000000000, 0.000000000000000000 ) ) ;
#17052 = AXIS2_PLACEMENT_3D ( 'NONE', #13946, #27686, #33991 ) ;
#17053 = CARTESIAN_POINT ( 'NONE',  ( 18.00000000000000355, 47.00885577955421013, -6.806061952191806874 ) ) ;
#17054 = VERTEX_POINT ( 'NONE', #4272 ) ;
#17055 = CARTESIAN_POINT ( 'NONE',  ( 17.99999999999999645, -3.803237743092135581, 31.26855263151013276 ) ) ;
#17056 = DIRECTION ( 'NONE',  ( -1.000000000000000000, 3.336006684570782732E-17, 0.000000000000000000 ) ) ;
#17057 = ORIENTED_EDGE ( 'NONE', *, *, #40936, .F. ) ;
#17058 = CARTESIAN_POINT ( 'NONE',  ( 17.99999999999999645, -27.83061035786878890, -117.2431154827800270 ) ) ;
#17059 = ORIENTED_EDGE ( 'NONE', *, *, #15404, .T. ) ;
#17060 = VECTOR ( 'NONE', #24923, 1000.000000000000000 ) ;
#17061 = AXIS2_PLACEMENT_3D ( 'NONE', #42076, #41438, #15093 ) ;
#17062 = VERTEX_POINT ( 'NONE', #34825 ) ;
#17063 = VECTOR ( 'NONE', #30763, 1000.000000000000000 ) ;
#17064 = DIRECTION ( 'NONE',  ( -1.000000000000000000, -0.000000000000000000, -0.000000000000000000 ) ) ;
#17065 = CARTESIAN_POINT ( 'NONE',  ( -91.59543978412355614, 31.00000000000000711, -12.18496625896582231 ) ) ;
#17066 = ORIENTED_EDGE ( 'NONE', *, *, #35082, .F. ) ;
#17067 = CARTESIAN_POINT ( 'NONE',  ( 0.000000000000000000, 0.000000000000000000, 0.000000000000000000 ) ) ;
#17068 = CIRCLE ( 'NONE', #19162, 99.99999999999994316 ) ;
#17069 = FACE_BOUND ( 'NONE', #27068, .T. ) ;
#17070 = LINE ( 'NONE', #19695, #28306 ) ;
#17071 = ORIENTED_EDGE ( 'NONE', *, *, #8153, .F. ) ;
#17072 = DIRECTION ( 'NONE',  ( -0.000000000000000000, -0.000000000000000000, 1.000000000000000000 ) ) ;
#17073 = AXIS2_PLACEMENT_3D ( 'NONE', #3627, #20073, #23328 ) ;
#17074 = DIRECTION ( 'NONE',  ( 0.000000000000000000, 0.000000000000000000, 1.000000000000000000 ) ) ;
#17076 = DIRECTION ( 'NONE',  ( -1.000000000000000000, -0.000000000000000000, -0.000000000000000000 ) ) ;
#17075 = DIRECTION ( 'NONE',  ( 1.000000000000000000, 0.000000000000000000, 0.000000000000000000 ) ) ;
#17077 = EDGE_CURVE ( 'NONE', #28092, #4616, #42201, .T. ) ;
#17078 = DIRECTION ( 'NONE',  ( 0.000000000000000000, -0.3612416661871601375, 0.9324722294043530368 ) ) ;
#17079 = DIRECTION ( 'NONE',  ( 0.000000000000000000, 0.000000000000000000, 1.000000000000000000 ) ) ;
#17080 = ORIENTED_EDGE ( 'NONE', *, *, #40908, .F. ) ;
#17082 = AXIS2_PLACEMENT_3D ( 'NONE', #20632, #30647, #23687 ) ;
#17081 = DIRECTION ( 'NONE',  ( 0.000000000000000000, 0.000000000000000000, 1.000000000000000000 ) ) ;
#17083 = CARTESIAN_POINT ( 'NONE',  ( -2.454369252093152376, 31.00000000000000355, 37.60416666486730009 ) ) ;
#17084 = ORIENTED_EDGE ( 'NONE', *, *, #30060, .F. ) ;
#17085 = CARTESIAN_POINT ( 'NONE',  ( -5.991980000000000750, 0.000000000000000000, 0.000000000000000000 ) ) ;
#17086 = DIRECTION ( 'NONE',  ( 0.000000000000000000, 0.000000000000000000, 1.000000000000000000 ) ) ;
#17087 = ORIENTED_EDGE ( 'NONE', *, *, #39864, .F. ) ;
#17088 = LINE ( 'NONE', #30378, #41463 ) ;
#17089 = CARTESIAN_POINT ( 'NONE',  ( 40.56819808336118882, 40.00000000000000000, -35.59309480518532354 ) ) ;
#17090 = AXIS2_PLACEMENT_3D ( 'NONE', #23290, #32858, #19800 ) ;
#17091 = CARTESIAN_POINT ( 'NONE',  ( -40.32452739091078797, 40.00000000000000000, -13.76986825753265720 ) ) ;
#17092 = AXIS2_PLACEMENT_3D ( 'NONE', #17246, #20299, #4520 ) ;
#17093 = AXIS2_PLACEMENT_3D ( 'NONE', #7937, #41303, #21306 ) ;
#17094 = VERTEX_POINT ( 'NONE', #37445 ) ;
#17095 = CARTESIAN_POINT ( 'NONE',  ( 17.99999999999999645, -75.72520367775142347, 82.78868281115956052 ) ) ;
#17096 = AXIS2_PLACEMENT_3D ( 'NONE', #26659, #39925, #33410 ) ;
#17097 = CYLINDRICAL_SURFACE ( 'NONE', #38142, 51.99999999999999289 ) ;
#17098 = AXIS2_PLACEMENT_3D ( 'NONE', #2487, #38941, #26086 ) ;
#17099 = EDGE_CURVE ( 'NONE', #12223, #3009, #19303, .T. ) ;
#17100 = DIRECTION ( 'NONE',  ( -1.000000000000000000, 0.000000000000000000, 0.000000000000000000 ) ) ;
#17101 = EDGE_CURVE ( 'NONE', #8291, #23736, #18505, .T. ) ;
#17102 = VECTOR ( 'NONE', #10371, 1000.000000000000000 ) ;
#17103 = ORIENTED_EDGE ( 'NONE', *, *, #18759, .F. ) ;
#17104 = CARTESIAN_POINT ( 'NONE',  ( 1.472621547668719444, 40.00000000000000000, -22.60416666365413718 ) ) ;
#17105 = ORIENTED_EDGE ( 'NONE', *, *, #7652, .T. ) ;
#17106 = DIRECTION ( 'NONE',  ( 1.000000000000000000, 0.000000000000000000, 0.000000000000000000 ) ) ;
#17107 = CARTESIAN_POINT ( 'NONE',  ( 17.99999999999999645, 87.74575819880170968, 75.87280091124503656 ) ) ;
#17108 = VERTEX_POINT ( 'NONE', #37656 ) ;
#17109 = DIRECTION ( 'NONE',  ( -1.000000000000000000, 0.000000000000000000, -0.000000000000000000 ) ) ;
#17110 = CARTESIAN_POINT ( 'NONE',  ( 17.99999999999999645, -87.92975456462855277, -69.68953103478244770 ) ) ;
#17111 = ORIENTED_EDGE ( 'NONE', *, *, #28934, .F. ) ;
#17112 = CARTESIAN_POINT ( 'NONE',  ( -5.991980000000000750, 1.842114939924247430E-15, -14.99999999999999822 ) ) ;
#17113 = ORIENTED_EDGE ( 'NONE', *, *, #28684, .F. ) ;
#17114 = CARTESIAN_POINT ( 'NONE',  ( 150.4999999999986926, 1.396217360982896810E-12, 9.999999999999962697 ) ) ;
#17115 = EDGE_CURVE ( 'NONE', #31141, #37671, #31349, .T. ) ;
#17116 = EDGE_LOOP ( 'NONE', ( #7850, #41708, #10539, #31278 ) ) ;
#17118 = ORIENTED_EDGE ( 'NONE', *, *, #20637, .F. ) ;
#17117 = PLANE ( 'NONE',  #21626 ) ;
#17119 = EDGE_CURVE ( 'NONE', #34811, #10513, #24181, .T. ) ;
#17120 = CARTESIAN_POINT ( 'NONE',  ( -54.47698434024490410, 31.00000000000000355, -31.57393205620728693 ) ) ;
#17121 = ORIENTED_EDGE ( 'NONE', *, *, #36626, .F. ) ;
#17122 = DIRECTION ( 'NONE',  ( 0.000000000000000000, 0.000000000000000000, 1.000000000000000000 ) ) ;
#17123 = CIRCLE ( 'NONE', #23369, 31.49899999999999878 ) ;
#17124 = AXIS2_PLACEMENT_3D ( 'NONE', #7095, #8346, #31488 ) ;
#17125 = ORIENTED_EDGE ( 'NONE', *, *, #25333, .F. ) ;
#17126 = AXIS2_PLACEMENT_3D ( 'NONE', #11610, #42478, #12623 ) ;
#17127 = CARTESIAN_POINT ( 'NONE',  ( 18.00000000000000355, -42.41764978026593269, -20.20639853260334107 ) ) ;
#17128 = VERTEX_POINT ( 'NONE', #34605 ) ;
#17129 = CARTESIAN_POINT ( 'NONE',  ( -26.95034633362163845, 40.00000000000000000, -79.72278128421112342 ) ) ;
#17130 = AXIS2_PLACEMENT_3D ( 'NONE', #28144, #25532, #8922 ) ;
#17131 = AXIS2_PLACEMENT_3D ( 'NONE', #441, #6560, #39714 ) ;
#17133 = DIRECTION ( 'NONE',  ( 0.000000000000000000, 0.8443279255020126328, 0.5358267949790005424 ) ) ;
#17132 = DIRECTION ( 'NONE',  ( 0.000000000000000000, -0.9822872507286903865, 0.1873813145857149975 ) ) ;
#17134 = AXIS2_PLACEMENT_3D ( 'NONE', #29801, #13646, #39992 ) ;
#17135 = CARTESIAN_POINT ( 'NONE',  ( 0.000000000000000000, -25.52601536738605859, 19.21447964122688390 ) ) ;
#17136 = ORIENTED_EDGE ( 'NONE', *, *, #4045, .T. ) ;
#17137 = FACE_OUTER_BOUND ( 'NONE', #28991, .T. ) ;
#17138 = ORIENTED_EDGE ( 'NONE', *, *, #4082, .T. ) ;
#17139 = CIRCLE ( 'NONE', #32423, 59.00000000000001421 ) ;
#17140 = CARTESIAN_POINT ( 'NONE',  ( 17.99999999999999645, 0.000000000000000000, 0.000000000000000000 ) ) ;
#17141 = CARTESIAN_POINT ( 'NONE',  ( 17.99999999999999645, 91.51415974874592507, 64.91094698989330425 ) ) ;
#17142 = CARTESIAN_POINT ( 'NONE',  ( -90.10416666596678681, 31.00000000000000711, -5.890486217120279200 ) ) ;
#17143 = DIRECTION ( 'NONE',  ( 0.000000000000000000, 0.000000000000000000, 1.000000000000000000 ) ) ;
#17144 = ORIENTED_EDGE ( 'NONE', *, *, #38290, .F. ) ;
#17145 = CARTESIAN_POINT ( 'NONE',  ( 18.00000000000000355, -26.17370628620681927, 39.63700417846155233 ) ) ;
#17146 = VERTEX_POINT ( 'NONE', #14786 ) ;
#17147 = DIRECTION ( 'NONE',  ( 1.000000000000000000, 0.000000000000000000, 0.000000000000000000 ) ) ;
#17148 = FACE_OUTER_BOUND ( 'NONE', #35769, .T. ) ;
#17150 = CARTESIAN_POINT ( 'NONE',  ( -101.9001375416480499, 31.00000000000000711, 6.549163350515033954 ) ) ;
#17149 = AXIS2_PLACEMENT_3D ( 'NONE', #1369, #28237, #18233 ) ;
#17151 = EDGE_CURVE ( 'NONE', #3818, #31641, #28369, .T. ) ;
#17152 = DIRECTION ( 'NONE',  ( 0.000000000000000000, 0.000000000000000000, 1.000000000000000000 ) ) ;
#17153 = AXIS2_PLACEMENT_3D ( 'NONE', #14598, #1895, #11308 ) ;
#17154 = EDGE_CURVE ( 'NONE', #14749, #23147, #19560, .T. ) ;
#17155 = VECTOR ( 'NONE', #31456, 1000.000000000000000 ) ;
#17156 = ORIENTED_EDGE ( 'NONE', *, *, #19144, .F. ) ;
#17157 = CARTESIAN_POINT ( 'NONE',  ( -10.00000000000000000, 0.000000000000000000, 0.000000000000000000 ) ) ;
#17158 = ORIENTED_EDGE ( 'NONE', *, *, #23556, .T. ) ;
#17159 = DIRECTION ( 'NONE',  ( 1.000000000000000000, 0.000000000000000000, 0.000000000000000000 ) ) ;
#17160 = CIRCLE ( 'NONE', #27576, 116.0000000000000000 ) ;
#17161 = CIRCLE ( 'NONE', #22065, 2.500000000000000888 ) ;
#17162 = CARTESIAN_POINT ( 'NONE',  ( 17.99999999999999645, -34.78944633786272789, -9.257128253673986507 ) ) ;
#17163 = CIRCLE ( 'NONE', #479, 10.49999999999999467 ) ;
#17164 = CARTESIAN_POINT ( 'NONE',  ( 18.00000000000000355, 45.78515115856043138, 12.64416602183680993 ) ) ;
#17165 = VERTEX_POINT ( 'NONE', #2492 ) ;
#17166 = ORIENTED_EDGE ( 'NONE', *, *, #41659, .F. ) ;
#17167 = FACE_OUTER_BOUND ( 'NONE', #28740, .T. ) ;
#17168 = LINE ( 'NONE', #10587, #24969 ) ;
#17169 = ADVANCED_FACE ( 'NONE', ( #18735 ), #8805, .T. ) ;
#17170 = VECTOR ( 'NONE', #23766, 1000.000000000000114 ) ;
#17171 = LINE ( 'NONE', #7742, #36881 ) ;
#17173 = VERTEX_POINT ( 'NONE', #32406 ) ;
#17172 = FACE_OUTER_BOUND ( 'NONE', #22392, .T. ) ;
#17174 = EDGE_CURVE ( 'NONE', #10231, #5717, #18612, .T. ) ;
#17175 = CARTESIAN_POINT ( 'NONE',  ( 32.62694724487210607, 31.00000000000000355, -16.02036196159510339 ) ) ;
#17176 = CARTESIAN_POINT ( 'NONE',  ( 0.000000000000000000, 21.48775762007859669, 23.64423737150145399 ) ) ;
#17178 = ORIENTED_EDGE ( 'NONE', *, *, #40546, .F. ) ;
#17177 = LINE ( 'NONE', #10382, #42528 ) ;
#17179 = VERTEX_POINT ( 'NONE', #12782 ) ;
#17180 = CARTESIAN_POINT ( 'NONE',  ( -4.121423858225412573, -12.61643262889541184, 0.000000000000000000 ) ) ;
#17181 = DIRECTION ( 'NONE',  ( 0.000000000000000000, 1.541976423090494253E-15, 1.000000000000000000 ) ) ;
#17182 = CARTESIAN_POINT ( 'NONE',  ( 43.74200748489512591, 40.00000000000000000, 38.49442098324160355 ) ) ;
#17183 = VECTOR ( 'NONE', #20933, 1000.000000000000000 ) ;
#17184 = DIRECTION ( 'NONE',  ( -1.000000000000000000, -0.000000000000000000, -0.000000000000000000 ) ) ;
#17185 = CIRCLE ( 'NONE', #3885, 116.0000000000000000 ) ;
#17186 = CARTESIAN_POINT ( 'NONE',  ( 0.000000000000000000, 0.000000000000000000, 0.000000000000000000 ) ) ;
#17188 = ORIENTED_EDGE ( 'NONE', *, *, #8542, .F. ) ;
#17187 = AXIS2_PLACEMENT_3D ( 'NONE', #5660, #21657, #1737 ) ;
#17189 = DIRECTION ( 'NONE',  ( 0.000000000000000000, -0.7525707698561440173, 0.6585113790650324317 ) ) ;
#17190 = ADVANCED_FACE ( 'NONE', ( #42208 ), #29575, .T. ) ;
#17191 = CIRCLE ( 'NONE', #31082, 59.00000000000000000 ) ;
#17192 = EDGE_LOOP ( 'NONE', ( #6761, #30915, #4335, #29895 ) ) ;
#17193 = EDGE_CURVE ( 'NONE', #40970, #42489, #30433, .T. ) ;
#17194 = CIRCLE ( 'NONE', #11604, 120.5010000000000332 ) ;
#17195 = DIRECTION ( 'NONE',  ( -1.000000000000000000, -0.000000000000000000, -0.000000000000000000 ) ) ;
#17196 = DIRECTION ( 'NONE',  ( 1.000000000000000000, -1.373900992973641868E-15, -6.546126324440886161E-16 ) ) ;
#17198 = EDGE_CURVE ( 'NONE', #29037, #2879, #22795, .T. ) ;
#17197 = CARTESIAN_POINT ( 'NONE',  ( 26.72236725836960147, 31.00000000000000355, -46.28813965123160301 ) ) ;
#17199 = FACE_OUTER_BOUND ( 'NONE', #25525, .T. ) ;
#17201 = ORIENTED_EDGE ( 'NONE', *, *, #15662, .T. ) ;
#17200 = AXIS2_PLACEMENT_3D ( 'NONE', #37280, #7616, #17039 ) ;
#17203 = AXIS2_PLACEMENT_3D ( 'NONE', #21597, #24860, #31802 ) ;
#17202 = CARTESIAN_POINT ( 'NONE',  ( 9.000000000000001776, -31.08872492059927595, -41.68322423723131465 ) ) ;
#17204 = ORIENTED_EDGE ( 'NONE', *, *, #16757, .T. ) ;
#17205 = CARTESIAN_POINT ( 'NONE',  ( -99.89583333318432778, 31.00000000000000711, 6.544984695199788760 ) ) ;
#17206 = VERTEX_POINT ( 'NONE', #42632 ) ;
#17207 = DIRECTION ( 'NONE',  ( 1.000000000000000000, -0.000000000000000000, -0.000000000000000000 ) ) ;
#17208 = CARTESIAN_POINT ( 'NONE',  ( -6.599999999999991651, -19.99999999999999289, 2.449293598294706119E-15 ) ) ;
#17209 = CARTESIAN_POINT ( 'NONE',  ( 58.79931003850258975, 31.00000000000000355, 51.72161244499935151 ) ) ;
#17210 = CARTESIAN_POINT ( 'NONE',  ( -20.82795069772234342, 40.00000000000000000, 77.32795358076222669 ) ) ;
#17211 = DIRECTION ( 'NONE',  ( 1.000000000000000000, -0.000000000000000000, 0.000000000000000000 ) ) ;
#17212 = EDGE_CURVE ( 'NONE', #20513, #7249, #26091, .T. ) ;
#17213 = ORIENTED_EDGE ( 'NONE', *, *, #42821, .F. ) ;
#17214 = CARTESIAN_POINT ( 'NONE',  ( 0.000000000000000000, 26.17370628620655282, 39.63700417846171575 ) ) ;
#17215 = ORIENTED_EDGE ( 'NONE', *, *, #29944, .T. ) ;
#17216 = DIRECTION ( 'NONE',  ( 0.000000000000000000, 0.000000000000000000, 1.000000000000000000 ) ) ;
#17217 = DIRECTION ( 'NONE',  ( 1.000000000000000000, 0.000000000000000000, 0.000000000000000000 ) ) ;
#17218 = VECTOR ( 'NONE', #11953, 1000.000000000000000 ) ;
#17220 = EDGE_LOOP ( 'NONE', ( #41410, #20030, #16769, #18602 ) ) ;
#17219 = FACE_OUTER_BOUND ( 'NONE', #38559, .T. ) ;
#17221 = CIRCLE ( 'NONE', #41560, 59.00000000000001421 ) ;
#17222 = DIRECTION ( 'NONE',  ( 0.000000000000000000, 0.000000000000000000, 1.000000000000000000 ) ) ;
#17224 = ORIENTED_EDGE ( 'NONE', *, *, #13170, .T. ) ;
#17223 = VECTOR ( 'NONE', #19176, 1000.000000000000000 ) ;
#17225 = FACE_OUTER_BOUND ( 'NONE', #18773, .T. ) ;
#17226 = AXIS2_PLACEMENT_3D ( 'NONE', #35463, #5371, #32198 ) ;
#17227 = EDGE_CURVE ( 'NONE', #41341, #23828, #6712, .T. ) ;
#17228 = CARTESIAN_POINT ( 'NONE',  ( -80.10416666582359824, 40.00000000000000711, -5.235987747607834031 ) ) ;
#17229 = DIRECTION ( 'NONE',  ( 0.000000000000000000, 0.000000000000000000, 1.000000000000000000 ) ) ;
#17230 =( GEOMETRIC_REPRESENTATION_CONTEXT ( 3 ) GLOBAL_UNCERTAINTY_ASSIGNED_CONTEXT ( ( #29602 ) ) GLOBAL_UNIT_ASSIGNED_CONTEXT ( ( #26675, #35612, #32570 ) ) REPRESENTATION_CONTEXT ( 'NONE', 'WORKASPACE' ) );
#17231 = ORIENTED_EDGE ( 'NONE', *, *, #23345, .F. ) ;
#17232 = CARTESIAN_POINT ( 'NONE',  ( 17.99999999999999645, 57.40245293794799153, -96.40140491896575270 ) ) ;
#17233 = ADVANCED_FACE ( 'NONE', ( #25468 ), #2914, .F. ) ;
#17234 = CARTESIAN_POINT ( 'NONE',  ( 6.600000000000004974, 19.59999999999999787, 0.000000000000000000 ) ) ;
#17235 = VECTOR ( 'NONE', #18095, 1000.000000000000000 ) ;
#17236 = VERTEX_POINT ( 'NONE', #2071 ) ;
#17237 = AXIS2_PLACEMENT_3D ( 'NONE', #34581, #37843, #28066 ) ;
#17238 =( NAMED_UNIT ( * ) PLANE_ANGLE_UNIT ( ) SI_UNIT ( $, .RADIAN. ) );
#17239 = ORIENTED_EDGE ( 'NONE', *, *, #7680, .T. ) ;
#17240 = CARTESIAN_POINT ( 'NONE',  ( 0.000000000000000000, -24.72041153920704204, -40.55929306992713634 ) ) ;
#17241 = ORIENTED_EDGE ( 'NONE', *, *, #18402, .T. ) ;
#17242 = CARTESIAN_POINT ( 'NONE',  ( 26.53203760875094019, 40.00000000000000000, 7.134992448515056651 ) ) ;
#17243 = CARTESIAN_POINT ( 'NONE',  ( 17.99999999999999645, -5.919241748379815427, 31.39643714728454427 ) ) ;
#17244 = AXIS2_PLACEMENT_3D ( 'NONE', #15834, #29779, #26071 ) ;
#17245 = DIRECTION ( 'NONE',  ( 0.000000000000000000, 0.3612416661871471479, 0.9324722294043580328 ) ) ;
#17246 = CARTESIAN_POINT ( 'NONE',  ( 18.00000000000000355, 0.000000000000000000, 0.000000000000000000 ) ) ;
#17247 = CYLINDRICAL_SURFACE ( 'NONE', #13683, 120.5010000000000190 ) ;
#17248 = ORIENTED_EDGE ( 'NONE', *, *, #12793, .F. ) ;
#17250 = CARTESIAN_POINT ( 'NONE',  ( 0.000000000000000000, 25.18647942089895153, -113.2326863338525271 ) ) ;
#17249 = CARTESIAN_POINT ( 'NONE',  ( 8.999999999999998224, -73.51007459736368332, -89.73443560133438268 ) ) ;
#17251 = ORIENTED_EDGE ( 'NONE', *, *, #27755, .F. ) ;
#17252 = CARTESIAN_POINT ( 'NONE',  ( 6.200000000000003730, 6.971071669133949438E-15, 0.000000000000000000 ) ) ;
#17254 = ADVANCED_FACE ( 'NONE', ( #28733 ), #16274, .F. ) ;
#17253 = CARTESIAN_POINT ( 'NONE',  ( -27.62299686580952240, 31.00000000000000355, -13.61136854378590577 ) ) ;
#17256 = ORIENTED_EDGE ( 'NONE', *, *, #15251, .F. ) ;
#17255 = CIRCLE ( 'NONE', #30493, 20.00000000000000711 ) ;
#17257 = DIRECTION ( 'NONE',  ( 0.000000000000000000, 0.8477344278896686847, 0.5304209081197460707 ) ) ;
#17258 = EDGE_CURVE ( 'NONE', #1626, #38421, #26942, .T. ) ;
#17259 = DIRECTION ( 'NONE',  ( 0.000000000000000000, 0.000000000000000000, 1.000000000000000000 ) ) ;
#17260 = CIRCLE ( 'NONE', #42268, 58.99999999999998579 ) ;
#17261 = AXIS2_PLACEMENT_3D ( 'NONE', #22973, #12694, #19905 ) ;
#17262 = CARTESIAN_POINT ( 'NONE',  ( -10.00000000000000000, 0.000000000000000000, 0.000000000000000000 ) ) ;
#17263 = CARTESIAN_POINT ( 'NONE',  ( 18.89933391970155085, 31.00000000000000355, -70.58587736658564893 ) ) ;
#17264 = AXIS2_PLACEMENT_3D ( 'NONE', #15119, #4606, #37765 ) ;
#17265 = CIRCLE ( 'NONE', #31872, 2.500000000000000444 ) ;
#17266 = VERTEX_POINT ( 'NONE', #28939 ) ;
#17268 = CARTESIAN_POINT ( 'NONE',  ( 3.148395399070833989, 31.00000000000000355, 49.39975974383467872 ) ) ;
#17267 = AXIS2_PLACEMENT_3D ( 'NONE', #18256, #11457, #41754 ) ;
#17269 = CARTESIAN_POINT ( 'NONE',  ( -25.13323546007955045, 40.00000000000000000, 74.03861446737784036 ) ) ;
#17270 = EDGE_CURVE ( 'NONE', #42546, #19619, #23476, .T. ) ;
#17271 = EDGE_CURVE ( 'NONE', #19094, #12205, #2703, .T. ) ;
#17272 = LINE ( 'NONE', #37507, #29723 ) ;
#17273 = DIRECTION ( 'NONE',  ( 0.000000000000000000, 0.000000000000000000, 1.000000000000000000 ) ) ;
#17274 = ORIENTED_EDGE ( 'NONE', *, *, #27875, .T. ) ;
#17275 = CARTESIAN_POINT ( 'NONE',  ( 8.999999999999998224, -79.18387647320706435, -84.76976882518842160 ) ) ;
#17276 = DIRECTION ( 'NONE',  ( -1.000000000000000000, 0.000000000000000000, -0.000000000000000000 ) ) ;
#17277 = PRODUCT_DEFINITION_SHAPE ( 'NONE', 'NONE',  #43197 ) ;
#17278 = EDGE_CURVE ( 'NONE', #276, #6849, #19139, .T. ) ;
#17279 = ORIENTED_EDGE ( 'NONE', *, *, #4756, .F. ) ;
#17280 = CARTESIAN_POINT ( 'NONE',  ( 48.45771864870608425, 40.00000000000000000, 27.97524394371832202 ) ) ;
#17281 = CARTESIAN_POINT ( 'NONE',  ( 17.99999999999999645, 21.48775762007859669, 23.64423737150145399 ) ) ;
#17282 = CARTESIAN_POINT ( 'NONE',  ( 17.99999999999999645, -116.0452958106478434, -32.46506308663576590 ) ) ;
#17283 = ORIENTED_EDGE ( 'NONE', *, *, #1091, .F. ) ;
#17284 = EDGE_CURVE ( 'NONE', #10707, #8886, #42923, .T. ) ;
#17285 = VECTOR ( 'NONE', #10802, 1000.000000000000000 ) ;
#17286 = FACE_OUTER_BOUND ( 'NONE', #22976, .T. ) ;
#17287 = CARTESIAN_POINT ( 'NONE',  ( -4.000000000000000000, -0.3979232138631226823, -3.896351557369779711E-17 ) ) ;
#17288 = ORIENTED_EDGE ( 'NONE', *, *, #27130, .F. ) ;
#17289 = FACE_OUTER_BOUND ( 'NONE', #10855, .T. ) ;
#17290 = VERTEX_POINT ( 'NONE', #25892 ) ;
#17291 = VECTOR ( 'NONE', #10968, 999.9999999999997726 ) ;
#17292 = AXIS2_PLACEMENT_3D ( 'NONE', #4147, #14445, #18179 ) ;
#17293 = DIRECTION ( 'NONE',  ( 0.000000000000000000, 0.000000000000000000, 1.000000000000000000 ) ) ;
#17294 = ORIENTED_EDGE ( 'NONE', *, *, #42125, .T. ) ;
#17295 = CIRCLE ( 'NONE', #20064, 59.00000000000000000 ) ;
#17296 = LINE ( 'NONE', #9629, #9045 ) ;
#17297 = AXIS2_PLACEMENT_3D ( 'NONE', #40455, #36975, #33702 ) ;
#17298 = CARTESIAN_POINT ( 'NONE',  ( -26.02152878260477564, 31.00000000000000355, 96.68563202202810203 ) ) ;
#17299 = ORIENTED_EDGE ( 'NONE', *, *, #4922, .T. ) ;
#17300 = AXIS2_PLACEMENT_3D ( 'NONE', #6382, #29321, #16236 ) ;
#17301 = CARTESIAN_POINT ( 'NONE',  ( 8.999999999999998224, 14.91999999999999993, 0.000000000000000000 ) ) ;
#17302 = DIRECTION ( 'NONE',  ( 0.000000000000000000, 0.000000000000000000, 1.000000000000000000 ) ) ;
#17303 = ORIENTED_EDGE ( 'NONE', *, *, #18599, .F. ) ;
#17304 = CARTESIAN_POINT ( 'NONE',  ( 106.4195705685756792, -106.4195705685758213, 9.999999999999669598 ) ) ;
#17305 = VECTOR ( 'NONE', #35065, 1000.000000000000000 ) ;
#17306 = CARTESIAN_POINT ( 'NONE',  ( 0.000000000000000000, 0.000000000000000000, -20.00000000000000000 ) ) ;
#17307 = EDGE_CURVE ( 'NONE', #25294, #26402, #22851, .T. ) ;
#17308 = EDGE_CURVE ( 'NONE', #30585, #16736, #22628, .T. ) ;
#17309 = CARTESIAN_POINT ( 'NONE',  ( -10.00000000000000000, 0.000000000000000000, 0.000000000000000000 ) ) ;
#17310 = EDGE_CURVE ( 'NONE', #4060, #11416, #29042, .T. ) ;
#17311 = EDGE_CURVE ( 'NONE', #1858, #880, #8125, .T. ) ;
#17312 = DIRECTION ( 'NONE',  ( -1.000000000000000000, 0.000000000000000000, 0.000000000000000000 ) ) ;
#17313 = ORIENTED_EDGE ( 'NONE', *, *, #40674, .T. ) ;
#17314 = DIRECTION ( 'NONE',  ( 0.9904134141151967885, 1.188683942061883417E-16, -0.1381349671179612493 ) ) ;
#17315 = CARTESIAN_POINT ( 'NONE',  ( 0.000000000000000000, -25.46650492921884279, -19.29328419707811193 ) ) ;
#17316 = CARTESIAN_POINT ( 'NONE',  ( 32.11716166826300167, 31.00000000000000355, 15.82712457579038912 ) ) ;
#17317 = VERTEX_POINT ( 'NONE', #36307 ) ;
#17318 = CARTESIAN_POINT ( 'NONE',  ( 18.00000000000000355, -38.92705108641749945, 27.21837053747784552 ) ) ;
#17319 = CYLINDRICAL_SURFACE ( 'NONE', #42542, 20.00000000000000355 ) ;
#17320 = CIRCLE ( 'NONE', #41654, 20.00000000000000355 ) ;
#17321 = VERTEX_POINT ( 'NONE', #16935 ) ;
#17322 = FACE_OUTER_BOUND ( 'NONE', #20527, .T. ) ;
#17323 = CARTESIAN_POINT ( 'NONE',  ( -49.46937513889707105, 40.00000000000000000, 6.524320044134898744 ) ) ;
#17324 = CIRCLE ( 'NONE', #7492, 58.99999999999999289 ) ;
#17325 = CARTESIAN_POINT ( 'NONE',  ( -13.02511903071888533, 40.00000000000000000, 48.29538318457647961 ) ) ;
#17326 = VECTOR ( 'NONE', #1649, 1000.000000000000000 ) ;
#17327 = AXIS2_PLACEMENT_3D ( 'NONE', #41528, #8172, #11681 ) ;
#17328 = ORIENTED_EDGE ( 'NONE', *, *, #14218, .T. ) ;
#17329 = CYLINDRICAL_SURFACE ( 'NONE', #17923, 59.00000000000000000 ) ;
#17330 = DIRECTION ( 'NONE',  ( -1.000000000000000000, 0.000000000000000000, -0.000000000000000000 ) ) ;
#17331 = AXIS2_PLACEMENT_3D ( 'NONE', #3022, #16391, #41908 ) ;
#17332 = DIRECTION ( 'NONE',  ( 0.000000000000000000, -0.7980172272802321665, -0.6026346363792661753 ) ) ;
#17333 = CARTESIAN_POINT ( 'NONE',  ( 0.000000000000000000, 0.000000000000000000, -25.00000000000000000 ) ) ;
#17334 = VERTEX_POINT ( 'NONE', #6635 ) ;
#17335 = CARTESIAN_POINT ( 'NONE',  ( 2.965790448435745574, 40.00000000000000000, -22.56328348808469997 ) ) ;
#17336 = ORIENTED_EDGE ( 'NONE', *, *, #10320, .T. ) ;
#17337 = CARTESIAN_POINT ( 'NONE',  ( 17.99999999999999645, 13.57797752207923381, 33.34124362422479493 ) ) ;
#17338 = LINE ( 'NONE', #7025, #37459 ) ;
#17339 = ORIENTED_EDGE ( 'NONE', *, *, #2446, .T. ) ;
#17340 = AXIS2_PLACEMENT_3D ( 'NONE', #18070, #28069, #5125 ) ;
#17341 = DIRECTION ( 'NONE',  ( -1.000000000000000000, 0.000000000000000000, 0.000000000000000000 ) ) ;
#17342 = DIRECTION ( 'NONE',  ( 1.000000000000000000, -3.469446951953614189E-17, 0.000000000000000000 ) ) ;
#17343 = ORIENTED_EDGE ( 'NONE', *, *, #39114, .T. ) ;
#17344 = CARTESIAN_POINT ( 'NONE',  ( 0.000000000000000000, -30.71634675606060227, 8.790889055186445589 ) ) ;
#17345 = ORIENTED_EDGE ( 'NONE', *, *, #1979, .T. ) ;
#17346 = DIRECTION ( 'NONE',  ( 1.000000000000000000, 0.000000000000000000, 0.000000000000000000 ) ) ;
#17347 = ORIENTED_EDGE ( 'NONE', *, *, #20808, .F. ) ;
#17349 = EDGE_LOOP ( 'NONE', ( #25763, #27566, #41813, #32460 ) ) ;
#17348 = CARTESIAN_POINT ( 'NONE',  ( 0.000000000000000000, 0.000000000000000000, -116.0000000000000000 ) ) ;
#17350 = CARTESIAN_POINT ( 'NONE',  ( -23.73339997550686675, 31.00000000000000355, -70.23208777904191891 ) ) ;
#17351 = ORIENTED_EDGE ( 'NONE', *, *, #31600, .F. ) ;
#17352 = DIRECTION ( 'NONE',  ( 0.000000000000000000, 0.000000000000000000, 1.000000000000000000 ) ) ;
#17353 = AXIS2_PLACEMENT_3D ( 'NONE', #35153, #1988, #18641 ) ;
#17354 = VERTEX_POINT ( 'NONE', #7281 ) ;
#17355 = DIRECTION ( 'NONE',  ( 0.000000000000000000, 1.000000000000000000, 0.000000000000000000 ) ) ;
#17356 = EDGE_LOOP ( 'NONE', ( #22173, #29867, #12788, #41116 ) ) ;
#17357 = CARTESIAN_POINT ( 'NONE',  ( 28.55926749299792178, 40.00000000000000000, 84.46800049165049984 ) ) ;
#17358 = CIRCLE ( 'NONE', #8259, 2.100000000000000089 ) ;
#17360 = CARTESIAN_POINT ( 'NONE',  ( 139.4999999999992610, -1.479897297339870344E-13, 9.999999999999946709 ) ) ;
#17359 = DIRECTION ( 'NONE',  ( -1.000000000000000000, 0.000000000000000000, 0.000000000000000000 ) ) ;
#17361 = EDGE_CURVE ( 'NONE', #16661, #33331, #27169, .T. ) ;
#17362 = EDGE_CURVE ( 'NONE', #17236, #5841, #5321, .T. ) ;
#17363 = DIRECTION ( 'NONE',  ( 0.000000000000000000, 0.000000000000000000, 1.000000000000000000 ) ) ;
#17364 = DIRECTION ( 'NONE',  ( -1.000000000000000000, 0.000000000000000000, 0.000000000000000000 ) ) ;
#17365 = ORIENTED_EDGE ( 'NONE', *, *, #34847, .T. ) ;
#17366 = EDGE_CURVE ( 'NONE', #18461, #19393, #9489, .T. ) ;
#17367 = FACE_OUTER_BOUND ( 'NONE', #39444, .T. ) ;
#17368 = CARTESIAN_POINT ( 'NONE',  ( 38.45889818826288575, 31.00000000000000355, 77.98987599019784511 ) ) ;
#17369 = CARTESIAN_POINT ( 'NONE',  ( 147.8500000000000227, 1.576728355889448963E-12, 6.999999999999998224 ) ) ;
#17370 = VERTEX_POINT ( 'NONE', #39789 ) ;
#17371 = CARTESIAN_POINT ( 'NONE',  ( 0.000000000000000000, -22.66088087769164972, -21.87856208362581256 ) ) ;
#17372 = EDGE_LOOP ( 'NONE', ( #28945, #27372, #19181, #11504 ) ) ;
#17373 = ADVANCED_FACE ( 'NONE', ( #26312 ), #33039, .T. ) ;
#17374 = ORIENTED_EDGE ( 'NONE', *, *, #34123, .F. ) ;
#17375 = DIRECTION ( 'NONE',  ( 0.000000000000000000, 1.000000000000000000, 0.000000000000000000 ) ) ;
#17376 = CARTESIAN_POINT ( 'NONE',  ( 0.000000000000000000, 0.000000000000000000, 0.000000000000000000 ) ) ;
#17377 = AXIS2_PLACEMENT_3D ( 'NONE', #36645, #30131, #13779 ) ;
#17378 =( LENGTH_UNIT ( ) NAMED_UNIT ( * ) SI_UNIT ( .MILLI., .METRE. ) );
#17379 = CIRCLE ( 'NONE', #1999, 0.08000000000000020983 ) ;
#17380 = DIRECTION ( 'NONE',  ( 0.000000000000000000, 0.9618256431728180456, 0.2736629900720866093 ) ) ;
#17381 = VECTOR ( 'NONE', #30870, 1000.000000000000000 ) ;
#17382 = ORIENTED_EDGE ( 'NONE', *, *, #19309, .F. ) ;
#17383 = LINE ( 'NONE', #524, #5422 ) ;
#17384 = ORIENTED_EDGE ( 'NONE', *, *, #40493, .T. ) ;
#17385 = CARTESIAN_POINT ( 'NONE',  ( 17.99999999999999645, 0.000000000000000000, 0.000000000000000000 ) ) ;
#17386 = CARTESIAN_POINT ( 'NONE',  ( 8.999999999999998224, -108.8880088604279166, 39.99251838045924501 ) ) ;
#17387 = DIRECTION ( 'NONE',  ( 1.000000000000000000, 0.000000000000000000, 0.000000000000000000 ) ) ;
#17388 = VERTEX_POINT ( 'NONE', #20641 ) ;
#17389 = EDGE_CURVE ( 'NONE', #21931, #3781, #20217, .T. ) ;
#17390 = ORIENTED_EDGE ( 'NONE', *, *, #15910, .F. ) ;
#17391 = DIRECTION ( 'NONE',  ( -1.000000000000000000, 0.000000000000000000, 0.000000000000000000 ) ) ;
#17392 = CARTESIAN_POINT ( 'NONE',  ( 18.00000000000000355, 12.30077720129095198, 50.52416135122085450 ) ) ;
#17393 = DIRECTION ( 'NONE',  ( 0.000000000000000000, -0.3612416661871601375, 0.9324722294043530368 ) ) ;
#17394 = ORIENTED_EDGE ( 'NONE', *, *, #41649, .T. ) ;
#17396 = ORIENTED_EDGE ( 'NONE', *, *, #12143, .F. ) ;
#17395 = DIRECTION ( 'NONE',  ( -1.000000000000000000, 0.000000000000000000, 0.000000000000000000 ) ) ;
#17397 = CARTESIAN_POINT ( 'NONE',  ( -31.99444157862340532, 31.00000000000000355, -4.262017635501121227 ) ) ;
#17398 = CARTESIAN_POINT ( 'NONE',  ( 42.80287614962790599, -40.05525454449572464, 69.29271901957253021 ) ) ;
#17400 = ORIENTED_EDGE ( 'NONE', *, *, #16584, .T. ) ;
#17399 = CARTESIAN_POINT ( 'NONE',  ( -6.004904395537136175, -19.19999999999999574, 2.351321854362917684E-15 ) ) ;
#17401 = VERTEX_POINT ( 'NONE', #33476 ) ;
#17402 = CYLINDRICAL_SURFACE ( 'NONE', #25281, 51.99999999999999289 ) ;
#17403 = CARTESIAN_POINT ( 'NONE',  ( -30.89738163651703928, 40.00000000000000000, 40.13100860032159289 ) ) ;
#17404 = VECTOR ( 'NONE', #27397, 1000.000000000000000 ) ;
#17405 = CIRCLE ( 'NONE', #23690, 47.49900000000000944 ) ;
#17406 = DIRECTION ( 'NONE',  ( -1.000000000000000000, 0.000000000000000000, 0.000000000000000000 ) ) ;
#17407 = PRODUCT_DEFINITION_CONTEXT ( 'detailed design', #32827, 'design' ) ;
#17408 = EDGE_CURVE ( 'NONE', #23134, #14428, #33878, .T. ) ;
#17409 = CARTESIAN_POINT ( 'NONE',  ( 8.999999999999998224, 79.18387647320761857, 84.76976882518788159 ) ) ;
#17410 = ORIENTED_EDGE ( 'NONE', *, *, #20357, .F. ) ;
#17411 = CARTESIAN_POINT ( 'NONE',  ( 18.00000000000000355, -46.87740477351715640, 16.82754413119429771 ) ) ;
#17412 = ORIENTED_EDGE ( 'NONE', *, *, #25107, .T. ) ;
#17413 = LINE ( 'NONE', #20684, #8566 ) ;
#17414 = CARTESIAN_POINT ( 'NONE',  ( -150.4999999999986926, -2.921102061156358310E-13, 10.00000000000004619 ) ) ;
#17415 = CARTESIAN_POINT ( 'NONE',  ( -56.43872490705654599, 31.00000000000000711, 19.17141758013517716 ) ) ;
#17416 = DIRECTION ( 'NONE',  ( 0.000000000000000000, 0.3681245526846786964, -0.9297764858882511252 ) ) ;
#17417 = VERTEX_POINT ( 'NONE', #10128 ) ;
#17418 = ADVANCED_FACE ( 'NONE', ( #16501 ), #30438, .T. ) ;
#17419 = EDGE_CURVE ( 'NONE', #18858, #909, #65, .T. ) ;
#17420 = CARTESIAN_POINT ( 'NONE',  ( 0.000000000000000000, 0.000000000000000000, 0.000000000000000000 ) ) ;
#17421 = ORIENTED_EDGE ( 'NONE', *, *, #23393, .T. ) ;
#17422 = CARTESIAN_POINT ( 'NONE',  ( 31.25450476884064699, 31.00000000000000355, 92.02345382966369414 ) ) ;
#17423 = AXIS2_PLACEMENT_3D ( 'NONE', #14394, #34221, #11119 ) ;
#17424 = EDGE_CURVE ( 'NONE', #4402, #42699, #10910, .T. ) ;
#17425 = ORIENTED_EDGE ( 'NONE', *, *, #33726, .T. ) ;
#17426 = CARTESIAN_POINT ( 'NONE',  ( -5.639656061357299244, -10.48075544252182922, -1.199999999999999956 ) ) ;
#17427 = CARTESIAN_POINT ( 'NONE',  ( 17.99999999999999645, -120.4984140710909344, 0.7894348306980537577 ) ) ;
#17428 = CARTESIAN_POINT ( 'NONE',  ( -53.44803860757283331, 31.00000000000000355, 46.73995993579659114 ) ) ;
#17429 = CARTESIAN_POINT ( 'NONE',  ( 47.76959191294547935, 40.00000000000000000, 62.44753968353898443 ) ) ;
#17430 = CARTESIAN_POINT ( 'NONE',  ( 0.000000000000000000, 0.000000000000000000, 0.000000000000000000 ) ) ;
#17431 = ORIENTED_EDGE ( 'NONE', *, *, #39074, .F. ) ;
#17432 = CARTESIAN_POINT ( 'NONE',  ( 0.000000000000000000, 0.000000000000000000, 0.000000000000000000 ) ) ;
#17433 = ORIENTED_EDGE ( 'NONE', *, *, #40262, .F. ) ;
#17434 = AXIS2_PLACEMENT_3D ( 'NONE', #19803, #22658, #29837 ) ;
#17435 = LINE ( 'NONE', #30277, #29756 ) ;
#17436 = CARTESIAN_POINT ( 'NONE',  ( 0.000000000000000000, 48.55277268144325120, 105.3500273609081432 ) ) ;
#17437 = AXIS2_PLACEMENT_3D ( 'NONE', #33445, #36926, #29766 ) ;
#17439 = ORIENTED_EDGE ( 'NONE', *, *, #30231, .T. ) ;
#17438 = DIRECTION ( 'NONE',  ( 0.000000000000000000, 0.000000000000000000, 1.000000000000000000 ) ) ;
#17440 = LINE ( 'NONE', #39853, #19165 ) ;
#17441 = ORIENTED_EDGE ( 'NONE', *, *, #27133, .T. ) ;
#17442 = CARTESIAN_POINT ( 'NONE',  ( 0.000000000000000000, 0.000000000000000000, 0.000000000000000000 ) ) ;
#17443 = AXIS2_PLACEMENT_3D ( 'NONE', #35572, #25794, #35766 ) ;
#17444 = CARTESIAN_POINT ( 'NONE',  ( -89.21153162435624040, 40.00000000000000711, 11.76024306507019901 ) ) ;
#17445 = CARTESIAN_POINT ( 'NONE',  ( 0.000000000000000000, 0.000000000000000000, 0.000000000000000000 ) ) ;
#17446 = EDGE_CURVE ( 'NONE', #22368, #26752, #10201, .T. ) ;
#17447 = ORIENTED_EDGE ( 'NONE', *, *, #7946, .F. ) ;
#17448 = DIRECTION ( 'NONE',  ( -1.000000000000000000, -0.000000000000000000, 0.000000000000000000 ) ) ;
#17449 = DIRECTION ( 'NONE',  ( 0.000000000000000000, 0.000000000000000000, 1.000000000000000000 ) ) ;
#17450 = VERTEX_POINT ( 'NONE', #13648 ) ;
#17451 = DIRECTION ( 'NONE',  ( 3.996523416598930318E-16, -2.658563593772947863E-15, -1.000000000000000000 ) ) ;
#17452 = ORIENTED_EDGE ( 'NONE', *, *, #8804, .T. ) ;
#17453 = CARTESIAN_POINT ( 'NONE',  ( 17.99999999999999645, 41.62036691425530677, 113.0850832732715787 ) ) ;
#17454 = ORIENTED_EDGE ( 'NONE', *, *, #11179, .F. ) ;
#17455 = CARTESIAN_POINT ( 'NONE',  ( -10.52919346384764054, 40.00000000000000000, -21.36894910329525743 ) ) ;
#17456 = DIRECTION ( 'NONE',  ( -1.000000000000000000, 1.084202172485488534E-16, 0.000000000000000000 ) ) ;
#17457 = FACE_OUTER_BOUND ( 'NONE', #11578, .T. ) ;
#17458 = DIRECTION ( 'NONE',  ( -1.000000000000000000, 0.000000000000000000, 0.000000000000000000 ) ) ;
#17459 = VERTEX_POINT ( 'NONE', #13224 ) ;
#17461 = LINE ( 'NONE', #10892, #1128 ) ;
#17460 = FACE_OUTER_BOUND ( 'NONE', #8295, .T. ) ;
#17462 = ADVANCED_FACE ( 'NONE', ( #3768 ), #23262, .T. ) ;
#17463 = VERTEX_POINT ( 'NONE', #4001 ) ;
#17464 = CIRCLE ( 'NONE', #13985, 120.5010000000000190 ) ;
#17465 = CARTESIAN_POINT ( 'NONE',  ( 0.000000000000000000, 80.02407177072956301, 78.64108602299977235 ) ) ;
#17466 = CIRCLE ( 'NONE', #29959, 59.00000000000000711 ) ;
#17468 = CARTESIAN_POINT ( 'NONE',  ( 24.21999397792122366, 31.00000000000000355, 8.216913396989165008 ) ) ;
#17467 = AXIS2_PLACEMENT_3D ( 'NONE', #16644, #17064, #36429 ) ;
#17469 = ORIENTED_EDGE ( 'NONE', *, *, #35669, .T. ) ;
#17470 = DIRECTION ( 'NONE',  ( 0.000000000000000000, 3.528251137579946599E-15, -1.000000000000000000 ) ) ;
#17471 = CARTESIAN_POINT ( 'NONE',  ( 0.000000000000000000, 114.6488492393079639, 37.09625815500055523 ) ) ;
#17472 = ITEM_DEFINED_TRANSFORMATION ( 'NONE', 'NONE', #24722,  #13552 ) ;
#17473 = ADVANCED_FACE ( 'NONE', ( #17148 ), #9712, .T. ) ;
#17474 = DIRECTION ( 'NONE',  ( 0.000000000000000000, 0.8951632913550635617, -0.4457383557765359772 ) ) ;
#17475 = CARTESIAN_POINT ( 'NONE',  ( -30.22953878324074495, 31.00000000000000355, 61.32923288305941867 ) ) ;
#17476 = ORIENTED_EDGE ( 'NONE', *, *, #12619, .F. ) ;
#17477 = CARTESIAN_POINT ( 'NONE',  ( 2.996940313443769099, 31.00000000000000355, -44.59688583547567475 ) ) ;
#17478 = CARTESIAN_POINT ( 'NONE',  ( -51.96644965832453522, 40.00000000000000711, 59.25555446698126616 ) ) ;
#17479 = DIRECTION ( 'NONE',  ( -1.000000000000000000, -0.000000000000000000, -0.000000000000000000 ) ) ;
#17480 = CARTESIAN_POINT ( 'NONE',  ( 0.000000000000000000, -120.2856157092986393, -7.201503623198056481 ) ) ;
#17481 = LINE ( 'NONE', #9864, #17063 ) ;
#17483 = ORIENTED_EDGE ( 'NONE', *, *, #34108, .F. ) ;
#17482 = DIRECTION ( 'NONE',  ( -1.000000000000000000, 0.000000000000000000, 0.000000000000000000 ) ) ;
#17484 = FACE_OUTER_BOUND ( 'NONE', #26399, .T. ) ;
#17485 = AXIS2_PLACEMENT_3D ( 'NONE', #37429, #23943, #20248 ) ;
#17486 = CARTESIAN_POINT ( 'NONE',  ( -2.449848172108560540, -3.432307619358754724, -3.503702292528910078 ) ) ;
#17487 = VERTEX_POINT ( 'NONE', #26725 ) ;
#17488 = CARTESIAN_POINT ( 'NONE',  ( 18.36587843422771016, 40.00000000000000000, 54.06640964556338957 ) ) ;
#17489 = CARTESIAN_POINT ( 'NONE',  ( 17.99999999999999645, -107.2703412112697094, 32.88383143828427535 ) ) ;
#17492 = EDGE_CURVE ( 'NONE', #20680, #35337, #13008, .T. ) ;
#17491 = DIRECTION ( 'NONE',  ( 0.000000000000000000, 0.000000000000000000, 1.000000000000000000 ) ) ;
#17490 = AXIS2_PLACEMENT_3D ( 'NONE', #9938, #12806, #6030 ) ;
#17493 = CIRCLE ( 'NONE', #41834, 31.49899999999999878 ) ;
#17494 = VERTEX_POINT ( 'NONE', #938 ) ;
#17496 = EDGE_CURVE ( 'NONE', #20343, #30860, #15803, .T. ) ;
#17495 = AXIS2_PLACEMENT_3D ( 'NONE', #21441, #857, #14652 ) ;
#17497 = DIRECTION ( 'NONE',  ( -1.000000000000000000, -0.000000000000000000, -0.000000000000000000 ) ) ;
#17498 = CARTESIAN_POINT ( 'NONE',  ( 0.000000000000000000, 0.000000000000000000, 0.000000000000000000 ) ) ;
#17499 = VECTOR ( 'NONE', #27070, 1000.000000000000000 ) ;
#17500 = ORIENTED_EDGE ( 'NONE', *, *, #40201, .F. ) ;
#17501 = CARTESIAN_POINT ( 'NONE',  ( 17.99999999999999645, 0.000000000000000000, 0.000000000000000000 ) ) ;
#17502 = ORIENTED_EDGE ( 'NONE', *, *, #9336, .F. ) ;
#17503 = CARTESIAN_POINT ( 'NONE',  ( 102.9999999999993321, -2.372200916521103027E-13, -40.00000000000000000 ) ) ;
#17504 = EDGE_LOOP ( 'NONE', ( #24145, #41385, #33874, #4265 ) ) ;
#17505 = CARTESIAN_POINT ( 'NONE',  ( 0.000000000000000000, -51.27532863109435368, 99.79535634195110561 ) ) ;
#17506 = CARTESIAN_POINT ( 'NONE',  ( 0.000000000000000000, -11.49545354908914518, -29.80986809967271967 ) ) ;
#17507 = ORIENTED_EDGE ( 'NONE', *, *, #7961, .T. ) ;
#17508 = FACE_OUTER_BOUND ( 'NONE', #3178, .T. ) ;
#17509 = CARTESIAN_POINT ( 'NONE',  ( 17.99999999999999645, 119.8996782608631406, -12.02323392193236629 ) ) ;
#17510 = ORIENTED_EDGE ( 'NONE', *, *, #22301, .F. ) ;
#17511 = DIRECTION ( 'NONE',  ( 0.000000000000000000, 0.000000000000000000, 1.000000000000000000 ) ) ;
#17512 = DIRECTION ( 'NONE',  ( 0.000000000000000000, 0.000000000000000000, 1.000000000000000000 ) ) ;
#17513 = CIRCLE ( 'NONE', #23090, 59.00000000000000000 ) ;
#17514 = DIRECTION ( 'NONE',  ( 0.000000000000000000, 0.000000000000000000, 1.000000000000000000 ) ) ;
#17515 = AXIS2_PLACEMENT_3D ( 'NONE', #11715, #25048, #8407 ) ;
#17516 = DIRECTION ( 'NONE',  ( 1.000000000000000000, 0.000000000000000000, 0.000000000000000000 ) ) ;
#17517 = EDGE_LOOP ( 'NONE', ( #18300, #33960, #42651, #2193 ) ) ;
#17518 = DIRECTION ( 'NONE',  ( 1.659994950812577912E-17, 0.9999999999999998890, 1.377814977426256780E-16 ) ) ;
#17519 = EDGE_CURVE ( 'NONE', #23300, #21142, #8838, .T. ) ;
#17520 = DIRECTION ( 'NONE',  ( 0.000000000000000000, 0.000000000000000000, 1.000000000000000000 ) ) ;
#17521 = CARTESIAN_POINT ( 'NONE',  ( -35.44024466369167925, 31.00000000000000355, -20.45798383175513635 ) ) ;
#17522 = AXIS2_PLACEMENT_3D ( 'NONE', #26539, #32649, #39607 ) ;
#17523 = VERTEX_POINT ( 'NONE', #11025 ) ;
#17525 = DIRECTION ( 'NONE',  ( 0.000000000000000000, 0.000000000000000000, 1.000000000000000000 ) ) ;
#17524 = CARTESIAN_POINT ( 'NONE',  ( 17.99999999999999645, -67.32409792376445523, -89.75376489259431878 ) ) ;
#17526 = CIRCLE ( 'NONE', #41863, 36.00000000000000000 ) ;
#17527 = ADVANCED_FACE ( 'NONE', ( #31076 ), #1167, .F. ) ;
#17528 = CARTESIAN_POINT ( 'NONE',  ( 18.00000000000000355, 0.000000000000000000, 0.000000000000000000 ) ) ;
#17529 = ORIENTED_EDGE ( 'NONE', *, *, #11365, .F. ) ;
#17530 = CIRCLE ( 'NONE', #25197, 51.99999999999999289 ) ;
#17531 = DIRECTION ( 'NONE',  ( -1.000000000000000000, 0.000000000000000000, 0.000000000000000000 ) ) ;
#17532 = CARTESIAN_POINT ( 'NONE',  ( 44.89583333484414140, 40.00000000000000000, -2.945243104263157274 ) ) ;
#17533 = CARTESIAN_POINT ( 'NONE',  ( -37.00582609754565766, 40.00000000000000000, 48.07482304778140758 ) ) ;
#17534 = AXIS2_PLACEMENT_3D ( 'NONE', #603, #42943, #10002 ) ;
#17535 = CARTESIAN_POINT ( 'NONE',  ( -4.000000000000000000, 0.000000000000000000, 0.000000000000000000 ) ) ;
#17536 = DIRECTION ( 'NONE',  ( 1.000000000000000000, 0.000000000000000000, 0.000000000000000000 ) ) ;
#17537 = AXIS2_PLACEMENT_3D ( 'NONE', #26667, #23413, #39934 ) ;
#17538 = DIRECTION ( 'NONE',  ( -3.996523416598930318E-16, 2.658563593772947863E-15, 1.000000000000000000 ) ) ;
#17539 = DIRECTION ( 'NONE',  ( 0.000000000000000000, -6.938893903907226800E-15, 1.000000000000000000 ) ) ;
#17540 = ORIENTED_EDGE ( 'NONE', *, *, #20951, .T. ) ;
#17541 = CARTESIAN_POINT ( 'NONE',  ( 23.12883206328222130, 40.00000000000000000, 11.39561251172168355 ) ) ;
#17542 = ORIENTED_EDGE ( 'NONE', *, *, #37473, .F. ) ;
#17543 = FACE_OUTER_BOUND ( 'NONE', #21613, .T. ) ;
#17544 = DIRECTION ( 'NONE',  ( -1.000000000000000000, 0.000000000000000000, -0.000000000000000000 ) ) ;
#17545 = EDGE_CURVE ( 'NONE', #3430, #20704, #36003, .T. ) ;
#17546 = VERTEX_POINT ( 'NONE', #8165 ) ;
#17547 = EDGE_CURVE ( 'NONE', #26216, #40741, #33219, .T. ) ;
#17548 = CYLINDRICAL_SURFACE ( 'NONE', #11033, 2.000000000000000888 ) ;
#17549 = EDGE_CURVE ( 'NONE', #28005, #41293, #6743, .T. ) ;
#17550 = EDGE_CURVE ( 'NONE', #39523, #5471, #11663, .T. ) ;
#17551 = CYLINDRICAL_SURFACE ( 'NONE', #30382, 59.00000000000001421 ) ;
#17552 = ORIENTED_EDGE ( 'NONE', *, *, #42508, .F. ) ;
#17553 = CARTESIAN_POINT ( 'NONE',  ( 0.000000000000000000, -61.59243992711522964, 93.77976230226020959 ) ) ;
#17554 = ORIENTED_EDGE ( 'NONE', *, *, #19103, .T. ) ;
#17555 = DIRECTION ( 'NONE',  ( 1.000000000000000000, -1.373900992973641868E-15, -6.546126324440886161E-16 ) ) ;
#17556 = AXIS2_PLACEMENT_3D ( 'NONE', #37839, #7962, #18065 ) ;
#17557 = ORIENTED_EDGE ( 'NONE', *, *, #10204, .T. ) ;
#17559 = ORIENTED_EDGE ( 'NONE', *, *, #39033, .F. ) ;
#17558 = DIRECTION ( 'NONE',  ( 3.009274222672345096E-17, 1.000000000000000000, -2.455023325076455345E-18 ) ) ;
#17560 = VECTOR ( 'NONE', #30144, 1000.000000000000000 ) ;
#17561 = CARTESIAN_POINT ( 'NONE',  ( 67.48878131082855703, 31.00000000000000000, 39.09986611101695786 ) ) ;
#17562 = ORIENTED_EDGE ( 'NONE', *, *, #25107, .F. ) ;
#17563 = CARTESIAN_POINT ( 'NONE',  ( 2.500000000000000000, -2.357898499370432166, 3.035766082959412415E-15 ) ) ;
#17564 = CIRCLE ( 'NONE', #27276, 11.00000000000023803 ) ;
#17565 = ORIENTED_EDGE ( 'NONE', *, *, #39768, .F. ) ;
#17566 = DIRECTION ( 'NONE',  ( -1.000000000000000000, 0.000000000000000000, -0.000000000000000000 ) ) ;
#17567 = ORIENTED_EDGE ( 'NONE', *, *, #8153, .T. ) ;
#17568 = CARTESIAN_POINT ( 'NONE',  ( -83.29221842949013421, 40.00000000000000711, -41.19657635676244922 ) ) ;
#17569 = VECTOR ( 'NONE', #10342, 1000.000000000000000 ) ;
#17571 = DIRECTION ( 'NONE',  ( 0.000000000000000000, 0.000000000000000000, 1.000000000000000000 ) ) ;
#17570 = FACE_OUTER_BOUND ( 'NONE', #31912, .T. ) ;
#17572 = DIRECTION ( 'NONE',  ( 0.000000000000000000, 0.000000000000000000, 1.000000000000000000 ) ) ;
#17573 = DIRECTION ( 'NONE',  ( 0.000000000000000000, 0.000000000000000000, 1.000000000000000000 ) ) ;
#17574 = VERTEX_POINT ( 'NONE', #20871 ) ;
#17575 = FILL_AREA_STYLE ('',( #10558 ) ) ;
#17576 = EDGE_CURVE ( 'NONE', #38193, #22892, #18040, .T. ) ;
#17577 = DIRECTION ( 'NONE',  ( -1.000000000000000000, 0.000000000000000000, 0.000000000000000000 ) ) ;
#17578 = CYLINDRICAL_SURFACE ( 'NONE', #16379, 20.00000000000000711 ) ;
#17579 = CARTESIAN_POINT ( 'NONE',  ( 57.06996419934371545, 31.00000000000000000, 65.05326946699807422 ) ) ;
#17580 = EDGE_CURVE ( 'NONE', #23370, #34600, #22831, .T. ) ;
#17581 = CARTESIAN_POINT ( 'NONE',  ( -19.99999999999999645, 31.00000000000000355, 1.283214542831033755 ) ) ;
#17582 = ORIENTED_EDGE ( 'NONE', *, *, #35139, .F. ) ;
#17583 = CARTESIAN_POINT ( 'NONE',  ( 1.888402776346428613, 40.00000000000000000, 29.39821258742166776 ) ) ;
#17584 = AXIS2_PLACEMENT_3D ( 'NONE', #28860, #22987, #36228 ) ;
#17585 =( REPRESENTATION_RELATIONSHIP ('NONE','NONE', #330, #18009 ) REPRESENTATION_RELATIONSHIP_WITH_TRANSFORMATION ( #17472 )SHAPE_REPRESENTATION_RELATIONSHIP( ) );
#17586 = EDGE_LOOP ( 'NONE', ( #6757, #23459, #23691, #38903 ) ) ;
#17587 = AXIS2_PLACEMENT_3D ( 'NONE', #8019, #35061, #14815 ) ;
#17588 = ORIENTED_EDGE ( 'NONE', *, *, #19654, .F. ) ;
#17589 = CARTESIAN_POINT ( 'NONE',  ( 2.804994570502171047, 3.229033611042449792, -3.526374918436834704 ) ) ;
#17590 = CARTESIAN_POINT ( 'NONE',  ( 0.000000000000000000, 0.000000000000000000, 6.999999999999998224 ) ) ;
#17591 = FILL_AREA_STYLE_COLOUR ( '', #40776 ) ;
#17592 = CIRCLE ( 'NONE', #37038, 116.0000000000000000 ) ;
#17593 = LINE ( 'NONE', #38259, #1669 ) ;
#17594 = ORIENTED_EDGE ( 'NONE', *, *, #22311, .F. ) ;
#17595 = CARTESIAN_POINT ( 'NONE',  ( 0.000000000000000000, 2.418575551222442055, -120.4767259403368769 ) ) ;
#17596 = ORIENTED_EDGE ( 'NONE', *, *, #24683, .T. ) ;
#17597 = DIRECTION ( 'NONE',  ( -1.000000000000000000, 0.000000000000000000, 0.000000000000000000 ) ) ;
#17598 = AXIS2_PLACEMENT_3D ( 'NONE', #39278, #6147, #22553 ) ;
#17599 = DIRECTION ( 'NONE',  ( -1.000000000000000000, -0.000000000000000000, 0.000000000000000000 ) ) ;
#17600 = EDGE_CURVE ( 'NONE', #7715, #28643, #26257, .T. ) ;
#17601 = CARTESIAN_POINT ( 'NONE',  ( 17.99999999999999645, 0.000000000000000000, 0.000000000000000000 ) ) ;
#17602 = EDGE_CURVE ( 'NONE', #25476, #29070, #12350, .T. ) ;
#17603 = ADVANCED_FACE ( 'NONE', ( #14288 ), #20027, .T. ) ;
#17604 = CYLINDRICAL_SURFACE ( 'NONE', #22042, 59.00000000000000000 ) ;
#17605 = ORIENTED_EDGE ( 'NONE', *, *, #21702, .T. ) ;
#17606 = EDGE_LOOP ( 'NONE', ( #35259, #25658, #14768, #39154 ) ) ;
#17607 = CYLINDRICAL_SURFACE ( 'NONE', #67, 120.5010000000000190 ) ;
#17608 = CARTESIAN_POINT ( 'NONE',  ( 17.99999999999999645, 40.37724737310070111, 104.6802291180868565 ) ) ;
#17609 = EDGE_CURVE ( 'NONE', #40313, #13499, #42950, .T. ) ;
#17610 = DIRECTION ( 'NONE',  ( -1.000000000000000000, 0.000000000000000000, 0.000000000000000000 ) ) ;
#17611 = ORIENTED_EDGE ( 'NONE', *, *, #31178, .F. ) ;
#17613 = EDGE_LOOP ( 'NONE', ( #36426, #22833, #14944, #16891 ) ) ;
#17612 = CARTESIAN_POINT ( 'NONE',  ( 0.000000000000000000, -89.07460286905796920, -81.15544420875052367 ) ) ;
#17614 = CARTESIAN_POINT ( 'NONE',  ( -14.09736097164098823, 31.00000000000000355, -41.75563764759219509 ) ) ;
#17615 = CARTESIAN_POINT ( 'NONE',  ( 17.99999999999999645, 15.21076497709711184, 119.5371223922155792 ) ) ;
#17617 = ORIENTED_EDGE ( 'NONE', *, *, #6241, .T. ) ;
#17616 = DIRECTION ( 'NONE',  ( -1.000000000000000000, 0.000000000000000000, 0.000000000000000000 ) ) ;
#17618 = ORIENTED_EDGE ( 'NONE', *, *, #21006, .T. ) ;
#17619 = AXIS2_PLACEMENT_3D ( 'NONE', #42305, #33139, #32499 ) ;
#17620 = VECTOR ( 'NONE', #27966, 1000.000000000000000 ) ;
#17621 = CARTESIAN_POINT ( 'NONE',  ( 64.03668805593822810, 39.99999999999999289, 21.85318084037336561 ) ) ;
#17622 = VECTOR ( 'NONE', #22106, 1000.000000000000000 ) ;
#17623 = EDGE_CURVE ( 'NONE', #10231, #2623, #31838, .T. ) ;
#17624 = CARTESIAN_POINT ( 'NONE',  ( 9.000000000000001776, 52.88069566989596382, -103.2454939717363516 ) ) ;
#17625 = VECTOR ( 'NONE', #30341, 1000.000000000000000 ) ;
#17626 = DIRECTION ( 'NONE',  ( -1.000000000000000000, -0.000000000000000000, -0.000000000000000000 ) ) ;
#17627 = ORIENTED_EDGE ( 'NONE', *, *, #40540, .F. ) ;
#17628 = DIRECTION ( 'NONE',  ( 0.000000000000000000, -0.8747630845319658288, 0.4845508703326421585 ) ) ;
#17629 = ORIENTED_EDGE ( 'NONE', *, *, #22208, .T. ) ;
#17630 =( NAMED_UNIT ( * ) SI_UNIT ( $, .STERADIAN. ) SOLID_ANGLE_UNIT ( ) );
#17631 = AXIS2_PLACEMENT_3D ( 'NONE', #27100, #13577, #13804 ) ;
#17632 = CARTESIAN_POINT ( 'NONE',  ( 0.000000000000000000, 31.11570115861502828, -4.898994019976315784 ) ) ;
#17633 = CARTESIAN_POINT ( 'NONE',  ( 9.000000000000000000, -35.89808275599447285, 2.706964063997107317 ) ) ;
#17634 = CARTESIAN_POINT ( 'NONE',  ( 42.89889459577944564, 31.00000000000000355, -32.91970121835214513 ) ) ;
#17635 = CARTESIAN_POINT ( 'NONE',  ( 0.000000000000000000, 31.81777574834302058, 2.898764365605871696 ) ) ;
#17636 = VERTEX_POINT ( 'NONE', #41080 ) ;
#17637 = EDGE_CURVE ( 'NONE', #16220, #23467, #40869, .T. ) ;
#17638 = DIRECTION ( 'NONE',  ( 0.000000000000000000, 0.1837495178165706178, -0.9829730996839017854 ) ) ;
#17639 = ORIENTED_EDGE ( 'NONE', *, *, #28631, .F. ) ;
#17640 = CARTESIAN_POINT ( 'NONE',  ( -8.325335757348113930, 40.00000000000000000, -31.05587074991522201 ) ) ;
#17641 = ORIENTED_EDGE ( 'NONE', *, *, #14083, .F. ) ;
#17642 = CARTESIAN_POINT ( 'NONE',  ( 52.26814377733353467, -2.055254544495723756, -19.42827587850796434 ) ) ;
#17643 = DIRECTION ( 'NONE',  ( 1.000000000000000000, 0.000000000000000000, 0.000000000000000000 ) ) ;
#17644 = CARTESIAN_POINT ( 'NONE',  ( -71.72626536482266602, 31.00000000000000711, -9.557116936239163252 ) ) ;
#17645 = CARTESIAN_POINT ( 'NONE',  ( 51.69257347811147696, 40.00000000000000000, 59.10123636508003386 ) ) ;
#17646 = DIRECTION ( 'NONE',  ( -1.000000000000000000, -0.000000000000000000, 0.000000000000000000 ) ) ;
#17647 = AXIS2_PLACEMENT_3D ( 'NONE', #41832, #31390, #31824 ) ;
#17648 = ORIENTED_EDGE ( 'NONE', *, *, #24612, .F. ) ;
#17649 = DIRECTION ( 'NONE',  ( 0.000000000000000000, -0.9957341762950355779, 0.09226835946329130234 ) ) ;
#17650 = VERTEX_POINT ( 'NONE', #4430 ) ;
#17651 = DIRECTION ( 'NONE',  ( 1.000000000000000000, 0.000000000000000000, 0.000000000000000000 ) ) ;
#17652 = CARTESIAN_POINT ( 'NONE',  ( -4.000000000000004441, 2.309401076758496263, -3.504269196027523847 ) ) ;
#17653 = AXIS2_PLACEMENT_3D ( 'NONE', #39012, #32265, #35730 ) ;
#17655 = VERTEX_POINT ( 'NONE', #17804 ) ;
#17654 = CARTESIAN_POINT ( 'NONE',  ( 17.99999999999999645, -23.87611429743677505, 20.54551452399611478 ) ) ;
#17656 = EDGE_CURVE ( 'NONE', #1418, #11001, #2552, .T. ) ;
#17657 = CYLINDRICAL_SURFACE ( 'NONE', #28217, 20.00000000000000355 ) ;
#17658 = ORIENTED_EDGE ( 'NONE', *, *, #12030, .T. ) ;
#17659 = DIRECTION ( 'NONE',  ( 0.000000000000000000, -0.5264321628773627193, 0.8502171357296098853 ) ) ;
#17660 = CARTESIAN_POINT ( 'NONE',  ( 42.89041025189590783, 40.00000000000000000, 86.97820559439793442 ) ) ;
#17661 = CARTESIAN_POINT ( 'NONE',  ( -0.6507732100473471171, 4.243078065514775510, -0.2236248678334823436 ) ) ;
#17662 = AXIS2_PLACEMENT_3D ( 'NONE', #4985, #17908, #1696 ) ;
#17663 = ORIENTED_EDGE ( 'NONE', *, *, #20270, .F. ) ;
#17664 = DIRECTION ( 'NONE',  ( -1.000000000000000000, 0.000000000000000000, 0.000000000000000000 ) ) ;
#17665 = CARTESIAN_POINT ( 'NONE',  ( 17.99999999999999645, 0.000000000000000000, 0.000000000000000000 ) ) ;
#17666 = VERTEX_POINT ( 'NONE', #24565 ) ;
#17667 = EDGE_CURVE ( 'NONE', #25771, #1782, #17260, .T. ) ;
#17668 = CARTESIAN_POINT ( 'NONE',  ( 17.99999999999999645, 0.000000000000000000, 0.000000000000000000 ) ) ;
#17669 = VERTEX_POINT ( 'NONE', #15587 ) ;
#17670 = CYLINDRICAL_SURFACE ( 'NONE', #35843, 13.59999999999999964 ) ;
#17671 = ORIENTED_EDGE ( 'NONE', *, *, #19082, .F. ) ;
#17672 = CARTESIAN_POINT ( 'NONE',  ( -4.434938641671375414, 40.00000000000000000, -34.07637162044569834 ) ) ;
#17673 = CARTESIAN_POINT ( 'NONE',  ( -15.99999999999997691, 40.00000000000000000, 5.571627607371296764E-15 ) ) ;
#17674 = ADVANCED_FACE ( 'NONE', ( #19296 ), #1816, .T. ) ;
#17675 = DIRECTION ( 'NONE',  ( -1.000000000000000000, -0.000000000000000000, -0.000000000000000000 ) ) ;
#17676 = CARTESIAN_POINT ( 'NONE',  ( 18.00000000000000355, 0.000000000000000000, 0.000000000000000000 ) ) ;
#17677 = ORIENTED_EDGE ( 'NONE', *, *, #32482, .F. ) ;
#17679 = CARTESIAN_POINT ( 'NONE',  ( 0.000000000000000000, -36.05989434073635636, 30.12041790338605551 ) ) ;
#17678 = LINE ( 'NONE', #31385, #25233 ) ;
#17680 = VERTEX_POINT ( 'NONE', #21937 ) ;
#17681 = CIRCLE ( 'NONE', #37149, 58.99999999999999289 ) ;
#17682 = CARTESIAN_POINT ( 'NONE',  ( 9.000000000000001776, -43.55304910509425298, 28.41006711799970574 ) ) ;
#17683 = CARTESIAN_POINT ( 'NONE',  ( -14.19360040536685830, 31.00000000000000355, 24.59234967646941783 ) ) ;
#17684 = EDGE_LOOP ( 'NONE', ( #2419, #5486, #42720, #27781 ) ) ;
#17685 = CARTESIAN_POINT ( 'NONE',  ( 0.000000000000000000, 57.69704296431184787, 105.7900857083231472 ) ) ;
#17686 = CARTESIAN_POINT ( 'NONE',  ( -4.000000000000000000, 2.309401076758498483, -3.433295621305379353 ) ) ;
#17687 = PRESENTATION_LAYER_ASSIGNMENT (  '', '', ( #26712 ) ) ;
#17688 = LINE ( 'NONE', #1045, #42757 ) ;
#17689 = CARTESIAN_POINT ( 'NONE',  ( 36.74538074116732389, 31.00000000000000355, -63.64477163140654170 ) ) ;
#17690 = AXIS2_PLACEMENT_3D ( 'NONE', #560, #13914, #7114 ) ;
#17691 = VERTEX_POINT ( 'NONE', #42152 ) ;
#17692 = CARTESIAN_POINT ( 'NONE',  ( 40.10317558968866081, 31.00000000000000355, -23.06553963618950931 ) ) ;
#17693 = CARTESIAN_POINT ( 'NONE',  ( 68.07048008643859305, 39.99999999999999289, 33.55317283102968418 ) ) ;
#17694 = FACE_BOUND ( 'NONE', #31234, .T. ) ;
#17695 = LINE ( 'NONE', #20532, #4724 ) ;
#17696 = DIRECTION ( 'NONE',  ( -1.000000000000000000, -0.000000000000000000, -0.000000000000000000 ) ) ;
#17697 = CIRCLE ( 'NONE', #32294, 20.00000000000000355 ) ;
#17699 = ORIENTED_EDGE ( 'NONE', *, *, #32084, .F. ) ;
#17698 = CARTESIAN_POINT ( 'NONE',  ( 0.000000000000000000, 0.000000000000000000, 0.000000000000000000 ) ) ;
#17700 = ADVANCED_FACE ( 'NONE', ( #5941 ), #18455, .F. ) ;
#17701 = DIRECTION ( 'NONE',  ( -3.996523416598930318E-16, 2.658563593772947863E-15, 1.000000000000000000 ) ) ;
#17702 = CARTESIAN_POINT ( 'NONE',  ( -0.6920835326022555245, -4.454600218803899558, -3.597382984111586079 ) ) ;
#17703 = EDGE_CURVE ( 'NONE', #26433, #19475, #5731, .T. ) ;
#17704 = AXIS2_PLACEMENT_3D ( 'NONE', #27993, #24518, #15122 ) ;
#17705 = ORIENTED_EDGE ( 'NONE', *, *, #34165, .T. ) ;
#17706 = CARTESIAN_POINT ( 'NONE',  ( 54.43714469963884284, 40.00000000000000000, -7.178810421751046000 ) ) ;
#17707 = CARTESIAN_POINT ( 'NONE',  ( 0.000000000000000000, -98.39501399267926729, -53.91376164787777014 ) ) ;
#17708 = DIRECTION ( 'NONE',  ( -1.000000000000000000, 0.000000000000000000, -0.000000000000000000 ) ) ;
#17709 = ORIENTED_EDGE ( 'NONE', *, *, #7271, .F. ) ;
#17710 = DIRECTION ( 'NONE',  ( 0.000000000000000000, 0.000000000000000000, 1.000000000000000000 ) ) ;
#17711 = DIRECTION ( 'NONE',  ( 0.000000000000000000, 0.6736956436465584286, -0.7390089172206580903 ) ) ;
#17712 = ORIENTED_EDGE ( 'NONE', *, *, #18629, .F. ) ;
#17713 = FACE_OUTER_BOUND ( 'NONE', #15643, .T. ) ;
#17714 = ORIENTED_EDGE ( 'NONE', *, *, #18711, .F. ) ;
#17715 = STYLED_ITEM ( 'NONE', ( #503 ), #3052 ) ;
#17716 = EDGE_CURVE ( 'NONE', #28510, #37542, #12308, .T. ) ;
#17717 = FACE_OUTER_BOUND ( 'NONE', #19799, .T. ) ;
#17718 = AXIS2_PLACEMENT_3D ( 'NONE', #8212, #21343, #7765 ) ;
#17719 = ORIENTED_EDGE ( 'NONE', *, *, #22788, .T. ) ;
#17720 = LINE ( 'NONE', #31863, #23069 ) ;
#17721 = CARTESIAN_POINT ( 'NONE',  ( 17.99999999999999645, 0.000000000000000000, 0.000000000000000000 ) ) ;
#17722 = EDGE_CURVE ( 'NONE', #4034, #21051, #29069, .T. ) ;
#17723 = ORIENTED_EDGE ( 'NONE', *, *, #29962, .T. ) ;
#17724 = DIRECTION ( 'NONE',  ( 0.000000000000000000, 0.000000000000000000, 1.000000000000000000 ) ) ;
#17725 = DIRECTION ( 'NONE',  ( 0.000000000000000000, -0.1837495178165570453, -0.9829730996839042279 ) ) ;
#17727 = ORIENTED_EDGE ( 'NONE', *, *, #32163, .T. ) ;
#17726 = CIRCLE ( 'NONE', #38562, 58.99999999999998579 ) ;
#17728 = DIRECTION ( 'NONE',  ( 0.000000000000000000, 0.6845471059286899473, -0.7289686274214103312 ) ) ;
#17729 = CARTESIAN_POINT ( 'NONE',  ( 0.000000000000000000, -34.74871106919691499, 106.6808302961370600 ) ) ;
#17730 = CYLINDRICAL_SURFACE ( 'NONE', #37784, 116.0000000000000000 ) ;
#17731 = AXIS2_PLACEMENT_3D ( 'NONE', #40325, #6744, #20108 ) ;
#17732 = CARTESIAN_POINT ( 'NONE',  ( 0.000000000000000000, 0.000000000000000000, 0.000000000000000000 ) ) ;
#17733 = ORIENTED_EDGE ( 'NONE', *, *, #4725, .F. ) ;
#17734 = DIRECTION ( 'NONE',  ( 0.000000000000000000, 0.000000000000000000, 1.000000000000000000 ) ) ;
#17736 = AXIS2_PLACEMENT_3D ( 'NONE', #22690, #29642, #35522 ) ;
#17735 = DIRECTION ( 'NONE',  ( 0.000000000000000000, 0.000000000000000000, -1.000000000000000000 ) ) ;
#17737 = CARTESIAN_POINT ( 'NONE',  ( -30.97228021248666607, 31.00000000000000355, 23.76985434021725041 ) ) ;
#17738 = EDGE_CURVE ( 'NONE', #27890, #42312, #5316, .T. ) ;
#17739 = VERTEX_POINT ( 'NONE', #38897 ) ;
#17741 = CARTESIAN_POINT ( 'NONE',  ( 18.00000000000000355, 0.000000000000000000, 0.000000000000000000 ) ) ;
#17740 = LINE ( 'NONE', #31010, #42742 ) ;
#17742 = EDGE_CURVE ( 'NONE', #3440, #3853, #40170, .T. ) ;
#17743 = CARTESIAN_POINT ( 'NONE',  ( 17.99999999999999645, -103.1672962317654338, 44.09967643725834563 ) ) ;
#17744 = ORIENTED_EDGE ( 'NONE', *, *, #19821, .F. ) ;
#17745 = DIRECTION ( 'NONE',  ( -0.000000000000000000, -0.000000000000000000, 1.000000000000000000 ) ) ;
#17746 = CARTESIAN_POINT ( 'NONE',  ( 6.892732713553924917, 40.00000000000000000, -52.36990085009771434 ) ) ;
#17747 = PRODUCT_DEFINITION_FORMATION_WITH_SPECIFIED_SOURCE ( 'ANY', '', #33245, .NOT_KNOWN. ) ;
#17748 = CARTESIAN_POINT ( 'NONE',  ( 35.58199112951898968, 40.00000000000000000, 46.53705319855855294 ) ) ;
#17749 = AXIS2_PLACEMENT_3D ( 'NONE', #12996, #26302, #23049 ) ;
#17750 = CARTESIAN_POINT ( 'NONE',  ( 18.00000000000000355, -47.49120266317494554, -0.8606222198180160099 ) ) ;
#17751 = DIRECTION ( 'NONE',  ( -1.000000000000000000, -0.000000000000000000, -0.000000000000000000 ) ) ;
#17752 = DIRECTION ( 'NONE',  ( -1.000000000000000000, -0.000000000000000000, -0.000000000000000000 ) ) ;
#17753 = VECTOR ( 'NONE', #40076, 1000.000000000000000 ) ;
#17754 = CARTESIAN_POINT ( 'NONE',  ( -105.9879088449591933, 40.00000000000000711, 4.119280070842334496 ) ) ;
#17755 = CIRCLE ( 'NONE', #4459, 51.99999999999999289 ) ;
#17756 = VERTEX_POINT ( 'NONE', #2435 ) ;
#17757 = CARTESIAN_POINT ( 'NONE',  ( -15.93581279029885422, 40.00000000000000000, -13.96891150189262021 ) ) ;
#17758 = ORIENTED_EDGE ( 'NONE', *, *, #34930, .F. ) ;
#17759 = DIRECTION ( 'NONE',  ( 0.000000000000000000, 0.000000000000000000, 1.000000000000000000 ) ) ;
#17760 = DIRECTION ( 'NONE',  ( 1.000000000000000000, 0.000000000000000000, 0.000000000000000000 ) ) ;
#17761 = ORIENTED_EDGE ( 'NONE', *, *, #15131, .F. ) ;
#17762 = CARTESIAN_POINT ( 'NONE',  ( 17.99999999999999645, 41.33768078145502756, 104.3046912715542902 ) ) ;
#17763 = CIRCLE ( 'NONE', #42088, 120.5010000000000190 ) ;
#17764 = B_SPLINE_CURVE_WITH_KNOTS ( 'NONE', 3,
 ( #22660, #23297, #9306, #9742, #2737 ),
 .UNSPECIFIED., .F., .F.,
 ( 4, 1, 4 ),
 ( 5.640274452250024914E-20, 0.002309401076758505356, 0.004618802153517010713 ),
 .UNSPECIFIED. ) ;
#17765 = DIRECTION ( 'NONE',  ( 0.000000000000000000, 0.8660254037844380415, -0.5000000000000012212 ) ) ;
#17766 = ORIENTED_EDGE ( 'NONE', *, *, #32004, .T. ) ;
#17767 = CARTESIAN_POINT ( 'NONE',  ( 17.99999999999999645, 0.000000000000000000, 0.000000000000000000 ) ) ;
#17768 = ORIENTED_EDGE ( 'NONE', *, *, #40250, .F. ) ;
#17769 = ADVANCED_FACE ( 'NONE', ( #36044 ), #28681, .T. ) ;
#17770 = AXIS2_PLACEMENT_3D ( 'NONE', #5157, #34396, #27440 ) ;
#17771 = ORIENTED_EDGE ( 'NONE', *, *, #8944, .T. ) ;
#17772 = CARTESIAN_POINT ( 'NONE',  ( -9.000000000000005329, 1.356908653455267209E-15, -11.08000000000000007 ) ) ;
#17773 = CARTESIAN_POINT ( 'NONE',  ( 33.43413415811954081, 31.00000000000000355, -67.56680175473152872 ) ) ;
#17774 = ADVANCED_FACE ( 'NONE', ( #2654 ), #41951, .F. ) ;
#17775 = VERTEX_POINT ( 'NONE', #31722 ) ;
#17776 = DIRECTION ( 'NONE',  ( 0.000000000000000000, 0.000000000000000000, 1.000000000000000000 ) ) ;
#17777 = EDGE_CURVE ( 'NONE', #19747, #26478, #25838, .T. ) ;
#17778 = ORIENTED_EDGE ( 'NONE', *, *, #3400, .F. ) ;
#17780 = CIRCLE ( 'NONE', #2347, 2.500000000000000444 ) ;
#17779 = DIRECTION ( 'NONE',  ( 0.000000000000000000, 0.000000000000000000, 1.000000000000000000 ) ) ;
#17781 = VERTEX_POINT ( 'NONE', #28479 ) ;
#17782 = CARTESIAN_POINT ( 'NONE',  ( -82.08563009789774867, 40.00000000000000711, 40.34115885382633593 ) ) ;
#17784 = DIRECTION ( 'NONE',  ( 0.000000000000000000, 0.000000000000000000, 1.000000000000000000 ) ) ;
#17783 = CARTESIAN_POINT ( 'NONE',  ( 18.00000000000000355, 44.47301969247445186, 16.68249143361925491 ) ) ;
#17785 = CARTESIAN_POINT ( 'NONE',  ( 18.00000000000000355, -42.03146605346771025, -22.12489237027361000 ) ) ;
#17786 = DIRECTION ( 'NONE',  ( 1.000000000000000000, 0.000000000000000000, 0.000000000000000000 ) ) ;
#17787 = VECTOR ( 'NONE', #2300, 1000.000000000000000 ) ;
#17788 = EDGE_LOOP ( 'NONE', ( #1503, #43180, #38563, #37309 ) ) ;
#17789 = AXIS2_PLACEMENT_3D ( 'NONE', #17896, #37048, #7151 ) ;
#17790 = CYLINDRICAL_SURFACE ( 'NONE', #3857, 13.59999999999999964 ) ;
#17791 = VECTOR ( 'NONE', #40759, 1000.000000000000000 ) ;
#17792 = CARTESIAN_POINT ( 'NONE',  ( 18.00000000000000355, 13.85708833600031475, -45.43276465116650087 ) ) ;
#17793 = CARTESIAN_POINT ( 'NONE',  ( -68.67288961433401084, 31.00000000000000711, -60.22678404055071155 ) ) ;
#17794 = ADVANCED_FACE ( 'NONE', ( #38676 ), #42379, .F. ) ;
#17795 = CYLINDRICAL_SURFACE ( 'NONE', #5816, 36.00000000000000000 ) ;
#17796 = VERTEX_POINT ( 'NONE', #41742 ) ;
#17797 = EDGE_CURVE ( 'NONE', #12185, #30056, #35415, .T. ) ;
#17798 = VECTOR ( 'NONE', #27000, 1000.000000000000000 ) ;
#17799 = CARTESIAN_POINT ( 'NONE',  ( 22.71825314374767402, 40.00000000000000000, -13.09499307598873941 ) ) ;
#17800 = VECTOR ( 'NONE', #15451, 1000.000000000000000 ) ;
#17801 = VERTEX_POINT ( 'NONE', #32146 ) ;
#17802 = ORIENTED_EDGE ( 'NONE', *, *, #29587, .T. ) ;
#17803 = DIRECTION ( 'NONE',  ( -1.000000000000000000, -0.000000000000000000, -0.000000000000000000 ) ) ;
#17804 = CARTESIAN_POINT ( 'NONE',  ( -100.6569797752917879, -2.055254544495720648, -8.979913733870429127 ) ) ;
#17805 = DIRECTION ( 'NONE',  ( 0.000000000000000000, 0.1590634960190654978, 0.9872683547213455535 ) ) ;
#17806 = DIRECTION ( 'NONE',  ( 0.000000000000000000, 0.000000000000000000, 1.000000000000000000 ) ) ;
#17807 = AXIS2_PLACEMENT_3D ( 'NONE', #28028, #27816, #11658 ) ;
#17808 = VERTEX_POINT ( 'NONE', #12523 ) ;
#17809 = CARTESIAN_POINT ( 'NONE',  ( -103.7695705685748777, -106.4195705685759776, 10.00000000000000000 ) ) ;
#17810 = VERTEX_POINT ( 'NONE', #2227 ) ;
#17811 = CARTESIAN_POINT ( 'NONE',  ( 17.99999999999999645, -101.1249659627859216, 48.60055280209385842 ) ) ;
#17812 = DIRECTION ( 'NONE',  ( -3.009274222672345712E-17, -1.000000000000000000, 2.455023325076455345E-18 ) ) ;
#17813 = DIRECTION ( 'NONE',  ( 0.000000000000000000, 0.9996456111234526265, -0.02662052143777151811 ) ) ;
#17814 = CIRCLE ( 'NONE', #32409, 116.0000000000000000 ) ;
#17815 = DIRECTION ( 'NONE',  ( -1.000000000000000000, -0.000000000000000000, -0.000000000000000000 ) ) ;
#17816 = ORIENTED_EDGE ( 'NONE', *, *, #23452, .T. ) ;
#17817 = VERTEX_POINT ( 'NONE', #22571 ) ;
#17818 = DIRECTION ( 'NONE',  ( 0.000000000000000000, 0.000000000000000000, 1.000000000000000000 ) ) ;
#17819 = CIRCLE ( 'NONE', #21990, 58.99999999999998579 ) ;
#17820 = CARTESIAN_POINT ( 'NONE',  ( 2.164352920501969098E-14, -1.058809993658036520E-13, -40.00000000000000000 ) ) ;
#17821 = EDGE_CURVE ( 'NONE', #42455, #2432, #464, .T. ) ;
#17822 = ORIENTED_EDGE ( 'NONE', *, *, #14745, .T. ) ;
#17823 = AXIS2_PLACEMENT_3D ( 'NONE', #21420, #11790, #8694 ) ;
#17825 = ORIENTED_EDGE ( 'NONE', *, *, #37441, .T. ) ;
#17824 = FACE_OUTER_BOUND ( 'NONE', #38099, .T. ) ;
#17826 = CARTESIAN_POINT ( 'NONE',  ( -5.720710522141557952, 31.00000000000000355, -44.01410879003383059 ) ) ;
#17827 = EDGE_CURVE ( 'NONE', #1103, #4859, #9557, .T. ) ;
#17828 = LINE ( 'NONE', #21551, #23741 ) ;
#17830 = DIRECTION ( 'NONE',  ( 1.000000000000000000, 0.000000000000000000, 0.000000000000000000 ) ) ;
#17829 = CARTESIAN_POINT ( 'NONE',  ( -4.000000000000000000, 0.7924765000094600165, -0.05906175389889745803 ) ) ;
#17831 = CIRCLE ( 'NONE', #33099, 58.99999999999999289 ) ;
#17832 = ORIENTED_EDGE ( 'NONE', *, *, #26088, .F. ) ;
#17833 = CARTESIAN_POINT ( 'NONE',  ( 57.47007747233163144, 39.99999999999999289, -33.06854485814638878 ) ) ;
#17834 = DIRECTION ( 'NONE',  ( 0.000000000000000000, 0.000000000000000000, 1.000000000000000000 ) ) ;
#17835 = UNCERTAINTY_MEASURE_WITH_UNIT (LENGTH_MEASURE( 1.000000000000000082E-05 ), #25202, 'distance_accuracy_value', 'NONE');
#17836 = CARTESIAN_POINT ( 'NONE',  ( 17.99999999999999645, -120.4984140710909202, -0.7894348306996294973 ) ) ;
#17837 = ORIENTED_EDGE ( 'NONE', *, *, #29054, .T. ) ;
#17838 = FACE_OUTER_BOUND ( 'NONE', #25830, .T. ) ;
#17839 = ORIENTED_EDGE ( 'NONE', *, *, #35186, .F. ) ;
#17840 = SURFACE_STYLE_FILL_AREA ( #36841 ) ;
#17841 = AXIS2_PLACEMENT_3D ( 'NONE', #9005, #2646, #2424 ) ;
#17842 = DIRECTION ( 'NONE',  ( -1.000000000000000000, -0.000000000000000000, 0.000000000000000000 ) ) ;
#17843 = DIRECTION ( 'NONE',  ( -1.000000000000000000, -0.000000000000000000, -0.000000000000000000 ) ) ;
#17844 = ADVANCED_FACE ( 'NONE', ( #36250 ), #32779, .F. ) ;
#17845 = CARTESIAN_POINT ( 'NONE',  ( -18.68892229297488683, 31.00000000000000355, 55.06009237583231197 ) ) ;
#17846 = EDGE_CURVE ( 'NONE', #18385, #2814, #9522, .T. ) ;
#17847 = LINE ( 'NONE', #14563, #22604 ) ;
#17848 = VECTOR ( 'NONE', #11265, 1000.000000000000000 ) ;
#17849 = EDGE_LOOP ( 'NONE', ( #39220, #38448, #8234, #36383 ) ) ;
#17850 = ADVANCED_FACE ( 'NONE', ( #3067 ), #10077, .F. ) ;
#17851 = ADVANCED_FACE ( 'NONE', ( #26677 ), #26252, .T. ) ;
#17852 = VECTOR ( 'NONE', #42759, 1000.000000000000000 ) ;
#17853 = AXIS2_PLACEMENT_3D ( 'NONE', #22263, #2959, #13063 ) ;
#17854 = DIRECTION ( 'NONE',  ( -1.000000000000000000, 0.000000000000000000, 0.000000000000000000 ) ) ;
#17855 = ORIENTED_EDGE ( 'NONE', *, *, #2745, .T. ) ;
#17856 = CARTESIAN_POINT ( 'NONE',  ( -29.89583333557403222, 40.00000000000000000, 1.963495399902740690 ) ) ;
#17857 = ORIENTED_EDGE ( 'NONE', *, *, #34845, .T. ) ;
#17859 = AXIS2_PLACEMENT_3D ( 'NONE', #979, #14559, #33953 ) ;
#17858 = DIRECTION ( 'NONE',  ( 0.000000000000000000, -0.9957341762950334685, -0.09226835946331306271 ) ) ;
#17860 = CARTESIAN_POINT ( 'NONE',  ( 0.000000000000000000, 47.00885577955412487, 6.806061952192453468 ) ) ;
#17861 = CARTESIAN_POINT ( 'NONE',  ( -64.43604943162229404, 31.00000000000000711, 49.29347324003089881 ) ) ;
#17863 = CARTESIAN_POINT ( 'NONE',  ( 66.32976035609178211, 39.99999999999999289, 58.33333674018342663 ) ) ;
#17862 = AXIS2_PLACEMENT_3D ( 'NONE', #35417, #5942, #25418 ) ;
#17864 = EDGE_CURVE ( 'NONE', #30173, #2012, #30385, .T. ) ;
#17865 = DIRECTION ( 'NONE',  ( 1.000000000000000000, -1.373900992973641671E-15, -3.895519384649692070E-16 ) ) ;
#17866 = CIRCLE ( 'NONE', #42181, 20.00000000000000711 ) ;
#17867 = EDGE_LOOP ( 'NONE', ( #38223, #34122, #12802, #19783 ) ) ;
#17868 = CARTESIAN_POINT ( 'NONE',  ( -31.74999999999995737, 0.000000000000000000, 0.000000000000000000 ) ) ;
#17869 = ORIENTED_EDGE ( 'NONE', *, *, #4223, .T. ) ;
#17870 = CARTESIAN_POINT ( 'NONE',  ( 17.99999999999999645, -112.5120133921110295, 43.14554256760978745 ) ) ;
#17871 = CARTESIAN_POINT ( 'NONE',  ( 0.000000000000000000, -68.61497464550662073, 99.05794392877581345 ) ) ;
#17873 = ORIENTED_EDGE ( 'NONE', *, *, #2975, .T. ) ;
#17872 = DIRECTION ( 'NONE',  ( 0.02040816326530612776, -0.9997917317482359900, 0.000000000000000000 ) ) ;
#17874 = DIRECTION ( 'NONE',  ( 0.000000000000000000, 0.2113826236296183214, 0.9774033898178677848 ) ) ;
#17875 = ORIENTED_EDGE ( 'NONE', *, *, #40622, .T. ) ;
#17876 = CARTESIAN_POINT ( 'NONE',  ( 17.99999999999999645, 106.5605152861910909, -56.26142179985714620 ) ) ;
#17877 = CARTESIAN_POINT ( 'NONE',  ( 86.04713929520032423, 39.99999999999999289, 42.41619695850760507 ) ) ;
#17878 = DIRECTION ( 'NONE',  ( -1.000000000000000000, -0.000000000000000000, 0.000000000000000000 ) ) ;
#17879 = EDGE_LOOP ( 'NONE', ( #12516, #41285, #27136, #11237 ) ) ;
#17880 = CARTESIAN_POINT ( 'NONE',  ( -3.413765605486552168, -14.29811891091961407, -1.199999999999999956 ) ) ;
#17881 = LINE ( 'NONE', #18531, #38492 ) ;
#17882 = CIRCLE ( 'NONE', #23434, 20.00000000000000355 ) ;
#17883 = CIRCLE ( 'NONE', #31080, 20.00000000000000711 ) ;
#17884 = VECTOR ( 'NONE', #2581, 1000.000000000000000 ) ;
#17885 = VECTOR ( 'NONE', #6695, 1000.000000000000000 ) ;
#17886 = DIRECTION ( 'NONE',  ( -1.000000000000000000, -0.000000000000000000, -0.000000000000000000 ) ) ;
#17887 = ORIENTED_EDGE ( 'NONE', *, *, #31903, .F. ) ;
#17888 = DIRECTION ( 'NONE',  ( -1.000000000000000000, 0.000000000000000000, -0.000000000000000000 ) ) ;
#17889 = ORIENTED_EDGE ( 'NONE', *, *, #7704, .F. ) ;
#17890 = DIRECTION ( 'NONE',  ( 0.000000000000000000, 0.000000000000000000, -1.000000000000000000 ) ) ;
#17891 = CARTESIAN_POINT ( 'NONE',  ( -29.88476798293163128, 40.00000000000000000, 10.10044382456043266 ) ) ;
#17892 =( GEOMETRIC_REPRESENTATION_CONTEXT ( 3 ) GLOBAL_UNCERTAINTY_ASSIGNED_CONTEXT ( ( #42660 ) ) GLOBAL_UNIT_ASSIGNED_CONTEXT ( ( #42139, #8786, #22145 ) ) REPRESENTATION_CONTEXT ( 'NONE', 'WORKASPACE' ) );
#17893 = CARTESIAN_POINT ( 'NONE',  ( 22.90854556226710415, -14.05525454449572997, -74.83297477053821467 ) ) ;
#17894 = CIRCLE ( 'NONE', #3170, 2.649999999999971934 ) ;
#17895 = AXIS2_PLACEMENT_3D ( 'NONE', #6702, #20065, #29636 ) ;
#17896 = CARTESIAN_POINT ( 'NONE',  ( 0.000000000000000000, -28.62203781743013664, 14.19692359621445199 ) ) ;
#17897 = AXIS2_PLACEMENT_3D ( 'NONE', #31001, #10497, #437 ) ;
#17898 = DIRECTION ( 'NONE',  ( 1.000000000000000000, 0.000000000000000000, 0.000000000000000000 ) ) ;
#17899 = ORIENTED_EDGE ( 'NONE', *, *, #20185, .F. ) ;
#17901 = LINE ( 'NONE', #41829, #38043 ) ;
#17900 = CARTESIAN_POINT ( 'NONE',  ( 0.2500000000000002220, 0.000000000000000000, 4.250000000000000000 ) ) ;
#17903 = ORIENTED_EDGE ( 'NONE', *, *, #4733, .T. ) ;
#17902 = AXIS2_PLACEMENT_3D ( 'NONE', #41814, #18106, #31370 ) ;
#17904 = CARTESIAN_POINT ( 'NONE',  ( -12.49999999999998401, -9.428438182424551053E-14, -45.00000000000000000 ) ) ;
#17905 = DIRECTION ( 'NONE',  ( 1.000000000000000000, 0.000000000000000000, 0.000000000000000000 ) ) ;
#17906 = CARTESIAN_POINT ( 'NONE',  ( -19.19493090124598922, 31.00000000000000355, -25.00897302100653263 ) ) ;
#17907 = ORIENTED_EDGE ( 'NONE', *, *, #25867, .T. ) ;
#17908 = DIRECTION ( 'NONE',  ( 1.000000000000000000, 0.000000000000000000, 0.000000000000000000 ) ) ;
#17909 = EDGE_CURVE ( 'NONE', #22945, #32325, #35305, .T. ) ;
#17910 = ADVANCED_FACE ( 'NONE', ( #13599 ), #6373, .T. ) ;
#17911 = FACE_BOUND ( 'NONE', #42096, .T. ) ;
#17912 = ITEM_DEFINED_TRANSFORMATION ( 'NONE', 'NONE', #22632,  #13552 ) ;
#17913 = EDGE_CURVE ( 'NONE', #11528, #20639, #1192, .T. ) ;
#17914 = CARTESIAN_POINT ( 'NONE',  ( 3.999999999999999112, -0.3979232138631231819, -5.929230630780099908E-17 ) ) ;
#17915 = CARTESIAN_POINT ( 'NONE',  ( -77.03666156126601550, 31.00000000000000711, 20.64125776147949409 ) ) ;
#17917 = ORIENTED_EDGE ( 'NONE', *, *, #1603, .F. ) ;
#17916 = CIRCLE ( 'NONE', #42230, 13.60000000000000320 ) ;
#17918 = CARTESIAN_POINT ( 'NONE',  ( -24.78443185005114557, 31.00000000000000355, 32.19086620116432584 ) ) ;
#17919 = AXIS2_PLACEMENT_3D ( 'NONE', #32328, #18663, #5510 ) ;
#17920 = CARTESIAN_POINT ( 'NONE',  ( -11.47416535668642723, 40.00000000000000000, 87.14428777381637303 ) ) ;
#17921 = EDGE_CURVE ( 'NONE', #39845, #14958, #14468, .T. ) ;
#17922 = VECTOR ( 'NONE', #11728, 1000.000000000000000 ) ;
#17923 = AXIS2_PLACEMENT_3D ( 'NONE', #7668, #27325, #24071 ) ;
#17924 = DIRECTION ( 'NONE',  ( 0.000000000000000000, 0.000000000000000000, 1.000000000000000000 ) ) ;
#17925 = ADVANCED_FACE ( 'NONE', ( #16439 ), #20167, .T. ) ;
#17926 = DIRECTION ( 'NONE',  ( -1.000000000000000000, -0.000000000000000000, -0.000000000000000000 ) ) ;
#17927 = DIRECTION ( 'NONE',  ( 0.000000000000000000, 0.000000000000000000, 1.000000000000000000 ) ) ;
#17928 = AXIS2_PLACEMENT_3D ( 'NONE', #38102, #18951, #11743 ) ;
#17930 = ORIENTED_EDGE ( 'NONE', *, *, #4893, .F. ) ;
#17929 = DIRECTION ( 'NONE',  ( 0.000000000000000000, -0.3641605752528102036, -0.9313361774523430947 ) ) ;
#17931 = LINE ( 'NONE', #1289, #19813 ) ;
#17932 = DIRECTION ( 'NONE',  ( 0.000000000000000000, 0.7705132427757861446, 0.6374239897486934092 ) ) ;
#17933 = AXIS2_PLACEMENT_3D ( 'NONE', #28166, #5657, #38592 ) ;
#17934 = ORIENTED_EDGE ( 'NONE', *, *, #13958, .F. ) ;
#17935 = CARTESIAN_POINT ( 'NONE',  ( -30.90996028308246224, 40.00000000000000000, -53.51249422725337013 ) ) ;
#17936 = DIRECTION ( 'NONE',  ( -3.996523416598930318E-16, 2.658563593772947863E-15, 1.000000000000000000 ) ) ;
#17937 = LINE ( 'NONE', #25277, #20753 ) ;
#17938 = VERTEX_POINT ( 'NONE', #2860 ) ;
#17939 = CARTESIAN_POINT ( 'NONE',  ( -1.600000000000000089, -12.75000000000000000, -1.199999999999999956 ) ) ;
#17940 = CARTESIAN_POINT ( 'NONE',  ( 17.99999999999999645, 37.07968990261480968, 109.9140418541958724 ) ) ;
#17941 = AXIS2_PLACEMENT_3D ( 'NONE', #5573, #29568, #35657 ) ;
#17942 = ORIENTED_EDGE ( 'NONE', *, *, #32431, .T. ) ;
#17943 = CARTESIAN_POINT ( 'NONE',  ( -10.00000000000000000, 0.000000000000000000, 0.000000000000000000 ) ) ;
#17944 = ORIENTED_EDGE ( 'NONE', *, *, #1017, .T. ) ;
#17945 = FACE_OUTER_BOUND ( 'NONE', #2036, .T. ) ;
#17946 = ORIENTED_EDGE ( 'NONE', *, *, #8889, .F. ) ;
#17947 = FACE_OUTER_BOUND ( 'NONE', #3693, .T. ) ;
#17948 = CARTESIAN_POINT ( 'NONE',  ( 17.99999999999999645, 104.2166695095712470, 60.49278301857841456 ) ) ;
#17949 = ORIENTED_EDGE ( 'NONE', *, *, #13407, .F. ) ;
#17950 = VECTOR ( 'NONE', #23325, 1000.000000000000114 ) ;
#17951 = CARTESIAN_POINT ( 'NONE',  ( 22.90854556226710415, -12.05525454449572464, -74.83297477053821467 ) ) ;
#17952 = CYLINDRICAL_SURFACE ( 'NONE', #19242, 120.5010000000000190 ) ;
#17953 = ORIENTED_EDGE ( 'NONE', *, *, #26578, .F. ) ;
#17954 = AXIS2_PLACEMENT_3D ( 'NONE', #21086, #34551, #30656 ) ;
#17955 = CARTESIAN_POINT ( 'NONE',  ( 18.00000000000000355, -35.20873326984057883, -31.88259874184068465 ) ) ;
#17957 = LINE ( 'NONE', #2164, #1106 ) ;
#17956 = AXIS2_PLACEMENT_3D ( 'NONE', #17820, #37187, #7741 ) ;
#17958 = ORIENTED_EDGE ( 'NONE', *, *, #8266, .T. ) ;
#17959 = FACE_OUTER_BOUND ( 'NONE', #4790, .T. ) ;
#17960 = VECTOR ( 'NONE', #3364, 1000.000000000000000 ) ;
#17961 = EDGE_CURVE ( 'NONE', #34610, #10833, #29783, .T. ) ;
#17962 = CARTESIAN_POINT ( 'NONE',  ( -2.600000000000000533, -12.75000000000000000, 0.000000000000000000 ) ) ;
#17963 = EDGE_LOOP ( 'NONE', ( #7202, #11912, #31365, #24997 ) ) ;
#17964 = DIRECTION ( 'NONE',  ( 4.329780281177459034E-17, 1.000000000000000000, -4.329780281177474441E-17 ) ) ;
#17965 = AXIS2_PLACEMENT_3D ( 'NONE', #34804, #30527, #7966 ) ;
#17966 = CARTESIAN_POINT ( 'NONE',  ( 0.000000000000000000, -26.17370628620627571, -39.63700417846190049 ) ) ;
#17967 = CARTESIAN_POINT ( 'NONE',  ( 41.10549127292548377, 31.00000000000000355, 20.25863663968860706 ) ) ;
#17968 = ORIENTED_EDGE ( 'NONE', *, *, #19133, .F. ) ;
#17970 = DIRECTION ( 'NONE',  ( 1.000000000000000000, 0.000000000000000000, 0.000000000000000000 ) ) ;
#17969 = CARTESIAN_POINT ( 'NONE',  ( -10.00000000000000000, 0.000000000000000000, 0.000000000000000000 ) ) ;
#17971 = CIRCLE ( 'NONE', #38802, 2.500000000000002665 ) ;
#17972 = DIRECTION ( 'NONE',  ( -1.000000000000000000, 0.000000000000000000, 0.000000000000000000 ) ) ;
#17973 = ORIENTED_EDGE ( 'NONE', *, *, #6483, .T. ) ;
#17974 = ADVANCED_FACE ( 'NONE', ( #32986 ), #29742, .F. ) ;
#17975 = DIRECTION ( 'NONE',  ( -1.000000000000000000, 0.000000000000000000, 0.000000000000000000 ) ) ;
#17976 = CARTESIAN_POINT ( 'NONE',  ( 15.14372185054182651, 40.00000000000000000, 44.57714859939663654 ) ) ;
#17977 = CARTESIAN_POINT ( 'NONE',  ( -50.71442127988192539, 40.00000000000000000, -13.67646662467582352 ) ) ;
#17978 = EDGE_CURVE ( 'NONE', #18607, #13782, #31187, .T. ) ;
#17979 = DIRECTION ( 'NONE',  ( 0.000000000000000000, 0.000000000000000000, 1.000000000000000000 ) ) ;
#17980 = ADVANCED_FACE ( 'NONE', ( #6580 ), #17097, .T. ) ;
#17981 = CARTESIAN_POINT ( 'NONE',  ( 17.99999999999999645, -64.58410930313591791, 101.7319213743680422 ) ) ;
#17982 = AXIS2_PLACEMENT_3D ( 'NONE', #28265, #34345, #41309 ) ;
#17983 = DIRECTION ( 'NONE',  ( 0.000000000000000000, 0.1837495178165706455, -0.9829730996839017854 ) ) ;
#17984 = CARTESIAN_POINT ( 'NONE',  ( -15.93581279029885422, 31.00000000000000355, -13.96891150189262021 ) ) ;
#17985 = AXIS2_PLACEMENT_3D ( 'NONE', #20587, #17751, #887 ) ;
#17986 = AXIS2_PLACEMENT_3D ( 'NONE', #41709, #42340, #21694 ) ;
#17987 = VERTEX_POINT ( 'NONE', #23215 ) ;
#17988 = CARTESIAN_POINT ( 'NONE',  ( -33.98628324864968420, 40.00000000000000000, 19.63407011443918293 ) ) ;
#17989 = VERTEX_POINT ( 'NONE', #23648 ) ;
#17990 = DIRECTION ( 'NONE',  ( 1.000000000000000000, 0.000000000000000000, 0.000000000000000000 ) ) ;
#17991 = DIRECTION ( 'NONE',  ( -1.000000000000000000, -0.000000000000000000, 0.000000000000000000 ) ) ;
#17992 = VECTOR ( 'NONE', #43079, 1000.000000000000000 ) ;
#17993 = AXIS2_PLACEMENT_3D ( 'NONE', #8819, #18906, #28906 ) ;
#17994 = ORIENTED_EDGE ( 'NONE', *, *, #37018, .T. ) ;
#17995 = CIRCLE ( 'NONE', #23545, 47.49900000000000944 ) ;
#17996 = DIRECTION ( 'NONE',  ( 0.000000000000000000, 0.000000000000000000, 1.000000000000000000 ) ) ;
#17997 = DIRECTION ( 'NONE',  ( 1.000000000000000000, 0.000000000000000000, 0.000000000000000000 ) ) ;
#17998 = ORIENTED_EDGE ( 'NONE', *, *, #14090, .T. ) ;
#17999 = CYLINDRICAL_SURFACE ( 'NONE', #38818, 59.00000000000000000 ) ;
#18000 = VERTEX_POINT ( 'NONE', #19944 ) ;
#18001 = ADVANCED_FACE ( 'NONE', ( #36908 ), #3298, .F. ) ;
#18002 = EDGE_CURVE ( 'NONE', #9695, #39040, #42301, .T. ) ;
#18003 = ORIENTED_EDGE ( 'NONE', *, *, #15687, .T. ) ;
#18004 = DIRECTION ( 'NONE',  ( 0.000000000000000000, -0.9407002666710364558, 0.3392388661180213427 ) ) ;
#18005 = CARTESIAN_POINT ( 'NONE',  ( 74.90833963775308746, 31.00000000000000000, 20.17845691862754975 ) ) ;
#18007 = EDGE_CURVE ( 'NONE', #30050, #23276, #24072, .T. ) ;
#18006 = VERTEX_POINT ( 'NONE', #40593 ) ;
#18008 = DIRECTION ( 'NONE',  ( 0.000000000000000000, 0.000000000000000000, 1.000000000000000000 ) ) ;
#18009 = SHAPE_REPRESENTATION ( 'socket head cap screw_iso_ISO 4762 M5 x 16 - 16N', ( #13552 ), #2321 ) ;
#18010 = CARTESIAN_POINT ( 'NONE',  ( 0.000000000000000000, 0.000000000000000000, 0.000000000000000000 ) ) ;
#18011 = ORIENTED_EDGE ( 'NONE', *, *, #20236, .T. ) ;
#18012 = DIRECTION ( 'NONE',  ( 0.000000000000000000, 0.000000000000000000, 1.000000000000000000 ) ) ;
#18013 = PRODUCT_DEFINITION_SHAPE ( 'NONE', 'NONE',  #43209 ) ;
#18014 = ORIENTED_EDGE ( 'NONE', *, *, #20397, .T. ) ;
#18015 = CARTESIAN_POINT ( 'NONE',  ( 11.57239447660066567, 40.00000000000000000, 88.72710294830137912 ) ) ;
#18016 = CARTESIAN_POINT ( 'NONE',  ( -6.237032369604345483, 31.00000000000000355, -23.31551866006812190 ) ) ;
#18017 = CIRCLE ( 'NONE', #15901, 59.00000000000001421 ) ;
#18019 = PLANE ( 'NONE',  #22170 ) ;
#18018 = CYLINDRICAL_SURFACE ( 'NONE', #30118, 15.00000000000000000 ) ;
#18020 = DIRECTION ( 'NONE',  ( 0.000000000000000000, 0.000000000000000000, -1.000000000000000000 ) ) ;
#18021 = CARTESIAN_POINT ( 'NONE',  ( 17.99999999999999645, 17.33727698085173330, 110.8498592715974098 ) ) ;
#18022 = AXIS2_PLACEMENT_3D ( 'NONE', #19886, #32727, #2808 ) ;
#18023 = EDGE_CURVE ( 'NONE', #6599, #10153, #32562, .T. ) ;
#18024 = ORIENTED_EDGE ( 'NONE', *, *, #33627, .F. ) ;
#18025 = AXIS2_PLACEMENT_3D ( 'NONE', #10932, #14425, #21206 ) ;
#18026 = CIRCLE ( 'NONE', #2588, 4.000000000000000000 ) ;
#18027 = VECTOR ( 'NONE', #13879, 1000.000000000000000 ) ;
#18028 = ORIENTED_EDGE ( 'NONE', *, *, #7152, .T. ) ;
#18029 = DIRECTION ( 'NONE',  ( 0.000000000000000000, 0.000000000000000000, -1.000000000000000000 ) ) ;
#18030 = CARTESIAN_POINT ( 'NONE',  ( 63.67823170517923614, 31.00000000000000000, 72.58713758494482704 ) ) ;
#18031 = DIRECTION ( 'NONE',  ( -0.9914448613738104932, -0.1305261922200512681, 0.000000000000000000 ) ) ;
#18033 = EDGE_LOOP ( 'NONE', ( #33969, #21323, #2251, #9834 ) ) ;
#18032 = AXIS2_PLACEMENT_3D ( 'NONE', #26208, #35768, #32309 ) ;
#18034 = CARTESIAN_POINT ( 'NONE',  ( -32.09999204393464822, 40.00000000000000000, -2.147948991655045159 ) ) ;
#18035 = EDGE_CURVE ( 'NONE', #7030, #11794, #27992, .T. ) ;
#18036 = ORIENTED_EDGE ( 'NONE', *, *, #18277, .T. ) ;
#18037 = AXIS2_PLACEMENT_3D ( 'NONE', #40468, #36780, #14117 ) ;
#18038 = ORIENTED_EDGE ( 'NONE', *, *, #33064, .T. ) ;
#18039 = CARTESIAN_POINT ( 'NONE',  ( 17.99999999999999645, 34.45183346761135113, 10.44371441202667761 ) ) ;
#18040 = LINE ( 'NONE', #1600, #31153 ) ;
#18041 = DIRECTION ( 'NONE',  ( -1.000000000000000000, -0.000000000000000000, -0.000000000000000000 ) ) ;
#18042 = DIRECTION ( 'NONE',  ( -1.058513553088275437E-16, -1.000000000000000000, 8.813324511995299047E-17 ) ) ;
#18043 = VERTEX_POINT ( 'NONE', #24303 ) ;
#18044 = CARTESIAN_POINT ( 'NONE',  ( 17.99999999999999645, 0.000000000000000000, 36.00000000000000000 ) ) ;
#18045 = ORIENTED_EDGE ( 'NONE', *, *, #1593, .T. ) ;
#18046 = DIRECTION ( 'NONE',  ( -1.000000000000000000, 0.000000000000000000, 0.000000000000000000 ) ) ;
#18047 = CYLINDRICAL_SURFACE ( 'NONE', #6748, 51.99999999999999289 ) ;
#18048 = DIRECTION ( 'NONE',  ( 1.000000000000000000, 0.000000000000000000, 0.000000000000000000 ) ) ;
#18049 = DIRECTION ( 'NONE',  ( -1.000000000000000000, -0.000000000000000000, -0.000000000000000000 ) ) ;
#18050 = ORIENTED_EDGE ( 'NONE', *, *, #18007, .T. ) ;
#18051 = ORIENTED_EDGE ( 'NONE', *, *, #24425, .T. ) ;
#18052 = CARTESIAN_POINT ( 'NONE',  ( 0.000000000000000000, -94.83915810436360516, -59.94836581341685644 ) ) ;
#18053 = FACE_BOUND ( 'NONE', #11607, .T. ) ;
#18054 = CIRCLE ( 'NONE', #10336, 31.49899999999999878 ) ;
#18055 = CIRCLE ( 'NONE', #25697, 59.00000000000002132 ) ;
#18056 = EDGE_CURVE ( 'NONE', #7995, #11400, #37414, .T. ) ;
#18057 = AXIS2_PLACEMENT_3D ( 'NONE', #4395, #4621, #40607 ) ;
#18058 = EDGE_LOOP ( 'NONE', ( #8612, #477, #7075, #42944 ) ) ;
#18060 = ORIENTED_EDGE ( 'NONE', *, *, #31338, .T. ) ;
#18059 = DIRECTION ( 'NONE',  ( 0.000000000000000000, 0.000000000000000000, 1.000000000000000000 ) ) ;
#18061 = CARTESIAN_POINT ( 'NONE',  ( -10.41556553088919834, 31.00000000000000355, 38.62046602036556209 ) ) ;
#18062 = EDGE_CURVE ( 'NONE', #30860, #13871, #31023, .T. ) ;
#18063 = CARTESIAN_POINT ( 'NONE',  ( 0.000000000000000000, 106.6051926090976991, -45.73109345704713036 ) ) ;
#18064 = AXIS2_PLACEMENT_3D ( 'NONE', #39804, #40013, #6232 ) ;
#18066 = DIRECTION ( 'NONE',  ( -1.000000000000000000, -0.000000000000000000, -0.000000000000000000 ) ) ;
#18065 = DIRECTION ( 'NONE',  ( 0.000000000000000000, 0.000000000000000000, 1.000000000000000000 ) ) ;
#18067 = VERTEX_POINT ( 'NONE', #7884 ) ;
#18068 = CARTESIAN_POINT ( 'NONE',  ( -8.920000000000003482, 1.827173024327850982E-15, -14.91999999999999815 ) ) ;
#18069 = CARTESIAN_POINT ( 'NONE',  ( -4.113979049837106494, 40.00000000000000000, -64.40000927351898952 ) ) ;
#18070 = CARTESIAN_POINT ( 'NONE',  ( 2.039745330509125010E-13, -150.5000000000013642, 6.999999999999586109 ) ) ;
#18071 = DIRECTION ( 'NONE',  ( 0.000000000000000000, -0.8747630845319559478, -0.4845508703326599775 ) ) ;
#18072 = ORIENTED_EDGE ( 'NONE', *, *, #24701, .F. ) ;
#18073 = DIRECTION ( 'NONE',  ( -1.000000000000000000, 0.000000000000000000, 0.000000000000000000 ) ) ;
#18074 = ADVANCED_FACE ( 'NONE', ( #34727 ), #34076, .F. ) ;
#18075 = VERTEX_POINT ( 'NONE', #24726 ) ;
#18076 = LINE ( 'NONE', #38081, #30196 ) ;
#18077 = DIRECTION ( 'NONE',  ( -3.996523416598930318E-16, 2.658563593772947863E-15, 1.000000000000000000 ) ) ;
#18078 = CARTESIAN_POINT ( 'NONE',  ( -59.82155519080263417, 31.00000000000000711, -7.874468279917395286 ) ) ;
#18079 = CARTESIAN_POINT ( 'NONE',  ( 0.000000000000000000, -11.49545354908957862, 29.80986809967256335 ) ) ;
#18080 = AXIS2_PLACEMENT_3D ( 'NONE', #31421, #18153, #14854 ) ;
#18081 = ORIENTED_EDGE ( 'NONE', *, *, #39567, .T. ) ;
#18082 = CIRCLE ( 'NONE', #36134, 59.00000000000001421 ) ;
#18083 = CARTESIAN_POINT ( 'NONE',  ( 8.999999999999998224, -19.47322409167248480, -30.27859877001420941 ) ) ;
#18084 = ADVANCED_FACE ( 'NONE', ( #18194 ), #37559, .F. ) ;
#18085 = ORIENTED_EDGE ( 'NONE', *, *, #15250, .F. ) ;
#18086 = LINE ( 'NONE', #31348, #34004 ) ;
#18087 = EDGE_CURVE ( 'NONE', #7056, #38197, #34496, .T. ) ;
#18088 = CARTESIAN_POINT ( 'NONE',  ( 0.000000000000000000, 38.92705108641770551, -27.21837053747755419 ) ) ;
#18089 = CARTESIAN_POINT ( 'NONE',  ( 56.68048384767583769, 31.00000000000000000, -64.44707192207098956 ) ) ;
#18090 = CARTESIAN_POINT ( 'NONE',  ( 86.62806645044916820, 39.99999999999999289, 11.52843970785434990 ) ) ;
#18091 = DIRECTION ( 'NONE',  ( 1.000000000000000000, 0.000000000000000000, 0.000000000000000000 ) ) ;
#18092 = ORIENTED_EDGE ( 'NONE', *, *, #18007, .F. ) ;
#18093 = CYLINDRICAL_SURFACE ( 'NONE', #10978, 20.00000000000000711 ) ;
#18094 = ORIENTED_EDGE ( 'NONE', *, *, #32544, .T. ) ;
#18095 = DIRECTION ( 'NONE',  ( -1.000000000000000000, -0.000000000000000000, 0.000000000000000000 ) ) ;
#18096 = CARTESIAN_POINT ( 'NONE',  ( 17.99999999999999645, -16.77566611177701006, -119.3275660838943963 ) ) ;
#18098 = VERTEX_POINT ( 'NONE', #21471 ) ;
#18097 = CARTESIAN_POINT ( 'NONE',  ( 0.000000000000000000, 42.41764978026606769, 20.20639853260304619 ) ) ;
#18099 = DIRECTION ( 'NONE',  ( 1.000000000000000000, 0.000000000000000000, 0.000000000000000000 ) ) ;
#18100 = EDGE_LOOP ( 'NONE', ( #42659, #22491, #41255, #39485 ) ) ;
#18101 = DIRECTION ( 'NONE',  ( 0.02040816326530612776, 0.9997917317482359900, -0.000000000000000000 ) ) ;
#18102 = CARTESIAN_POINT ( 'NONE',  ( 41.30831894254264824, 40.00000000000000000, -83.80005689411834169 ) ) ;
#18103 = DIRECTION ( 'NONE',  ( -1.000000000000000000, 0.000000000000000000, 0.000000000000000000 ) ) ;
#18104 = ORIENTED_EDGE ( 'NONE', *, *, #9119, .T. ) ;
#18105 = EDGE_CURVE ( 'NONE', #7775, #10843, #31869, .T. ) ;
#18106 = DIRECTION ( 'NONE',  ( -1.000000000000000000, -0.000000000000000000, -0.000000000000000000 ) ) ;
#18108 = EDGE_CURVE ( 'NONE', #1020, #8971, #24959, .T. ) ;
#18107 = CIRCLE ( 'NONE', #37539, 13.60000000000000497 ) ;
#18109 = DIRECTION ( 'NONE',  ( 0.000000000000000000, 0.000000000000000000, -1.000000000000000000 ) ) ;
#18110 = AXIS2_PLACEMENT_3D ( 'NONE', #11518, #8237, #18312 ) ;
#18111 = EDGE_CURVE ( 'NONE', #24063, #33745, #15208, .T. ) ;
#18112 = EDGE_CURVE ( 'NONE', #5268, #6410, #26294, .T. ) ;
#18113 = AXIS2_PLACEMENT_3D ( 'NONE', #18202, #14040, #27998 ) ;
#18115 = CARTESIAN_POINT ( 'NONE',  ( 12.40854556226731198, -35.35525454449573601, -74.83297477053802993 ) ) ;
#18114 = DIRECTION ( 'NONE',  ( 1.000000000000000000, -1.373900992973641671E-15, -3.895519384649692070E-16 ) ) ;
#18116 = ORIENTED_EDGE ( 'NONE', *, *, #21265, .F. ) ;
#18117 = DIRECTION ( 'NONE',  ( 1.000000000000000000, 0.000000000000000000, 0.000000000000000000 ) ) ;
#18118 = ORIENTED_EDGE ( 'NONE', *, *, #6428, .T. ) ;
#18119 = CARTESIAN_POINT ( 'NONE',  ( 18.00000000000000355, 0.000000000000000000, 0.000000000000000000 ) ) ;
#18120 = CARTESIAN_POINT ( 'NONE',  ( -8.786317949316114095, 40.00000000000000000, -33.00646673686679833 ) ) ;
#18121 = DIRECTION ( 'NONE',  ( -1.000000000000000000, 0.000000000000000000, 0.000000000000000000 ) ) ;
#18122 = DIRECTION ( 'NONE',  ( 0.000000000000000000, 0.000000000000000000, 1.000000000000000000 ) ) ;
#18123 = DIRECTION ( 'NONE',  ( 0.000000000000000000, -0.9048270524660235736, 0.4257792915650641108 ) ) ;
#18124 = VERTEX_POINT ( 'NONE', #40817 ) ;
#18126 = CARTESIAN_POINT ( 'NONE',  ( 0.000000000000000000, 0.2227391519123156360, -46.98410307550729215 ) ) ;
#18125 = CARTESIAN_POINT ( 'NONE',  ( 0.000000000000000000, 103.5682682299988500, -43.14958040911561454 ) ) ;
#18127 = ORIENTED_EDGE ( 'NONE', *, *, #35189, .F. ) ;
#18128 = CARTESIAN_POINT ( 'NONE',  ( -150.4999999999986926, -3.000858968969551636E-13, 7.000000000000042633 ) ) ;
#18129 = CARTESIAN_POINT ( 'NONE',  ( 17.99999999999999645, -80.02407177072905142, -78.64108602300026973 ) ) ;
#18130 = CARTESIAN_POINT ( 'NONE',  ( -14.08558183832706234, 31.00000000000000355, -28.55406316770863739 ) ) ;
#18131 = ORIENTED_EDGE ( 'NONE', *, *, #8110, .T. ) ;
#18132 = DIRECTION ( 'NONE',  ( 0.000000000000000000, 1.000000000000000000, 0.000000000000000000 ) ) ;
#18133 = DIRECTION ( 'NONE',  ( 0.000000000000000000, 0.3612416661871471479, 0.9324722294043580328 ) ) ;
#18134 = CARTESIAN_POINT ( 'NONE',  ( -12.50000000000000000, 1.530808498934191521E-15, -20.00000000000000000 ) ) ;
#18135 = EDGE_CURVE ( 'NONE', #9576, #22696, #37982, .T. ) ;
#18136 = CARTESIAN_POINT ( 'NONE',  ( -79.27599250299880396, 31.00000000000000711, 10.45126230984107707 ) ) ;
#18137 = AXIS2_PLACEMENT_3D ( 'NONE', #41614, #28763, #5814 ) ;
#18138 = VERTEX_POINT ( 'NONE', #1549 ) ;
#18139 = CIRCLE ( 'NONE', #20209, 10.99999999999999645 ) ;
#18140 = CARTESIAN_POINT ( 'NONE',  ( 56.89991739620084132, 31.00000000000000355, -3.630084216720528278 ) ) ;
#18141 = CARTESIAN_POINT ( 'NONE',  ( -29.64342647699677613, 40.00000000000000000, -87.27882330658468391 ) ) ;
#18142 = CIRCLE ( 'NONE', #11131, 20.00000000000000711 ) ;
#18143 = ORIENTED_EDGE ( 'NONE', *, *, #9275, .F. ) ;
#18144 = DIRECTION ( 'NONE',  ( -1.000000000000000000, 0.000000000000000000, 0.000000000000000000 ) ) ;
#18145 = CARTESIAN_POINT ( 'NONE',  ( 0.000000000000000000, -84.09610293794118263, 74.27057253242982426 ) ) ;
#18146 = DIRECTION ( 'NONE',  ( 0.000000000000000000, 0.000000000000000000, 1.000000000000000000 ) ) ;
#18148 = VERTEX_POINT ( 'NONE', #7669 ) ;
#18147 = DIRECTION ( 'NONE',  ( 1.000000000000000000, -0.000000000000000000, 0.000000000000000000 ) ) ;
#18149 = FACE_OUTER_BOUND ( 'NONE', #36713, .T. ) ;
#18150 = CARTESIAN_POINT ( 'NONE',  ( 2.500000000000000000, 0.000000000000000000, 0.000000000000000000 ) ) ;
#18151 = ORIENTED_EDGE ( 'NONE', *, *, #1766, .T. ) ;
#18152 = CARTESIAN_POINT ( 'NONE',  ( 38.75409931461306456, 40.00000000000000000, -50.52625141960567134 ) ) ;
#18153 = DIRECTION ( 'NONE',  ( -1.000000000000000000, 0.000000000000000000, -0.000000000000000000 ) ) ;
#18154 = ORIENTED_EDGE ( 'NONE', *, *, #2954, .T. ) ;
#18155 = DIRECTION ( 'NONE',  ( -1.000000000000000000, -0.000000000000000000, 0.000000000000000000 ) ) ;
#18156 = CYLINDRICAL_SURFACE ( 'NONE', #34055, 13.40000000000000213 ) ;
#18157 = EDGE_CURVE ( 'NONE', #31298, #20435, #15169, .T. ) ;
#18158 = EDGE_CURVE ( 'NONE', #27914, #7995, #7228, .T. ) ;
#18159 = ORIENTED_EDGE ( 'NONE', *, *, #7680, .F. ) ;
#18160 = FACE_OUTER_BOUND ( 'NONE', #30021, .T. ) ;
#18161 = ORIENTED_EDGE ( 'NONE', *, *, #15410, .T. ) ;
#18162 = EDGE_CURVE ( 'NONE', #18006, #12660, #7458, .T. ) ;
#18163 = DIRECTION ( 'NONE',  ( -1.000000000000000000, 0.000000000000000000, 0.000000000000000000 ) ) ;
#18165 = ORIENTED_EDGE ( 'NONE', *, *, #7822, .F. ) ;
#18164 = CIRCLE ( 'NONE', #34115, 116.0000000000000000 ) ;
#18166 = DIRECTION ( 'NONE',  ( -1.000000000000000000, -0.000000000000000000, 0.000000000000000000 ) ) ;
#18167 = AXIS2_PLACEMENT_3D ( 'NONE', #783, #6699, #27432 ) ;
#18168 = CARTESIAN_POINT ( 'NONE',  ( -101.1468392227577340, 31.00000000000000711, 13.20405500233197671 ) ) ;
#18169 = ORIENTED_EDGE ( 'NONE', *, *, #10827, .T. ) ;
#18170 = AXIS2_PLACEMENT_3D ( 'NONE', #42343, #38861, #42119 ) ;
#18171 = CARTESIAN_POINT ( 'NONE',  ( 18.00000000000000355, 49.65209126885762458, 15.44894276735567651 ) ) ;
#18172 = CARTESIAN_POINT ( 'NONE',  ( 17.99999999999999645, 114.1157422997285806, -20.82300072952825332 ) ) ;
#18173 = ORIENTED_EDGE ( 'NONE', *, *, #36562, .T. ) ;
#18174 = DIRECTION ( 'NONE',  ( 0.000000000000000000, 0.000000000000000000, 1.000000000000000000 ) ) ;
#18175 = CARTESIAN_POINT ( 'NONE',  ( 0.000000000000000000, -43.55304910509424587, 28.41006711799970219 ) ) ;
#18176 = EDGE_CURVE ( 'NONE', #7568, #41800, #23537, .T. ) ;
#18177 = ORIENTED_EDGE ( 'NONE', *, *, #34171, .T. ) ;
#18178 = CARTESIAN_POINT ( 'NONE',  ( 0.000000000000000000, -11.41303419185048185, 111.6154788735835410 ) ) ;
#18179 = DIRECTION ( 'NONE',  ( 1.000000000000000000, 0.000000000000000000, 0.000000000000000000 ) ) ;
#18180 = APPLICATION_PROTOCOL_DEFINITION ( 'draft international standard', 'automotive_design', 1998, #27897 ) ;
#18181 = FACE_OUTER_BOUND ( 'NONE', #6202, .T. ) ;
#18182 = CARTESIAN_POINT ( 'NONE',  ( 52.83624534446448706, 31.00000000000000355, -14.15919354876300318 ) ) ;
#18183 = VERTEX_POINT ( 'NONE', #35360 ) ;
#18185 = CARTESIAN_POINT ( 'NONE',  ( 17.99999999999999645, 61.59243992711459015, 93.77976230226062171 ) ) ;
#18184 = DIRECTION ( 'NONE',  ( 1.000000000000000000, 0.000000000000000000, 0.000000000000000000 ) ) ;
#18186 = DIRECTION ( 'NONE',  ( 0.000000000000000000, 0.9996456111234524045, 0.02662052143777824190 ) ) ;
#18187 = ORIENTED_EDGE ( 'NONE', *, *, #33060, .T. ) ;
#18188 = DIRECTION ( 'NONE',  ( 0.000000000000000000, 0.000000000000000000, 1.000000000000000000 ) ) ;
#18189 = CARTESIAN_POINT ( 'NONE',  ( 55.10416666547021691, 40.00000000000000000, 3.599741573803287853 ) ) ;
#18190 = CARTESIAN_POINT ( 'NONE',  ( -40.14822235766499148, 40.00000000000000000, 45.62378674120105160 ) ) ;
#18191 = VECTOR ( 'NONE', #18147, 1000.000000000000000 ) ;
#18192 = CIRCLE ( 'NONE', #3471, 116.0000000000000000 ) ;
#18193 = DIRECTION ( 'NONE',  ( -3.996523416598930318E-16, 2.658563593772947863E-15, 1.000000000000000000 ) ) ;
#18194 = FACE_OUTER_BOUND ( 'NONE', #4143, .T. ) ;
#18195 = CIRCLE ( 'NONE', #40418, 59.00000000000000711 ) ;
#18196 = AXIS2_PLACEMENT_3D ( 'NONE', #18150, #11567, #4553 ) ;
#18197 = DIRECTION ( 'NONE',  ( 1.000000000000000000, -0.000000000000000000, 0.000000000000000000 ) ) ;
#18198 = CARTESIAN_POINT ( 'NONE',  ( 1.472621547668719444, 31.00000000000000355, -22.60416666365413718 ) ) ;
#18199 = ORIENTED_EDGE ( 'NONE', *, *, #2, .T. ) ;
#18200 = CARTESIAN_POINT ( 'NONE',  ( -20.72449291656876369, 40.00000000000000000, -23.61699481730619610 ) ) ;
#18201 = ORIENTED_EDGE ( 'NONE', *, *, #35565, .T. ) ;
#18202 = CARTESIAN_POINT ( 'NONE',  ( -8.749793197483592522, 117.9447454555042754, 2.972870684497274762 ) ) ;
#18203 = CARTESIAN_POINT ( 'NONE',  ( 0.000000000000000000, -107.2703412112692689, -32.88383143828572486 ) ) ;
#18204 = ORIENTED_EDGE ( 'NONE', *, *, #39768, .T. ) ;
#18205 = DIRECTION ( 'NONE',  ( -1.000000000000000000, 0.000000000000000000, -0.000000000000000000 ) ) ;
#18206 = ADVANCED_FACE ( 'NONE', ( #5890 ), #2179, .F. ) ;
#18207 = CARTESIAN_POINT ( 'NONE',  ( 17.99999999999999645, 0.000000000000000000, 0.000000000000000000 ) ) ;
#18208 = ORIENTED_EDGE ( 'NONE', *, *, #19227, .F. ) ;
#18209 = DIRECTION ( 'NONE',  ( 0.000000000000000000, -0.5076658003388468954, 0.8615540813938020737 ) ) ;
#18210 = EDGE_LOOP ( 'NONE', ( #6912, #20837, #9292, #10103 ) ) ;
#18211 = VERTEX_POINT ( 'NONE', #25163 ) ;
#18212 = DIRECTION ( 'NONE',  ( 1.000000000000000000, 0.000000000000000000, 0.000000000000000000 ) ) ;
#18214 = AXIS2_PLACEMENT_3D ( 'NONE', #43167, #10233, #20311 ) ;
#18213 = CARTESIAN_POINT ( 'NONE',  ( -55.03444096782886419, 31.00000000000000355, -48.41538206856125015 ) ) ;
#18215 = ORIENTED_EDGE ( 'NONE', *, *, #27419, .F. ) ;
#18216 = CARTESIAN_POINT ( 'NONE',  ( 0.000000000000000000, 0.000000000000000000, 0.000000000000000000 ) ) ;
#18217 = CIRCLE ( 'NONE', #17485, 51.99999999999999289 ) ;
#18218 = CARTESIAN_POINT ( 'NONE',  ( 3.678949249685231848, 0.000000000000000000, 0.000000000000000000 ) ) ;
#18219 = ORIENTED_EDGE ( 'NONE', *, *, #19467, .T. ) ;
#18220 = EDGE_CURVE ( 'NONE', #5342, #35630, #35338, .T. ) ;
#18221 = CYLINDRICAL_SURFACE ( 'NONE', #19663, 10.99999999999999645 ) ;
#18222 = ORIENTED_EDGE ( 'NONE', *, *, #40965, .T. ) ;
#18223 = CARTESIAN_POINT ( 'NONE',  ( 39.23423008407738877, 40.00000000000000000, 79.83814995801118641 ) ) ;
#18224 = AXIS2_PLACEMENT_3D ( 'NONE', #25714, #38966, #25912 ) ;
#18225 = AXIS2_PLACEMENT_3D ( 'NONE', #40409, #36714, #17122 ) ;
#18226 = CARTESIAN_POINT ( 'NONE',  ( -21.37212791037561388, 31.00000000000000355, -7.253704819187424491 ) ) ;
#18227 = EDGE_CURVE ( 'NONE', #24053, #25660, #40895, .T. ) ;
#18228 = AXIS2_PLACEMENT_3D ( 'NONE', #37046, #3215, #6937 ) ;
#18230 = FACE_OUTER_BOUND ( 'NONE', #42936, .T. ) ;
#18229 = CYLINDRICAL_SURFACE ( 'NONE', #24573, 36.00000000000000000 ) ;
#18231 = AXIS2_PLACEMENT_3D ( 'NONE', #42921, #39005, #6071 ) ;
#18232 = ADVANCED_FACE ( 'NONE', ( #8967 ), #18628, .T. ) ;
#18233 = DIRECTION ( 'NONE',  ( 1.000000000000000000, 0.000000000000000000, 0.000000000000000000 ) ) ;
#18234 = CARTESIAN_POINT ( 'NONE',  ( 18.00000000000000355, 27.43636312076321104, 38.14186064215159888 ) ) ;
#18235 = ORIENTED_EDGE ( 'NONE', *, *, #7526, .T. ) ;
#18236 = DIRECTION ( 'NONE',  ( -1.000000000000000000, -0.000000000000000000, 0.000000000000000000 ) ) ;
#18237 = EDGE_LOOP ( 'NONE', ( #2170, #1000, #24434, #25560 ) ) ;
#18238 = DIRECTION ( 'NONE',  ( -1.000000000000000000, -0.000000000000000000, 0.000000000000000000 ) ) ;
#18239 = CARTESIAN_POINT ( 'NONE',  ( 48.45023387855729879, 31.00000000000000355, 83.88660019351674180 ) ) ;
#18240 = CARTESIAN_POINT ( 'NONE',  ( -16.41266422346949128, 31.00000000000000355, -1.216702565357028698 ) ) ;
#18241 = ORIENTED_EDGE ( 'NONE', *, *, #37350, .T. ) ;
#18242 = CARTESIAN_POINT ( 'NONE',  ( 12.72035051019986618, 40.00000000000000000, 25.87482915247129966 ) ) ;
#18243 = EDGE_CURVE ( 'NONE', #30242, #17459, #21680, .T. ) ;
#18244 = VERTEX_POINT ( 'NONE', #11836 ) ;
#18245 = ORIENTED_EDGE ( 'NONE', *, *, #35031, .F. ) ;
#18246 = CARTESIAN_POINT ( 'NONE',  ( 0.000000000000000000, 71.21168426767221149, -86.70160608319253015 ) ) ;
#18247 = DIRECTION ( 'NONE',  ( 0.000000000000000000, 0.3641605752528168094, 0.9313361774523405412 ) ) ;
#18248 = CARTESIAN_POINT ( 'NONE',  ( 0.000000000000000000, 0.000000000000000000, 0.000000000000000000 ) ) ;
#18249 = LINE ( 'NONE', #8168, #22614 ) ;
#18250 = AXIS2_PLACEMENT_3D ( 'NONE', #11267, #4920, #28516 ) ;
#18251 = ORIENTED_EDGE ( 'NONE', *, *, #30810, .T. ) ;
#18252 = DIRECTION ( 'NONE',  ( -1.000000000000000000, -0.000000000000000000, -0.000000000000000000 ) ) ;
#18253 = EDGE_LOOP ( 'NONE', ( #8156, #19477, #22588, #7804 ) ) ;
#18254 = DIRECTION ( 'NONE',  ( -1.000000000000000000, -0.000000000000000000, -0.000000000000000000 ) ) ;
#18255 = VECTOR ( 'NONE', #2050, 1000.000000000000000 ) ;
#18256 = CARTESIAN_POINT ( 'NONE',  ( 17.99999999999999645, 80.02407177072956301, 78.64108602299977235 ) ) ;
#18257 = VECTOR ( 'NONE', #35386, 1000.000000000000000 ) ;
#18258 = LINE ( 'NONE', #31523, #38168 ) ;
#18259 = CIRCLE ( 'NONE', #25895, 31.49899999999999878 ) ;
#18260 = CARTESIAN_POINT ( 'NONE',  ( -26.14979319748359643, -2.055254544495722868, 2.972870684497277427 ) ) ;
#18261 = ORIENTED_EDGE ( 'NONE', *, *, #36153, .F. ) ;
#18262 = ORIENTED_EDGE ( 'NONE', *, *, #42066, .T. ) ;
#18263 = CARTESIAN_POINT ( 'NONE',  ( 0.000000000000000000, -115.6826031496111398, -8.575274253898639287 ) ) ;
#18264 = LINE ( 'NONE', #1615, #22869 ) ;
#18265 = AXIS2_PLACEMENT_3D ( 'NONE', #20955, #4305, #27915 ) ;
#18266 = ORIENTED_EDGE ( 'NONE', *, *, #17119, .T. ) ;
#18268 = ORIENTED_EDGE ( 'NONE', *, *, #39788, .T. ) ;
#18267 = CARTESIAN_POINT ( 'NONE',  ( 17.99999999999999645, 0.000000000000000000, 0.000000000000000000 ) ) ;
#18269 = CARTESIAN_POINT ( 'NONE',  ( 45.06603723660748528, 31.00000000000000355, 15.38899812203272788 ) ) ;
#18270 = FACE_OUTER_BOUND ( 'NONE', #11926, .T. ) ;
#18271 = EDGE_CURVE ( 'NONE', #13702, #41253, #32300, .T. ) ;
#18273 = PRESENTATION_STYLE_ASSIGNMENT (( #15211 ) ) ;
#18272 = CARTESIAN_POINT ( 'NONE',  ( 17.99999999999999645, -115.9387338813861277, -3.769613505537241949 ) ) ;
#18274 = VERTEX_POINT ( 'NONE', #18405 ) ;
#18275 = LINE ( 'NONE', #11705, #6043 ) ;
#18276 = CARTESIAN_POINT ( 'NONE',  ( -47.50570208456527865, 40.00000000000000000, -41.80188021843024870 ) ) ;
#18277 = EDGE_CURVE ( 'NONE', #23787, #11001, #1765, .T. ) ;
#18278 = FACE_OUTER_BOUND ( 'NONE', #35887, .T. ) ;
#18279 = CARTESIAN_POINT ( 'NONE',  ( -10.00000000000000000, 0.000000000000000000, 0.000000000000000000 ) ) ;
#18280 = VERTEX_POINT ( 'NONE', #15970 ) ;
#18281 = CARTESIAN_POINT ( 'NONE',  ( 9.000000000000000000, 6.007673836298521586, -35.49518073029990717 ) ) ;
#18282 = ORIENTED_EDGE ( 'NONE', *, *, #32458, .F. ) ;
#18283 = AXIS2_PLACEMENT_3D ( 'NONE', #30194, #30415, #33244 ) ;
#18284 = DIRECTION ( 'NONE',  ( 0.000000000000000000, 0.000000000000000000, -1.000000000000000000 ) ) ;
#18285 = CARTESIAN_POINT ( 'NONE',  ( 17.99999999999999645, 0.000000000000000000, 0.000000000000000000 ) ) ;
#18286 = AXIS2_PLACEMENT_3D ( 'NONE', #29188, #16095, #16532 ) ;
#18287 = CARTESIAN_POINT ( 'NONE',  ( 64.37268382102905662, 31.00000000000000000, -8.487791176987355968 ) ) ;
#18288 = CARTESIAN_POINT ( 'NONE',  ( 18.00000000000000355, 0.000000000000000000, 0.000000000000000000 ) ) ;
#18289 = ORIENTED_EDGE ( 'NONE', *, *, #39954, .T. ) ;
#18290 = CIRCLE ( 'NONE', #16871, 13.60000000000000320 ) ;
#18291 = CARTESIAN_POINT ( 'NONE',  ( 17.99999999999999645, -112.1427988504407551, -3.502162136924565239 ) ) ;
#18292 = EDGE_CURVE ( 'NONE', #17669, #13070, #10266, .T. ) ;
#18293 = ORIENTED_EDGE ( 'NONE', *, *, #35614, .T. ) ;
#18294 = DIRECTION ( 'NONE',  ( -1.000000000000000000, 0.000000000000000000, -0.000000000000000000 ) ) ;
#18295 = EDGE_CURVE ( 'NONE', #18000, #31449, #15870, .T. ) ;
#18296 = CARTESIAN_POINT ( 'NONE',  ( 0.000000000000000000, -52.19040376560500505, 99.31985817764160629 ) ) ;
#18297 = CARTESIAN_POINT ( 'NONE',  ( -40.08783408682389648, 31.00000000000000355, 81.04563091337925584 ) ) ;
#18298 = CARTESIAN_POINT ( 'NONE',  ( -82.08563009789774867, 40.00000000000000711, 40.34115885382633593 ) ) ;
#18299 = FACE_OUTER_BOUND ( 'NONE', #24657, .T. ) ;
#18300 = ORIENTED_EDGE ( 'NONE', *, *, #39289, .F. ) ;
#18301 = CARTESIAN_POINT ( 'NONE',  ( 0.000000000000000000, 0.000000000000000000, 0.000000000000000000 ) ) ;
#18302 = ORIENTED_EDGE ( 'NONE', *, *, #569, .T. ) ;
#18303 = CARTESIAN_POINT ( 'NONE',  ( 0.000000000000000000, -108.8684555192045025, -27.12806418649726936 ) ) ;
#18304 = DIRECTION ( 'NONE',  ( -1.000000000000000000, 0.000000000000000000, 0.000000000000000000 ) ) ;
#18306 = ORIENTED_EDGE ( 'NONE', *, *, #38986, .T. ) ;
#18305 = LINE ( 'NONE', #27889, #30461 ) ;
#18307 = DIRECTION ( 'NONE',  ( -1.000000000000000000, 0.000000000000000000, -0.000000000000000000 ) ) ;
#18308 = ORIENTED_EDGE ( 'NONE', *, *, #13272, .T. ) ;
#18309 = CARTESIAN_POINT ( 'NONE',  ( 0.000000000000000000, 9.484061862023926537, 30.03730300138984433 ) ) ;
#18310 = CARTESIAN_POINT ( 'NONE',  ( 81.71702119589899382, 39.99999999999999289, -47.19735719316410183 ) ) ;
#18311 = CIRCLE ( 'NONE', #21803, 116.0000000000000000 ) ;
#18312 = DIRECTION ( 'NONE',  ( 0.000000000000000000, -1.000000000000000000, 1.224646799147353207E-16 ) ) ;
#18313 = AXIS2_PLACEMENT_3D ( 'NONE', #26866, #13574, #42991 ) ;
#18314 = CIRCLE ( 'NONE', #3622, 20.00000000000000711 ) ;
#18315 = ORIENTED_EDGE ( 'NONE', *, *, #36779, .T. ) ;
#18316 = CARTESIAN_POINT ( 'NONE',  ( 0.000000000000000000, 13.56094713063571433, 50.20060470671744923 ) ) ;
#18317 = DIRECTION ( 'NONE',  ( 0.000000000000000000, 0.000000000000000000, 1.000000000000000000 ) ) ;
#18318 = VECTOR ( 'NONE', #21433, 1000.000000000000000 ) ;
#18319 = EDGE_CURVE ( 'NONE', #34259, #42455, #38619, .T. ) ;
#18321 = DIRECTION ( 'NONE',  ( -1.000000000000000000, 0.000000000000000000, 0.000000000000000000 ) ) ;
#18320 = DIRECTION ( 'NONE',  ( 0.000000000000000000, 0.000000000000000000, 1.000000000000000000 ) ) ;
#18322 = ORIENTED_EDGE ( 'NONE', *, *, #18111, .F. ) ;
#18323 = CARTESIAN_POINT ( 'NONE',  ( 0.000000000000000000, 36.34385289850631295, -29.77717097092038756 ) ) ;
#18324 = VERTEX_POINT ( 'NONE', #34935 ) ;
#18325 = LINE ( 'NONE', #35488, #40507 ) ;
#18327 = CARTESIAN_POINT ( 'NONE',  ( 23.59836588144746017, 40.00000000000000000, -26.81698947917456621 ) ) ;
#18326 = AXIS2_PLACEMENT_3D ( 'NONE', #29499, #25820, #26232 ) ;
#18328 = DIRECTION ( 'NONE',  ( -1.000000000000000000, -0.000000000000000000, -0.000000000000000000 ) ) ;
#18329 = EDGE_CURVE ( 'NONE', #1575, #33606, #17324, .T. ) ;
#18330 = DIRECTION ( 'NONE',  ( -1.000000000000000000, 0.000000000000000000, 0.000000000000000000 ) ) ;
#18331 = ADVANCED_FACE ( 'NONE', ( #35760 ), #41901, .T. ) ;
#18332 = CARTESIAN_POINT ( 'NONE',  ( 0.000000000000000000, 0.000000000000000000, 0.000000000000000000 ) ) ;
#18333 = VERTEX_POINT ( 'NONE', #31890 ) ;
#18334 = DIRECTION ( 'NONE',  ( 0.000000000000000000, 0.000000000000000000, 1.000000000000000000 ) ) ;
#18335 = VERTEX_POINT ( 'NONE', #9172 ) ;
#18336 = LINE ( 'NONE', #27699, #2928 ) ;
#18337 = CARTESIAN_POINT ( 'NONE',  ( 17.99999999999999645, -116.4607004671426438, -30.94182036827323756 ) ) ;
#18338 = CARTESIAN_POINT ( 'NONE',  ( -13.53264355869793967, 31.00000000000000355, -39.83251807627727459 ) ) ;
#18339 = VERTEX_POINT ( 'NONE', #18838 ) ;
#18340 = DIRECTION ( 'NONE',  ( 0.000000000000000000, 0.5528000653611888637, 0.8333139190825180620 ) ) ;
#18341 = CARTESIAN_POINT ( 'NONE',  ( 9.000000000000000000, -34.45183346761128718, -10.44371441202691742 ) ) ;
#18342 = CARTESIAN_POINT ( 'NONE',  ( 46.64447153568531945, 31.00000000000000355, 60.78881617101084345 ) ) ;
#18343 = VECTOR ( 'NONE', #42908, 1000.000000000000000 ) ;
#18344 = EDGE_CURVE ( 'NONE', #10739, #15532, #9613, .T. ) ;
#18345 = EDGE_CURVE ( 'NONE', #5490, #34783, #15238, .T. ) ;
#18346 = ORIENTED_EDGE ( 'NONE', *, *, #28512, .F. ) ;
#18347 = CARTESIAN_POINT ( 'NONE',  ( 38.48770111205617894, 31.00000000000000355, 44.02435964457617956 ) ) ;
#18348 = ADVANCED_FACE ( 'NONE', ( #2381 ), #22104, .F. ) ;
#18349 = ADVANCED_FACE ( 'NONE', ( #16621 ), #22734, .F. ) ;
#18350 = AXIS2_PLACEMENT_3D ( 'NONE', #41372, #11521, #18109 ) ;
#18351 = CARTESIAN_POINT ( 'NONE',  ( -81.55297449308174862, 40.00000000000000711, -40.20044092665353475 ) ) ;
#18352 = ORIENTED_EDGE ( 'NONE', *, *, #19339, .T. ) ;
#18353 = VECTOR ( 'NONE', #42721, 1000.000000000000000 ) ;
#18354 = CARTESIAN_POINT ( 'NONE',  ( -10.00000000000000000, 0.000000000000000000, 0.000000000000000000 ) ) ;
#18355 = CARTESIAN_POINT ( 'NONE',  ( 18.00000000000000355, -32.32520163883607722, 34.09746168776025854 ) ) ;
#18356 = CARTESIAN_POINT ( 'NONE',  ( -25.39999999999999147, 1.836970198721029589E-15, -15.00000000000000000 ) ) ;
#18358 = ORIENTED_EDGE ( 'NONE', *, *, #29118, .F. ) ;
#18357 = CARTESIAN_POINT ( 'NONE',  ( 17.99999999999999645, 0.000000000000000000, 0.000000000000000000 ) ) ;
#18359 = FACE_OUTER_BOUND ( 'NONE', #38312, .T. ) ;
#18360 = DIRECTION ( 'NONE',  ( -1.000000000000000000, 1.373900992973642066E-15, 3.979293995072266947E-16 ) ) ;
#18361 = PRODUCT_DEFINITION_SHAPE ( 'NONE', 'NONE',  #43213 ) ;
#18362 = VERTEX_POINT ( 'NONE', #40111 ) ;
#18363 = CARTESIAN_POINT ( 'NONE',  ( -37.49462465745612860, 40.00000000000000000, -48.86220178749748300 ) ) ;
#18364 = LINE ( 'NONE', #35321, #6146 ) ;
#18365 = ORIENTED_EDGE ( 'NONE', *, *, #25735, .T. ) ;
#18366 = DIRECTION ( 'NONE',  ( 0.000000000000000000, 0.000000000000000000, -1.000000000000000000 ) ) ;
#18367 = CARTESIAN_POINT ( 'NONE',  ( 0.000000000000000000, 46.87740477351718482, 16.82754413119463166 ) ) ;
#18368 = LINE ( 'NONE', #15085, #28427 ) ;
#18369 = EDGE_LOOP ( 'NONE', ( #7461, #10992 ) ) ;
#18370 = EDGE_CURVE ( 'NONE', #30536, #14276, #38845, .T. ) ;
#18371 = VECTOR ( 'NONE', #29406, 1000.000000000000000 ) ;
#18372 = ORIENTED_EDGE ( 'NONE', *, *, #41538, .T. ) ;
#18373 = DIRECTION ( 'NONE',  ( 3.009274222672345096E-17, 1.000000000000000000, -2.455023325076454960E-18 ) ) ;
#18374 = VERTEX_POINT ( 'NONE', #12890 ) ;
#18375 = CARTESIAN_POINT ( 'NONE',  ( 9.000000000000001776, -42.87700105098682002, 107.7847984684003393 ) ) ;
#18376 = CARTESIAN_POINT ( 'NONE',  ( 0.000000000000000000, 17.50309955389674954, -43.60271849949345579 ) ) ;
#18377 = EDGE_CURVE ( 'NONE', #11054, #15772, #26417, .T. ) ;
#18378 = CYLINDRICAL_SURFACE ( 'NONE', #27476, 20.00000000000000355 ) ;
#18379 = CARTESIAN_POINT ( 'NONE',  ( 17.99999999999999645, 101.1249659627849269, 48.60055280209592610 ) ) ;
#18380 = VERTEX_POINT ( 'NONE', #6524 ) ;
#18382 = DIRECTION ( 'NONE',  ( -0.000000000000000000, -0.000000000000000000, 1.000000000000000000 ) ) ;
#18381 = MECHANICAL_DESIGN_GEOMETRIC_PRESENTATION_REPRESENTATION (  '', ( #30978 ), #26063 ) ;
#18383 = CIRCLE ( 'NONE', #866, 59.00000000000000000 ) ;
#18384 = CARTESIAN_POINT ( 'NONE',  ( 0.000000000000000000, 5.492704054968225336, -115.8698847939555776 ) ) ;
#18385 = VERTEX_POINT ( 'NONE', #3014 ) ;
#18386 = DIRECTION ( 'NONE',  ( -1.000000000000000000, 0.000000000000000000, -0.000000000000000000 ) ) ;
#18387 = DIRECTION ( 'NONE',  ( 0.000000000000000000, 0.000000000000000000, 1.000000000000000000 ) ) ;
#18388 = DIRECTION ( 'NONE',  ( -2.137915722948479303E-31, 1.000000000000000000, -6.123233995736766036E-17 ) ) ;
#18389 = LINE ( 'NONE', #41886, #237 ) ;
#18390 = CARTESIAN_POINT ( 'NONE',  ( -15.46676570949300000, 31.00000000000000355, 45.57083133015776610 ) ) ;
#18391 = ORIENTED_EDGE ( 'NONE', *, *, #12108, .T. ) ;
#18393 = CARTESIAN_POINT ( 'NONE',  ( 0.000000000000000000, 34.74871106919619024, 106.6808302961373158 ) ) ;
#18392 = LINE ( 'NONE', #11169, #30950 ) ;
#18394 = EDGE_CURVE ( 'NONE', #967, #34610, #23166, .T. ) ;
#18395 = EDGE_CURVE ( 'NONE', #32974, #36878, #37450, .T. ) ;
#18396 = ORIENTED_EDGE ( 'NONE', *, *, #29202, .T. ) ;
#18397 = ADVANCED_FACE ( 'NONE', ( #42734 ), #39896, .T. ) ;
#18398 = EDGE_CURVE ( 'NONE', #11164, #7056, #34001, .T. ) ;
#18399 = AXIS2_PLACEMENT_3D ( 'NONE', #11826, #8311, #34707 ) ;
#18400 = CARTESIAN_POINT ( 'NONE',  ( -15.01009539198478748, 40.00000000000000000, 56.06562763604418365 ) ) ;
#18401 = CARTESIAN_POINT ( 'NONE',  ( -7.911223860816524400, 40.00000000000000000, 59.30865348673674475 ) ) ;
#18402 = EDGE_CURVE ( 'NONE', #14428, #30604, #26837, .T. ) ;
#18403 = AXIS2_PLACEMENT_3D ( 'NONE', #26991, #36346, #39828 ) ;
#18404 = DIRECTION ( 'NONE',  ( 0.000000000000000000, 0.2631025642275217069, -0.9647678688145158166 ) ) ;
#18405 = CARTESIAN_POINT ( 'NONE',  ( 0.000000000000000000, -57.69704296431110890, -105.7900857083235451 ) ) ;
#18406 = EDGE_CURVE ( 'NONE', #2151, #21317, #39554, .T. ) ;
#18407 = CARTESIAN_POINT ( 'NONE',  ( 17.99999999999999645, 30.71634675606066267, -8.790889055186230649 ) ) ;
#18408 = DIRECTION ( 'NONE',  ( 1.000000000000000000, 0.000000000000000000, 0.000000000000000000 ) ) ;
#18409 = ORIENTED_EDGE ( 'NONE', *, *, #36695, .T. ) ;
#18410 = CARTESIAN_POINT ( 'NONE',  ( -23.46968090759046888, 40.00000000000000000, -20.57717900685300449 ) ) ;
#18411 = VERTEX_POINT ( 'NONE', #3243 ) ;
#18412 = DIRECTION ( 'NONE',  ( -1.000000000000000000, 0.000000000000000000, -0.000000000000000000 ) ) ;
#18413 = AXIS2_PLACEMENT_3D ( 'NONE', #39190, #35920, #29409 ) ;
#18414 = DIRECTION ( 'NONE',  ( 1.000000000000000000, 0.000000000000000000, 0.000000000000000000 ) ) ;
#18415 = ORIENTED_EDGE ( 'NONE', *, *, #15332, .F. ) ;
#18416 = CARTESIAN_POINT ( 'NONE',  ( 0.000000000000000000, -78.75547124681308730, -91.20343606297076633 ) ) ;
#18417 = CYLINDRICAL_SURFACE ( 'NONE', #28993, 4.500000000000002665 ) ;
#18418 = ORIENTED_EDGE ( 'NONE', *, *, #34346, .F. ) ;
#18419 = CARTESIAN_POINT ( 'NONE',  ( 4.211140560182196957, -2.431303136016555122, -3.745885042887436622 ) ) ;
#18420 = ORIENTED_EDGE ( 'NONE', *, *, #19171, .T. ) ;
#18421 = VERTEX_POINT ( 'NONE', #26198 ) ;
#18422 = CARTESIAN_POINT ( 'NONE',  ( 0.2500000000000002220, 0.000000000000000000, 0.000000000000000000 ) ) ;
#18423 = CARTESIAN_POINT ( 'NONE',  ( 39.23423008409712054, 31.00000000000000355, 79.83814995801117220 ) ) ;
#18424 = AXIS2_PLACEMENT_3D ( 'NONE', #21292, #11225, #24558 ) ;
#18425 = ORIENTED_EDGE ( 'NONE', *, *, #34945, .F. ) ;
#18426 = CARTESIAN_POINT ( 'NONE',  ( 18.00000000000000355, 0.000000000000000000, 0.000000000000000000 ) ) ;
#18427 = AXIS2_PLACEMENT_3D ( 'NONE', #26298, #3114, #13809 ) ;
#18428 = EDGE_CURVE ( 'NONE', #12487, #2427, #9608, .T. ) ;
#18429 = CARTESIAN_POINT ( 'NONE',  ( -8.749793197483594298, -2.055254544495723756, 2.972870684497274762 ) ) ;
#18430 = ORIENTED_EDGE ( 'NONE', *, *, #22811, .T. ) ;
#18431 = DIRECTION ( 'NONE',  ( 0.000000000000000000, 0.000000000000000000, 1.000000000000000000 ) ) ;
#18432 = AXIS2_PLACEMENT_3D ( 'NONE', #18840, #23167, #6327 ) ;
#18433 = CARTESIAN_POINT ( 'NONE',  ( 18.00000000000000355, 0.000000000000000000, 0.000000000000000000 ) ) ;
#18434 = CARTESIAN_POINT ( 'NONE',  ( 27.02985023942251175, 31.00000000000000355, 3.586895573513789071 ) ) ;
#18436 = FACE_OUTER_BOUND ( 'NONE', #19927, .T. ) ;
#18435 = DIRECTION ( 'NONE',  ( 1.000000000000000000, 0.000000000000000000, -0.000000000000000000 ) ) ;
#18437 = LINE ( 'NONE', #41283, #16452 ) ;
#18438 = CARTESIAN_POINT ( 'NONE',  ( -6.004904395537136175, 19.19999999999999574, 0.000000000000000000 ) ) ;
#18439 = ORIENTED_EDGE ( 'NONE', *, *, #6718, .F. ) ;
#18440 =( LENGTH_UNIT ( ) NAMED_UNIT ( * ) SI_UNIT ( .MILLI., .METRE. ) );
#18441 = ORIENTED_EDGE ( 'NONE', *, *, #2420, .F. ) ;
#18442 = CARTESIAN_POINT ( 'NONE',  ( 9.000000000000001776, -47.31079789947416003, -105.9135893174955783 ) ) ;
#18443 = CARTESIAN_POINT ( 'NONE',  ( 91.55691129138550366, 31.00000000000000000, -24.53049628908797430 ) ) ;
#18444 = DIRECTION ( 'NONE',  ( 0.000000000000000000, -0.9213119778704166318, 0.3888241754733122724 ) ) ;
#18445 = ORIENTED_EDGE ( 'NONE', *, *, #19895, .F. ) ;
#18446 = EDGE_CURVE ( 'NONE', #1856, #10231, #10022, .T. ) ;
#18447 = ADVANCED_FACE ( 'NONE', ( #3462 ), #36201, .F. ) ;
#18448 = CIRCLE ( 'NONE', #3031, 13.59999999999999964 ) ;
#18449 = CARTESIAN_POINT ( 'NONE',  ( 27.02985023942251885, 40.00000000000000000, 3.586895573513070090 ) ) ;
#18450 = EDGE_CURVE ( 'NONE', #17523, #29749, #20782, .T. ) ;
#18451 = ORIENTED_EDGE ( 'NONE', *, *, #36206, .T. ) ;
#18452 = VECTOR ( 'NONE', #39360, 1000.000000000000000 ) ;
#18453 = ORIENTED_EDGE ( 'NONE', *, *, #87, .F. ) ;
#18454 = CYLINDRICAL_SURFACE ( 'NONE', #24874, 59.00000000000000711 ) ;
#18455 = CYLINDRICAL_SURFACE ( 'NONE', #26972, 59.00000000000000000 ) ;
#18456 = DIRECTION ( 'NONE',  ( 0.000000000000000000, 0.000000000000000000, 1.000000000000000000 ) ) ;
#18457 = AXIS2_PLACEMENT_3D ( 'NONE', #12466, #7167, #167 ) ;
#18458 = FACE_BOUND ( 'NONE', #32525, .T. ) ;
#18459 = ADVANCED_FACE ( 'NONE', ( #10248 ), #23594, .F. ) ;
#18460 = FACE_OUTER_BOUND ( 'NONE', #17504, .T. ) ;
#18461 = VERTEX_POINT ( 'NONE', #30329 ) ;
#18462 = CARTESIAN_POINT ( 'NONE',  ( 0.000000000000000000, 0.000000000000000000, -25.00000000000000000 ) ) ;
#18463 = ORIENTED_EDGE ( 'NONE', *, *, #4641, .F. ) ;
#18464 = CARTESIAN_POINT ( 'NONE',  ( 0.000000000000000000, 119.0898412705474385, 18.38751498043774646 ) ) ;
#18465 = CARTESIAN_POINT ( 'NONE',  ( 0.000000000000000000, 0.000000000000000000, 0.000000000000000000 ) ) ;
#18466 = EDGE_CURVE ( 'NONE', #26511, #18955, #25988, .T. ) ;
#18467 = DIRECTION ( 'NONE',  ( 1.000000000000000000, 0.000000000000000000, 0.000000000000000000 ) ) ;
#18468 = CARTESIAN_POINT ( 'NONE',  ( 17.99999999999999645, 32.49609705003727100, -15.49205204337240005 ) ) ;
#18469 = ORIENTED_EDGE ( 'NONE', *, *, #27559, .F. ) ;
#18470 = ORIENTED_EDGE ( 'NONE', *, *, #13190, .T. ) ;
#18471 = CARTESIAN_POINT ( 'NONE',  ( -106.4195705685741871, -106.4195705685773135, 9.999999999999753086 ) ) ;
#18472 = AXIS2_PLACEMENT_3D ( 'NONE', #16209, #26237, #39509 ) ;
#18473 = DIRECTION ( 'NONE',  ( 1.000000000000000000, 0.000000000000000000, 0.000000000000000000 ) ) ;
#18474 =( GEOMETRIC_REPRESENTATION_CONTEXT ( 3 ) GLOBAL_UNCERTAINTY_ASSIGNED_CONTEXT ( ( #13897 ) ) GLOBAL_UNIT_ASSIGNED_CONTEXT ( ( #159, #11062, #10227 ) ) REPRESENTATION_CONTEXT ( 'NONE', 'WORKASPACE' ) );
#18475 = ORIENTED_EDGE ( 'NONE', *, *, #19288, .T. ) ;
#18477 = ORIENTED_EDGE ( 'NONE', *, *, #10315, .F. ) ;
#18476 = DIRECTION ( 'NONE',  ( 0.000000000000000000, 0.2113826236296182937, 0.9774033898178680069 ) ) ;
#18478 = CARTESIAN_POINT ( 'NONE',  ( -34.17541447290002310, 31.00000000000000355, -26.31327426976606176 ) ) ;
#18479 = ORIENTED_EDGE ( 'NONE', *, *, #4397, .T. ) ;
#18480 = CYLINDRICAL_SURFACE ( 'NONE', #2116, 100.0000000000000000 ) ;
#18481 = AXIS2_PLACEMENT_3D ( 'NONE', #31810, #28968, #42239 ) ;
#18483 = CARTESIAN_POINT ( 'NONE',  ( 0.000000000000000000, 89.07460286905850921, 81.15544420874989839 ) ) ;
#18482 = CARTESIAN_POINT ( 'NONE',  ( -4.000000000000000000, 0.000000000000000000, 0.000000000000000000 ) ) ;
#18484 = EDGE_LOOP ( 'NONE', ( #40349, #29537, #38426, #37897 ) ) ;
#18485 = CARTESIAN_POINT ( 'NONE',  ( 2.500000000000000000, 0.000000000000000000, 0.000000000000000000 ) ) ;
#18486 = CARTESIAN_POINT ( 'NONE',  ( -60.39136959355892031, 40.00000000000000711, -16.27924862580663046 ) ) ;
#18487 = DIRECTION ( 'NONE',  ( -1.000000000000000000, -0.000000000000000000, -0.000000000000000000 ) ) ;
#18488 = AXIS2_PLACEMENT_3D ( 'NONE', #28992, #35924, #5832 ) ;
#18489 = CARTESIAN_POINT ( 'NONE',  ( 18.00000000000000355, -46.90537658765333617, 2.727856614654147638 ) ) ;
#18490 = ORIENTED_EDGE ( 'NONE', *, *, #6426, .T. ) ;
#18491 = DIRECTION ( 'NONE',  ( 1.000000000000000000, 0.000000000000000000, 0.000000000000000000 ) ) ;
#18492 = VERTEX_POINT ( 'NONE', #35988 ) ;
#18493 = CIRCLE ( 'NONE', #15666, 59.00000000000001421 ) ;
#18494 = DIRECTION ( 'NONE',  ( -1.000000000000000000, -0.000000000000000000, -0.000000000000000000 ) ) ;
#18495 = CARTESIAN_POINT ( 'NONE',  ( 9.000000000000001776, -115.9750404417043939, -2.406240749598616446 ) ) ;
#18496 = CARTESIAN_POINT ( 'NONE',  ( 9.510694223897102617, 31.00000000000000355, -72.24097909213479340 ) ) ;
#18497 = LINE ( 'NONE', #2696, #14939 ) ;
#18498 = ORIENTED_EDGE ( 'NONE', *, *, #18569, .F. ) ;
#18499 = ADVANCED_FACE ( 'NONE', ( #6111 ), #1283, .F. ) ;
#18500 = EDGE_CURVE ( 'NONE', #24559, #39731, #34232, .T. ) ;
#18501 = CIRCLE ( 'NONE', #42810, 19.19999999999999574 ) ;
#18502 = DIRECTION ( 'NONE',  ( 1.000000000000000000, 0.000000000000000000, -0.000000000000000000 ) ) ;
#18503 = EDGE_LOOP ( 'NONE', ( #41517, #4899, #23439, #11811 ) ) ;
#18504 = LINE ( 'NONE', #18937, #17326 ) ;
#18505 = LINE ( 'NONE', #1434, #15104 ) ;
#18506 = CARTESIAN_POINT ( 'NONE',  ( 87.09251733236551729, 31.00000000000000000, 5.815661930448015937 ) ) ;
#18507 = CARTESIAN_POINT ( 'NONE',  ( -5.980347265640406640, 40.00000000000000000, 89.59238221261722401 ) ) ;
#18508 = AXIS2_PLACEMENT_3D ( 'NONE', #4576, #11367, #24697 ) ;
#18509 =( BOUNDED_SURFACE ( )  B_SPLINE_SURFACE ( 3, 2, ( 
 ( #40218, #7273, #13213 ),
 ( #27371, #271, #3553 ),
 ( #33678, #39988, #10120 ),
 ( #13643, #23471, #37163 ),
 ( #10783, #7501, #36735 ),
 ( #512, #34119, #10565 ) ),
 .UNSPECIFIED., .F., .F., .F. ) 
 B_SPLINE_SURFACE_WITH_KNOTS ( ( 4, 2, 4 ),
 ( 3, 3 ),
 ( 0.02032853247518126225, 0.02278863295364821212, 0.02524873343211516200 ),
 ( 0.000000000000000000, 1.000000000000000000 ),
 .UNSPECIFIED. ) 
 GEOMETRIC_REPRESENTATION_ITEM ( )  RATIONAL_B_SPLINE_SURFACE ( (
 ( 1.000000000000000000, 0.8047781615896835161, 1.000000000000000000),
 ( 1.000000000000000000, 0.8123767586291043008, 1.000000000000000000),
 ( 1.000000000000000000, 0.8190662415562011134, 1.000000000000000000),
 ( 1.000000000000000000, 0.8192361015671398849, 1.000000000000000000),
 ( 1.000000000000000000, 0.8126135807102121689, 1.000000000000000000),
 ( 1.000000000000000000, 0.8047712338318585568, 1.000000000000000000) ) ) 
 REPRESENTATION_ITEM ( '' )  SURFACE ( )  );
#18510 = DIRECTION ( 'NONE',  ( 0.000000000000000000, 1.246648735278247733E-14, -1.000000000000000000 ) ) ;
#18511 = AXIS2_PLACEMENT_3D ( 'NONE', #32542, #41721, #25609 ) ;
#18512 = EDGE_CURVE ( 'NONE', #566, #27409, #22184, .T. ) ;
#18513 = ORIENTED_EDGE ( 'NONE', *, *, #43083, .F. ) ;
#18514 = DIRECTION ( 'NONE',  ( -1.000000000000000000, -0.000000000000000000, -0.000000000000000000 ) ) ;
#18515 = ORIENTED_EDGE ( 'NONE', *, *, #4189, .T. ) ;
#18516 = DIRECTION ( 'NONE',  ( 0.000000000000000000, -0.1837495178165570453, -0.9829730996839042279 ) ) ;
#18517 = AXIS2_PLACEMENT_3D ( 'NONE', #18999, #25120, #15700 ) ;
#18518 = EDGE_CURVE ( 'NONE', #33403, #11059, #6115, .T. ) ;
#18520 = VECTOR ( 'NONE', #10058, 1000.000000000000000 ) ;
#18519 = CYLINDRICAL_SURFACE ( 'NONE', #28982, 36.00000000000000000 ) ;
#18521 = STYLED_ITEM ( 'NONE', ( #19556 ), #27661 ) ;
#18523 = ORIENTED_EDGE ( 'NONE', *, *, #38552, .F. ) ;
#18522 = LINE ( 'NONE', #35258, #12344 ) ;
#18524 = DIRECTION ( 'NONE',  ( 1.000000000000000000, 0.000000000000000000, 0.000000000000000000 ) ) ;
#18525 = ORIENTED_EDGE ( 'NONE', *, *, #40574, .T. ) ;
#18526 = DIRECTION ( 'NONE',  ( 0.000000000000000000, 0.9574220383620062336, -0.2886919473396183933 ) ) ;
#18527 = CIRCLE ( 'NONE', #36541, 120.5010000000000190 ) ;
#18528 = CARTESIAN_POINT ( 'NONE',  ( 17.99999999999999645, -47.31079789947556691, 105.9135893174949530 ) ) ;
#18529 = VERTEX_POINT ( 'NONE', #37074 ) ;
#18530 = CARTESIAN_POINT ( 'NONE',  ( -31.74999999999995737, 0.000000000000000000, 0.000000000000000000 ) ) ;
#18531 = CARTESIAN_POINT ( 'NONE',  ( 17.99999999999999645, 110.0562500189198829, 49.07252625220148445 ) ) ;
#18533 = CARTESIAN_POINT ( 'NONE',  ( -8.749793197483594298, -12.05525454449572464, 2.972870684497274762 ) ) ;
#18532 = CARTESIAN_POINT ( 'NONE',  ( 0.000000000000000000, 0.000000000000000000, 0.000000000000000000 ) ) ;
#18534 = ORIENTED_EDGE ( 'NONE', *, *, #1960, .F. ) ;
#18535 = CARTESIAN_POINT ( 'NONE',  ( -105.9879088449591933, 40.00000000000000000, -0.3807199291576673361 ) ) ;
#18537 = EDGE_LOOP ( 'NONE', ( #25170, #29917, #23012 ) ) ;
#18536 = EDGE_CURVE ( 'NONE', #15632, #10000, #30533, .T. ) ;
#18538 = CARTESIAN_POINT ( 'NONE',  ( 17.99999999999999645, 111.2559044912524939, 32.83479428644713494 ) ) ;
#18539 = CARTESIAN_POINT ( 'NONE',  ( 36.95980244579788376, 40.00000000000000000, 4.931273285801174744 ) ) ;
#18540 = CARTESIAN_POINT ( 'NONE',  ( 0.000000000000000000, 110.0562500189198829, 49.07252625220149156 ) ) ;
#18541 = EDGE_CURVE ( 'NONE', #28005, #21531, #10681, .T. ) ;
#18542 = AXIS2_PLACEMENT_3D ( 'NONE', #3108, #32608, #32813 ) ;
#18543 = LINE ( 'NONE', #8023, #4711 ) ;
#18544 = DIRECTION ( 'NONE',  ( -1.000000000000000000, -0.000000000000000000, 0.000000000000000000 ) ) ;
#18546 = VERTEX_POINT ( 'NONE', #40335 ) ;
#18545 = CIRCLE ( 'NONE', #11566, 59.00000000000000000 ) ;
#18547 = CARTESIAN_POINT ( 'NONE',  ( 1.257172072275274388, -3.892973519170983110, -3.433252694550781303 ) ) ;
#18548 = CIRCLE ( 'NONE', #17126, 139.4999999999992610 ) ;
#18549 = VERTEX_POINT ( 'NONE', #17480 ) ;
#18550 = AXIS2_PLACEMENT_3D ( 'NONE', #11951, #24849, #5380 ) ;
#18551 = DIRECTION ( 'NONE',  ( 1.000000000000000000, 0.000000000000000000, 0.000000000000000000 ) ) ;
#18552 = DIRECTION ( 'NONE',  ( 0.000000000000000000, 0.000000000000000000, 1.000000000000000000 ) ) ;
#18553 = VECTOR ( 'NONE', #38551, 1000.000000000000000 ) ;
#18554 = CARTESIAN_POINT ( 'NONE',  ( -35.29531037056285214, 31.00000000000000355, 17.40921588598563119 ) ) ;
#18555 = ORIENTED_EDGE ( 'NONE', *, *, #36669, .T. ) ;
#18556 = DIRECTION ( 'NONE',  ( -1.000000000000000000, -0.000000000000000000, -0.000000000000000000 ) ) ;
#18557 = CONTEXT_DEPENDENT_SHAPE_REPRESENTATION ( #30928, #38869 ) ;
#18558 = EDGE_CURVE ( 'NONE', #12961, #28114, #21511, .T. ) ;
#18560 = CIRCLE ( 'NONE', #25487, 13.60000000000000320 ) ;
#18559 = LINE ( 'NONE', #41400, #13570 ) ;
#18561 = CARTESIAN_POINT ( 'NONE',  ( -49.69442049507403425, 31.00000000000000355, -64.76435429890716478 ) ) ;
#18562 = VERTEX_POINT ( 'NONE', #37281 ) ;
#18563 = CARTESIAN_POINT ( 'NONE',  ( -7.015336270751801884, 31.00000000000000355, -53.95087245963820521 ) ) ;
#18564 = CARTESIAN_POINT ( 'NONE',  ( -77.37786320076959612, 40.00000000000000711, 44.69160382239309115 ) ) ;
#18565 = EDGE_CURVE ( 'NONE', #33336, #42002, #11735, .T. ) ;
#18566 = ORIENTED_EDGE ( 'NONE', *, *, #5423, .T. ) ;
#18567 = CARTESIAN_POINT ( 'NONE',  ( -4.235886605889389145, -2.417314728048544303, -3.751161874094020909 ) ) ;
#18568 = DIRECTION ( 'NONE',  ( -1.000000000000000000, 0.000000000000000000, 0.000000000000000000 ) ) ;
#18569 = EDGE_CURVE ( 'NONE', #4344, #38954, #17695, .T. ) ;
#18570 = CARTESIAN_POINT ( 'NONE',  ( 17.99999999999999645, 110.8621702203448649, 34.14058016547577523 ) ) ;
#18571 = AXIS2_PLACEMENT_3D ( 'NONE', #31926, #11653, #8563 ) ;
#18573 = ORIENTED_EDGE ( 'NONE', *, *, #38625, .T. ) ;
#18572 = CYLINDRICAL_SURFACE ( 'NONE', #7666, 10.49999999999999467 ) ;
#18574 = EDGE_CURVE ( 'NONE', #41141, #29185, #14187, .T. ) ;
#18575 = AXIS2_PLACEMENT_3D ( 'NONE', #24639, #11965, #24868 ) ;
#18576 = LINE ( 'NONE', #40990, #943 ) ;
#18577 = VECTOR ( 'NONE', #23783, 1000.000000000000000 ) ;
#18578 = DIRECTION ( 'NONE',  ( 0.000000000000000000, -0.6783118362696222148, 0.7347741508630615259 ) ) ;
#18579 = VECTOR ( 'NONE', #13703, 1000.000000000000000 ) ;
#18580 = VERTEX_POINT ( 'NONE', #40758 ) ;
#18581 = CARTESIAN_POINT ( 'NONE',  ( 59.08215048199704711, 39.99999999999999289, 29.12166076727282515 ) ) ;
#18582 = DIRECTION ( 'NONE',  ( -0.000000000000000000, -0.000000000000000000, 1.000000000000000000 ) ) ;
#18583 = AXIS2_PLACEMENT_3D ( 'NONE', #24564, #3767, #17147 ) ;
#18584 = ORIENTED_EDGE ( 'NONE', *, *, #2944, .F. ) ;
#18585 = AXIS2_PLACEMENT_3D ( 'NONE', #1638, #12136, #5134 ) ;
#18586 = DIRECTION ( 'NONE',  ( 1.000000000000000000, 0.000000000000000000, -0.000000000000000000 ) ) ;
#18587 = DIRECTION ( 'NONE',  ( 1.000000000000000000, 0.000000000000000000, 0.000000000000000000 ) ) ;
#18588 = AXIS2_PLACEMENT_3D ( 'NONE', #12310, #25638, #29107 ) ;
#18589 = CIRCLE ( 'NONE', #22769, 20.00000000000000711 ) ;
#18590 = LINE ( 'NONE', #11579, #29820 ) ;
#18591 = ORIENTED_EDGE ( 'NONE', *, *, #22872, .F. ) ;
#18592 = AXIS2_PLACEMENT_3D ( 'NONE', #20285, #10870, #10646 ) ;
#18593 = ORIENTED_EDGE ( 'NONE', *, *, #29903, .F. ) ;
#18594 = DIRECTION ( 'NONE',  ( -1.000000000000000000, 0.000000000000000000, -0.000000000000000000 ) ) ;
#18595 = EDGE_LOOP ( 'NONE', ( #11156, #39786, #39658, #16345 ) ) ;
#18596 = CYLINDRICAL_SURFACE ( 'NONE', #19572, 120.5010000000000190 ) ;
#18597 = CARTESIAN_POINT ( 'NONE',  ( 17.99999999999999645, -101.1403355683142422, -56.80345518653591341 ) ) ;
#18598 = EDGE_CURVE ( 'NONE', #37525, #40004, #14502, .T. ) ;
#18599 = EDGE_CURVE ( 'NONE', #30629, #22504, #27045, .T. ) ;
#18600 = CARTESIAN_POINT ( 'NONE',  ( 9.000000000000001776, -49.25004636492375454, -16.68630974939812006 ) ) ;
#18601 = FACE_OUTER_BOUND ( 'NONE', #4848, .T. ) ;
#18602 = ORIENTED_EDGE ( 'NONE', *, *, #10200, .T. ) ;
#18603 = DIRECTION ( 'NONE',  ( 3.996523416598930318E-16, -2.658563593772947863E-15, -1.000000000000000000 ) ) ;
#18604 = UNCERTAINTY_MEASURE_WITH_UNIT (LENGTH_MEASURE( 1.000000000000000082E-05 ), #12510, 'distance_accuracy_value', 'NONE');
#18605 = CARTESIAN_POINT ( 'NONE',  ( 9.999999999999998224, 1.543054966925665076E-15, 12.59999999999999964 ) ) ;
#18607 = VERTEX_POINT ( 'NONE', #30967 ) ;
#18606 = VECTOR ( 'NONE', #18869, 1000.000000000000000 ) ;
#18608 = CARTESIAN_POINT ( 'NONE',  ( 0.000000000000000000, 13.22719389141978930, 28.58720592780601066 ) ) ;
#18609 = AXIS2_PLACEMENT_3D ( 'NONE', #16203, #37487, #20304 ) ;
#18610 = CARTESIAN_POINT ( 'NONE',  ( 0.000000000000000000, 0.000000000000000000, 0.000000000000000000 ) ) ;
#18611 = AXIS2_PLACEMENT_3D ( 'NONE', #39823, #2945, #32660 ) ;
#18612 = CIRCLE ( 'NONE', #12315, 120.5010000000000332 ) ;
#18613 = PRODUCT_CONTEXT ( 'NONE', #14185, 'mechanical' ) ;
#18614 = EDGE_CURVE ( 'NONE', #33396, #20507, #6801, .T. ) ;
#18615 = DIRECTION ( 'NONE',  ( 0.000000000000000000, 0.000000000000000000, 1.000000000000000000 ) ) ;
#18616 = CARTESIAN_POINT ( 'NONE',  ( 30.63689417572177831, 31.00000000000000355, 34.91779699477408627 ) ) ;
#18617 = ORIENTED_EDGE ( 'NONE', *, *, #19068, .F. ) ;
#18618 = CIRCLE ( 'NONE', #3922, 59.00000000000000000 ) ;
#18620 = CYLINDRICAL_SURFACE ( 'NONE', #3915, 20.00000000000000355 ) ;
#18619 = DIRECTION ( 'NONE',  ( -1.000000000000000000, 1.577021341797097807E-16, 0.000000000000000000 ) ) ;
#18621 = CIRCLE ( 'NONE', #5329, 20.00000000000000000 ) ;
#18622 = ORIENTED_EDGE ( 'NONE', *, *, #42234, .T. ) ;
#18623 = MECHANICAL_DESIGN_GEOMETRIC_PRESENTATION_REPRESENTATION (  '', ( #40113 ), #9497 ) ;
#18624 = CARTESIAN_POINT ( 'NONE',  ( 8.201713468707295007, 40.00000000000000000, -62.30543997111072940 ) ) ;
#18625 = CIRCLE ( 'NONE', #17902, 116.0000000000000000 ) ;
#18626 = EDGE_CURVE ( 'NONE', #22539, #13634, #12414, .T. ) ;
#18627 = DIRECTION ( 'NONE',  ( -1.000000000000000000, 0.000000000000000000, 0.000000000000000000 ) ) ;
#18628 = CYLINDRICAL_SURFACE ( 'NONE', #8873, 4.500000000000002665 ) ;
#18629 = EDGE_CURVE ( 'NONE', #8703, #2020, #7400, .T. ) ;
#18630 = AXIS2_PLACEMENT_3D ( 'NONE', #16489, #29795, #33468 ) ;
#18631 = DIRECTION ( 'NONE',  ( 0.000000000000000000, -0.6736956436465481035, -0.7390089172206674162 ) ) ;
#18632 = CARTESIAN_POINT ( 'NONE',  ( -13.09503298281258132, 31.00000000000000355, -17.05789676611946959 ) ) ;
#18633 = ORIENTED_EDGE ( 'NONE', *, *, #32241, .F. ) ;
#18634 = CARTESIAN_POINT ( 'NONE',  ( 4.888094100070568437, 40.00000000000000000, 37.04995123692341252 ) ) ;
#18635 = ORIENTED_EDGE ( 'NONE', *, *, #657, .F. ) ;
#18636 = FACE_OUTER_BOUND ( 'NONE', #3119, .T. ) ;
#18637 = PLANE ( 'NONE',  #25639 ) ;
#18638 = ORIENTED_EDGE ( 'NONE', *, *, #22846, .T. ) ;
#18639 = EDGE_CURVE ( 'NONE', #14830, #19624, #10300, .T. ) ;
#18640 = AXIS2_PLACEMENT_3D ( 'NONE', #15645, #36317, #32002 ) ;
#18641 = DIRECTION ( 'NONE',  ( 0.000000000000000000, -0.8477344278896651319, -0.5304209081197519549 ) ) ;
#18642 = DIRECTION ( 'NONE',  ( 0.000000000000000000, 0.000000000000000000, 1.000000000000000000 ) ) ;
#18643 = ORIENTED_EDGE ( 'NONE', *, *, #12541, .T. ) ;
#18644 = CARTESIAN_POINT ( 'NONE',  ( 0.3461262719736147297, -4.658553426539303821, -3.671615880910379381 ) ) ;
#18645 = ORIENTED_EDGE ( 'NONE', *, *, #11194, .F. ) ;
#18646 = AXIS2_PLACEMENT_3D ( 'NONE', #18720, #11484, #11713 ) ;
#18647 = ORIENTED_EDGE ( 'NONE', *, *, #42765, .T. ) ;
#18648 = CIRCLE ( 'NONE', #39492, 1.399999999999998579 ) ;
#18649 = CARTESIAN_POINT ( 'NONE',  ( 18.00000000000000355, -34.03046037009278280, 33.13733193845793323 ) ) ;
#18650 = ADVANCED_FACE ( 'NONE', ( #41193 ), #13818, .F. ) ;
#18651 = CARTESIAN_POINT ( 'NONE',  ( -40.35386350238496789, 31.00000000000000355, 69.65762217234957632 ) ) ;
#18652 = ORIENTED_EDGE ( 'NONE', *, *, #605, .T. ) ;
#18653 = CARTESIAN_POINT ( 'NONE',  ( -4.000000000000000000, -2.472261339043343220, -3.687027428081192326 ) ) ;
#18654 = ADVANCED_FACE ( 'NONE', ( #24459 ), #24671, .T. ) ;
#18655 = CIRCLE ( 'NONE', #13729, 120.5010000000000190 ) ;
#18656 = ADVANCED_FACE ( 'NONE', ( #8921 ), #38790, .F. ) ;
#18657 = EDGE_CURVE ( 'NONE', #26205, #36343, #38201, .T. ) ;
#18658 = EDGE_CURVE ( 'NONE', #12090, #36312, #12001, .T. ) ;
#18659 = DIRECTION ( 'NONE',  ( -1.000000000000000000, 0.000000000000000000, -0.000000000000000000 ) ) ;
#18660 = ORIENTED_EDGE ( 'NONE', *, *, #33118, .T. ) ;
#18661 = CARTESIAN_POINT ( 'NONE',  ( 4.207491450040567571, -2.029819825146485179, -3.671670828759567407 ) ) ;
#18662 = CIRCLE ( 'NONE', #13048, 15.00000000000000000 ) ;
#18663 = DIRECTION ( 'NONE',  ( -1.000000000000000000, 0.000000000000000000, 0.000000000000000000 ) ) ;
#18664 = AXIS2_PLACEMENT_3D ( 'NONE', #41559, #18487, #8404 ) ;
#18665 = CARTESIAN_POINT ( 'NONE',  ( 23.62253089228586234, 31.00000000000000355, -11.62353008834390167 ) ) ;
#18667 = CARTESIAN_POINT ( 'NONE',  ( 17.99999999999999645, 0.000000000000000000, 0.000000000000000000 ) ) ;
#18666 = CARTESIAN_POINT ( 'NONE',  ( 0.000000000000000000, 110.1579703617966430, 21.29539948940285043 ) ) ;
#18668 = CARTESIAN_POINT ( 'NONE',  ( -91.96080130434580724, -14.05525454449571043, 14.45886780445738218 ) ) ;
#18669 = CARTESIAN_POINT ( 'NONE',  ( 0.000000000000000000, -30.78424799127063238, -6.672111855473501940 ) ) ;
#18670 = EDGE_LOOP ( 'NONE', ( #30660, #2270, #28261, #5740 ) ) ;
#18671 =( NAMED_UNIT ( * ) PLANE_ANGLE_UNIT ( ) SI_UNIT ( $, .RADIAN. ) );
#18672 = DIRECTION ( 'NONE',  ( -1.000000000000000000, 0.000000000000000000, 0.000000000000000000 ) ) ;
#18673 = ORIENTED_EDGE ( 'NONE', *, *, #22259, .F. ) ;
#18674 = CARTESIAN_POINT ( 'NONE',  ( 17.99999999999999645, -66.49630760163542220, -90.36876423296052963 ) ) ;
#18675 = CARTESIAN_POINT ( 'NONE',  ( 90.64482129758324902, 31.00000000000000000, 30.77200948131585889 ) ) ;
#18676 = CYLINDRICAL_SURFACE ( 'NONE', #7908, 2.649999999999985700 ) ;
#18677 = CIRCLE ( 'NONE', #11698, 20.00000000000000711 ) ;
#18678 = ORIENTED_EDGE ( 'NONE', *, *, #15937, .F. ) ;
#18679 = CARTESIAN_POINT ( 'NONE',  ( -28.96462450050677973, 40.00000000000000000, -9.827991688575851370 ) ) ;
#18680 = CARTESIAN_POINT ( 'NONE',  ( -10.41556553088919834, 40.00000000000000000, 38.62046602037417387 ) ) ;
#18681 = AXIS2_PLACEMENT_3D ( 'NONE', #40830, #475, #30827 ) ;
#18682 = CIRCLE ( 'NONE', #1198, 59.00000000000000711 ) ;
#18683 = ORIENTED_EDGE ( 'NONE', *, *, #20845, .F. ) ;
#18684 = VECTOR ( 'NONE', #16519, 1000.000000000000000 ) ;
#18685 = ORIENTED_EDGE ( 'NONE', *, *, #32026, .F. ) ;
#18686 = CARTESIAN_POINT ( 'NONE',  ( 53.30287614962722387, -35.35525454449572180, 69.29271901957299917 ) ) ;
#18687 = DIRECTION ( 'NONE',  ( 0.000000000000000000, 0.000000000000000000, 1.000000000000000000 ) ) ;
#18688 = CARTESIAN_POINT ( 'NONE',  ( 17.99999999999999645, 13.00789606333472470, 115.2683592318615382 ) ) ;
#18689 = AXIS2_PLACEMENT_3D ( 'NONE', #9721, #28949, #5792 ) ;
#18690 = DIRECTION ( 'NONE',  ( 0.000000000000000000, 0.000000000000000000, 1.000000000000000000 ) ) ;
#18691 = DIRECTION ( 'NONE',  ( 1.000000000000000000, -0.000000000000000000, 0.000000000000000000 ) ) ;
#18692 = ORIENTED_EDGE ( 'NONE', *, *, #22511, .F. ) ;
#18693 = CARTESIAN_POINT ( 'NONE',  ( -12.55910585664918422, 0.7408941433508191565, -1.199999999999999956 ) ) ;
#18694 = VERTEX_POINT ( 'NONE', #38566 ) ;
#18695 = CARTESIAN_POINT ( 'NONE',  ( -15.99999999999997691, 39.99999999999999289, -4.499999999999995559 ) ) ;
#18696 = CARTESIAN_POINT ( 'NONE',  ( 0.000000000000000000, 0.000000000000000000, 0.000000000000000000 ) ) ;
#18697 = APPLICATION_CONTEXT ( 'automotive_design' ) ;
#18698 = CIRCLE ( 'NONE', #16582, 4.250000000000000000 ) ;
#18699 = CARTESIAN_POINT ( 'NONE',  ( 18.00000000000000355, 43.55304910509406113, 28.41006711800000062 ) ) ;
#18700 = DIRECTION ( 'NONE',  ( 1.000000000000000000, -1.058513553088275437E-16, 0.000000000000000000 ) ) ;
#18701 = ORIENTED_EDGE ( 'NONE', *, *, #39473, .T. ) ;
#18702 = ORIENTED_EDGE ( 'NONE', *, *, #27368, .F. ) ;
#18703 = FACE_OUTER_BOUND ( 'NONE', #23639, .T. ) ;
#18704 = ORIENTED_EDGE ( 'NONE', *, *, #25722, .F. ) ;
#18706 = VERTEX_POINT ( 'NONE', #31409 ) ;
#18705 = DIRECTION ( 'NONE',  ( -1.000000000000000000, 0.000000000000000000, 0.000000000000000000 ) ) ;
#18707 = CARTESIAN_POINT ( 'NONE',  ( -46.12092335262209986, 31.00000000000000355, 22.64177125690870795 ) ) ;
#18708 = ORIENTED_EDGE ( 'NONE', *, *, #17151, .F. ) ;
#18709 = DIRECTION ( 'NONE',  ( 1.000000000000000000, 0.000000000000000000, 0.000000000000000000 ) ) ;
#18710 = ADVANCED_FACE ( 'NONE', ( #9123 ), #15275, .T. ) ;
#18711 = EDGE_CURVE ( 'NONE', #5699, #35404, #35518, .T. ) ;
#18712 = AXIS2_PLACEMENT_3D ( 'NONE', #22524, #42100, #19038 ) ;
#18713 = CARTESIAN_POINT ( 'NONE',  ( -2.649999999999993694, -150.5000000000000284, 9.999999999999998224 ) ) ;
#18714 = ADVANCED_FACE ( 'NONE', ( #5634 ), #21844, .T. ) ;
#18715 = ORIENTED_EDGE ( 'NONE', *, *, #22030, .F. ) ;
#18716 = VECTOR ( 'NONE', #19925, 1000.000000000000000 ) ;
#18717 = CARTESIAN_POINT ( 'NONE',  ( -32.59403919554602425, 40.00000000000000000, -66.35267222978370683 ) ) ;
#18718 = VECTOR ( 'NONE', #41751, 1000.000000000000000 ) ;
#18719 = CARTESIAN_POINT ( 'NONE',  ( 17.99999999999999645, -116.4607004671430417, 30.94182036827165660 ) ) ;
#18720 = CARTESIAN_POINT ( 'NONE',  ( -15.99999999999997691, 17.11489954122026447, 5.571627607371296764E-15 ) ) ;
#18721 = ORIENTED_EDGE ( 'NONE', *, *, #9037, .F. ) ;
#18722 = DIRECTION ( 'NONE',  ( 0.000000000000000000, 0.000000000000000000, 1.000000000000000000 ) ) ;
#18723 = ORIENTED_EDGE ( 'NONE', *, *, #26843, .T. ) ;
#18724 =( LENGTH_UNIT ( ) NAMED_UNIT ( * ) SI_UNIT ( .MILLI., .METRE. ) );
#18725 = CARTESIAN_POINT ( 'NONE',  ( 0.000000000000000000, 47.31079789947627745, -105.9135893174946119 ) ) ;
#18726 = DIRECTION ( 'NONE',  ( -1.000000000000000000, -0.000000000000000000, -0.000000000000000000 ) ) ;
#18727 = CIRCLE ( 'NONE', #42314, 120.5010000000000474 ) ;
#18728 = ADVANCED_FACE ( 'NONE', ( #31612 ), #8693, .F. ) ;
#18729 = CARTESIAN_POINT ( 'NONE',  ( -34.23962737045593485, 31.00000000000000355, 59.30561363632230609 ) ) ;
#18730 = DIRECTION ( 'NONE',  ( 0.000000000000000000, 0.000000000000000000, 1.000000000000000000 ) ) ;
#18731 = ORIENTED_EDGE ( 'NONE', *, *, #41616, .T. ) ;
#18732 = DIRECTION ( 'NONE',  ( 0.000000000000000000, 0.000000000000000000, 1.000000000000000000 ) ) ;
#18733 = ORIENTED_EDGE ( 'NONE', *, *, #42990, .F. ) ;
#18734 = LINE ( 'NONE', #31779, #26360 ) ;
#18735 = FACE_OUTER_BOUND ( 'NONE', #14047, .T. ) ;
#18736 = CARTESIAN_POINT ( 'NONE',  ( 28.55926749297819711, 31.00000000000000355, 84.46800049165048563 ) ) ;
#18737 = CARTESIAN_POINT ( 'NONE',  ( 53.86549405311984628, 40.00000000000000000, 70.40131829845091715 ) ) ;
#18738 = DIRECTION ( 'NONE',  ( -1.000000000000000000, 0.000000000000000000, -0.000000000000000000 ) ) ;
#18739 = EDGE_CURVE ( 'NONE', #12013, #12125, #32047, .T. ) ;
#18740 = CIRCLE ( 'NONE', #13188, 13.60000000000000142 ) ;
#18741 = AXIS2_PLACEMENT_3D ( 'NONE', #41348, #35242, #5370 ) ;
#18742 = EDGE_LOOP ( 'NONE', ( #485, #16152, #36293, #8454 ) ) ;
#18743 = CARTESIAN_POINT ( 'NONE',  ( 0.000000000000000000, 0.000000000000000000, 0.000000000000000000 ) ) ;
#18744 = EDGE_LOOP ( 'NONE', ( #4005, #21586, #16483, #23849 ) ) ;
#18745 = AXIS2_PLACEMENT_3D ( 'NONE', #39960, #36060, #23438 ) ;
#18746 = DIRECTION ( 'NONE',  ( 0.000000000000000000, 0.000000000000000000, 1.000000000000000000 ) ) ;
#18747 = DIRECTION ( 'NONE',  ( 1.000000000000000000, 0.000000000000000000, 0.000000000000000000 ) ) ;
#18748 = CIRCLE ( 'NONE', #32605, 4.000000000000000000 ) ;
#18750 = ORIENTED_EDGE ( 'NONE', *, *, #41298, .F. ) ;
#18749 = CARTESIAN_POINT ( 'NONE',  ( -10.00000000000000000, 0.000000000000000000, 0.000000000000000000 ) ) ;
#18751 = CARTESIAN_POINT ( 'NONE',  ( 0.000000000000000000, 0.000000000000000000, 0.000000000000000000 ) ) ;
#18752 = ORIENTED_EDGE ( 'NONE', *, *, #37646, .T. ) ;
#18753 = DIRECTION ( 'NONE',  ( 1.000000000000000000, 0.000000000000000000, 0.000000000000000000 ) ) ;
#18754 = CARTESIAN_POINT ( 'NONE',  ( 18.00000000000000355, 39.55064067543064965, 25.36340625197373555 ) ) ;
#18755 = DIRECTION ( 'NONE',  ( -1.000000000000000000, 0.000000000000000000, 0.000000000000000000 ) ) ;
#18756 = ORIENTED_EDGE ( 'NONE', *, *, #29533, .T. ) ;
#18757 = CARTESIAN_POINT ( 'NONE',  ( 26.62151981922249533, 31.00000000000000355, -3.482817046706074393 ) ) ;
#18758 = DIRECTION ( 'NONE',  ( 0.000000000000000000, 0.000000000000000000, 1.000000000000000000 ) ) ;
#18759 = EDGE_CURVE ( 'NONE', #17938, #22817, #10334, .T. ) ;
#18761 = DIRECTION ( 'NONE',  ( -1.000000000000000000, 2.668805347656627603E-17, 0.000000000000000000 ) ) ;
#18760 = DIRECTION ( 'NONE',  ( 1.000000000000000000, 0.000000000000000000, 0.000000000000000000 ) ) ;
#18762 = VERTEX_POINT ( 'NONE', #22049 ) ;
#18763 = DIRECTION ( 'NONE',  ( 0.000000000000000000, 0.000000000000000000, 1.000000000000000000 ) ) ;
#18764 = CARTESIAN_POINT ( 'NONE',  ( 1.039096088315723056E-14, -6.912265343809663812E-14, -26.00000000000000355 ) ) ;
#18765 = CARTESIAN_POINT ( 'NONE',  ( 41.62382930722196051, 40.00000000000000000, -20.43270582883756248 ) ) ;
#18766 = CARTESIAN_POINT ( 'NONE',  ( 0.000000000000000000, 0.000000000000000000, 0.000000000000000000 ) ) ;
#18767 = CIRCLE ( 'NONE', #1285, 14.91999999999999815 ) ;
#18768 = AXIS2_PLACEMENT_3D ( 'NONE', #6488, #23128, #6282 ) ;
#18769 = EDGE_CURVE ( 'NONE', #19587, #815, #28499, .T. ) ;
#18770 = DIRECTION ( 'NONE',  ( 0.000000000000000000, 0.000000000000000000, 1.000000000000000000 ) ) ;
#18771 = DIRECTION ( 'NONE',  ( 0.000000000000000000, 0.000000000000000000, 1.000000000000000000 ) ) ;
#18772 = B_SPLINE_CURVE_WITH_KNOTS ( 'NONE', 3,
 ( #15734, #19234, #39885, #9366, #39676, #12880 ),
 .UNSPECIFIED., .F., .F.,
 ( 4, 2, 4 ),
 ( 4.336808689942017736E-19, 0.0002095117440854729585, 0.0004190234881709454834 ),
 .UNSPECIFIED. ) ;
#18773 = EDGE_LOOP ( 'NONE', ( #36393, #11102, #25973, #26236 ) ) ;
#18774 = AXIS2_PLACEMENT_3D ( 'NONE', #1827, #41753, #14525 ) ;
#18775 = CARTESIAN_POINT ( 'NONE',  ( 4.236525694536557474, -2.416953475386482530, -3.751298745799839462 ) ) ;
#18776 = EDGE_CURVE ( 'NONE', #35634, #23198, #22933, .T. ) ;
#18777 = ORIENTED_EDGE ( 'NONE', *, *, #19288, .F. ) ;
#18778 = CARTESIAN_POINT ( 'NONE',  ( 17.99999999999999645, 23.21237537461745859, 109.7700237000592836 ) ) ;
#18779 = LINE ( 'NONE', #32033, #28280 ) ;
#18780 = EDGE_CURVE ( 'NONE', #10372, #14556, #34719, .T. ) ;
#18781 = CARTESIAN_POINT ( 'NONE',  ( -35.44024466369167925, 31.00000000000000355, -20.45798383175513635 ) ) ;
#18782 = ORIENTED_EDGE ( 'NONE', *, *, #9119, .F. ) ;
#18783 = CARTESIAN_POINT ( 'NONE',  ( 17.99999999999999645, 67.32409792376626001, -89.75376489259298296 ) ) ;
#18784 = VERTEX_POINT ( 'NONE', #8481 ) ;
#18785 = LINE ( 'NONE', #28781, #35815 ) ;
#18786 = CARTESIAN_POINT ( 'NONE',  ( 50.95389515256417923, 31.00000000000000355, -66.42840393140320998 ) ) ;
#18787 = ORIENTED_EDGE ( 'NONE', *, *, #11076, .F. ) ;
#18788 = CARTESIAN_POINT ( 'NONE',  ( 35.58199112953183629, 31.00000000000000355, 46.53705319858424616 ) ) ;
#18789 = CARTESIAN_POINT ( 'NONE',  ( 24.08498528996878107, 40.00000000000000000, -89.94621034038658536 ) ) ;
#18790 = ORIENTED_EDGE ( 'NONE', *, *, #17278, .F. ) ;
#18791 = EDGE_CURVE ( 'NONE', #35178, #42713, #40960, .T. ) ;
#18792 = CARTESIAN_POINT ( 'NONE',  ( 17.99999999999999645, 0.000000000000000000, 0.000000000000000000 ) ) ;
#18793 = DIRECTION ( 'NONE',  ( -1.000000000000000000, -0.000000000000000000, -0.000000000000000000 ) ) ;
#18794 = CARTESIAN_POINT ( 'NONE',  ( 18.00000000000000355, -17.08890430202782085, 43.76671000081940122 ) ) ;
#18795 = AXIS2_PLACEMENT_3D ( 'NONE', #8391, #18705, #25034 ) ;
#18796 = VECTOR ( 'NONE', #9290, 1000.000000000000000 ) ;
#18798 = ORIENTED_EDGE ( 'NONE', *, *, #29435, .F. ) ;
#18797 = DIRECTION ( 'NONE',  ( 2.932542530036133930E-17, 1.000000000000000000, -5.216001792149171863E-18 ) ) ;
#18799 = DIRECTION ( 'NONE',  ( -1.000000000000000000, -0.000000000000000000, 0.000000000000000000 ) ) ;
#18800 = CYLINDRICAL_SURFACE ( 'NONE', #29341, 36.00000000000000000 ) ;
#18801 = AXIS2_PLACEMENT_3D ( 'NONE', #27551, #24966, #34291 ) ;
#18802 = ORIENTED_EDGE ( 'NONE', *, *, #11753, .F. ) ;
#18803 = CARTESIAN_POINT ( 'NONE',  ( 49.83821931962687302, 40.00000000000000000, 43.70611527624207326 ) ) ;
#18804 = DIRECTION ( 'NONE',  ( 0.000000000000000000, 0.000000000000000000, 1.000000000000000000 ) ) ;
#18805 = ORIENTED_EDGE ( 'NONE', *, *, #30036, .F. ) ;
#18806 = DIRECTION ( 'NONE',  ( -1.000000000000000000, -0.000000000000000000, 0.000000000000000000 ) ) ;
#18807 = CARTESIAN_POINT ( 'NONE',  ( 18.00000000000000355, 2.123073309835852296, -47.45152853935331905 ) ) ;
#18808 = VERTEX_POINT ( 'NONE', #18998 ) ;
#18809 = EDGE_CURVE ( 'NONE', #20992, #25091, #28582, .T. ) ;
#18810 = ORIENTED_EDGE ( 'NONE', *, *, #4697, .F. ) ;
#18811 = CARTESIAN_POINT ( 'NONE',  ( 17.99999999999999645, 0.000000000000000000, 0.000000000000000000 ) ) ;
#18812 = ORIENTED_EDGE ( 'NONE', *, *, #22702, .T. ) ;
#18813 = DIRECTION ( 'NONE',  ( 0.000000000000000000, 9.408669700213191589E-16, -1.000000000000000000 ) ) ;
#18814 = DIRECTION ( 'NONE',  ( 0.000000000000000000, 0.000000000000000000, -1.000000000000000000 ) ) ;
#18815 = DIRECTION ( 'NONE',  ( 0.000000000000000000, 0.5264321628773568351, -0.8502171357296134380 ) ) ;
#18816 = DIRECTION ( 'NONE',  ( 0.000000000000000000, -0.05322217484216513333, -0.9985826956767627216 ) ) ;
#18817 = ORIENTED_EDGE ( 'NONE', *, *, #34136, .F. ) ;
#18818 = CARTESIAN_POINT ( 'NONE',  ( 0.000000000000000000, -31.81777574834303124, -2.898764365605651427 ) ) ;
#18819 = EDGE_CURVE ( 'NONE', #37013, #39320, #9645, .T. ) ;
#18820 = ORIENTED_EDGE ( 'NONE', *, *, #940, .T. ) ;
#18821 = CARTESIAN_POINT ( 'NONE',  ( 17.99999999999999645, 0.000000000000000000, 0.000000000000000000 ) ) ;
#18822 = TOROIDAL_SURFACE ( 'NONE', #39671, 4.000000000000000000, 0.2500000000000000000 ) ;
#18823 = ORIENTED_EDGE ( 'NONE', *, *, #38827, .T. ) ;
#18824 = VECTOR ( 'NONE', #27986, 1000.000000000000000 ) ;
#18825 = CARTESIAN_POINT ( 'NONE',  ( -31.75000000000000000, -18.77999999999999048, 2.299886688798728323E-15 ) ) ;
#18826 = ADVANCED_FACE ( 'NONE', ( #8277 ), #5431, .F. ) ;
#18827 = LINE ( 'NONE', #19026, #8634 ) ;
#18828 = AXIS2_PLACEMENT_3D ( 'NONE', #21688, #28206, #24523 ) ;
#18829 = CARTESIAN_POINT ( 'NONE',  ( 1.054598134147292892E-12, 17.99999999999998934, 150.5000000000000284 ) ) ;
#18830 = DIRECTION ( 'NONE',  ( -0.000000000000000000, -0.000000000000000000, 1.000000000000000000 ) ) ;
#18831 = CARTESIAN_POINT ( 'NONE',  ( 28.34477777927418529, 31.00000000000000355, 36.93558740410973229 ) ) ;
#18832 = ORIENTED_EDGE ( 'NONE', *, *, #16971, .T. ) ;
#18833 = DIRECTION ( 'NONE',  ( 0.000000000000000000, 0.000000000000000000, 1.000000000000000000 ) ) ;
#18834 = ORIENTED_EDGE ( 'NONE', *, *, #28108, .F. ) ;
#18835 = CARTESIAN_POINT ( 'NONE',  ( -19.97695672607123640, 40.00000000000000000, -58.81104016858105155 ) ) ;
#18836 = EDGE_CURVE ( 'NONE', #39379, #34690, #15935, .T. ) ;
#18837 = CARTESIAN_POINT ( 'NONE',  ( 0.000000000000000000, 0.000000000000000000, 0.000000000000000000 ) ) ;
#18838 = CARTESIAN_POINT ( 'NONE',  ( 18.00000000000000355, -13.56094713063537682, -50.20060470671753450 ) ) ;
#18839 = EDGE_CURVE ( 'NONE', #4630, #4850, #23119, .T. ) ;
#18840 = CARTESIAN_POINT ( 'NONE',  ( 18.00000000000000355, 39.55064067543099071, -25.36340625197318488 ) ) ;
#18841 = DIRECTION ( 'NONE',  ( 0.000000000000000000, -0.6736956436465636466, 0.7390089172206532053 ) ) ;
#18842 = VERTEX_POINT ( 'NONE', #16571 ) ;
#18843 = CARTESIAN_POINT ( 'NONE',  ( -39.89583333501392559, 40.00000000000000000, 2.617993869485681468 ) ) ;
#18844 = ORIENTED_EDGE ( 'NONE', *, *, #39114, .F. ) ;
#18845 = CARTESIAN_POINT ( 'NONE',  ( 0.000000000000000000, -62.45178862086279992, 93.20969140437486544 ) ) ;
#18847 = DIRECTION ( 'NONE',  ( 0.000000000000000000, 0.000000000000000000, 1.000000000000000000 ) ) ;
#18846 = CIRCLE ( 'NONE', #36185, 59.00000000000000000 ) ;
#18848 = EDGE_LOOP ( 'NONE', ( #18154, #7561, #31316, #10066 ) ) ;
#18849 = AXIS2_PLACEMENT_3D ( 'NONE', #41917, #25384, #12698 ) ;
#18850 = DIRECTION ( 'NONE',  ( 0.000000000000000000, -0.2631025642275088838, -0.9647678688145193693 ) ) ;
#18851 = ORIENTED_EDGE ( 'NONE', *, *, #22463, .T. ) ;
#18852 = CARTESIAN_POINT ( 'NONE',  ( 3.333333333333332593, 2.694301256218250007, -3.300726591567078483 ) ) ;
#18853 = ORIENTED_EDGE ( 'NONE', *, *, #19708, .T. ) ;
#18854 = EDGE_CURVE ( 'NONE', #7746, #34978, #34030, .T. ) ;
#18855 = ORIENTED_EDGE ( 'NONE', *, *, #17738, .F. ) ;
#18856 = DIRECTION ( 'NONE',  ( -1.000000000000000000, 0.000000000000000000, 0.000000000000000000 ) ) ;
#18857 = CARTESIAN_POINT ( 'NONE',  ( -64.43604943162229404, 31.00000000000000711, 49.29347324003089881 ) ) ;
#18858 = VERTEX_POINT ( 'NONE', #26786 ) ;
#18859 = DIRECTION ( 'NONE',  ( 0.000000000000000000, 0.000000000000000000, 1.000000000000000000 ) ) ;
#18860 = CYLINDRICAL_SURFACE ( 'NONE', #10132, 13.59999999999999964 ) ;
#18861 = ORIENTED_EDGE ( 'NONE', *, *, #7402, .F. ) ;
#18862 = DIRECTION ( 'NONE',  ( 0.000000000000000000, 0.000000000000000000, 1.000000000000000000 ) ) ;
#18863 = EDGE_CURVE ( 'NONE', #18183, #9792, #36103, .T. ) ;
#18864 = CARTESIAN_POINT ( 'NONE',  ( -12.69999999999999929, 1.543054966925665076E-15, 12.59999999999999964 ) ) ;
#18865 = CARTESIAN_POINT ( 'NONE',  ( -15.43003214871278139, 31.00000000000000355, -17.59684744742187945 ) ) ;
#18866 = EDGE_CURVE ( 'NONE', #40502, #3181, #27771, .T. ) ;
#18868 = FACE_OUTER_BOUND ( 'NONE', #3111, .T. ) ;
#18867 = CARTESIAN_POINT ( 'NONE',  ( 2.250206802516403481, -2.055254544495723312, 2.972870684497274762 ) ) ;
#18869 = DIRECTION ( 'NONE',  ( -1.000000000000000000, 0.000000000000000000, 0.000000000000000000 ) ) ;
#18870 = DIRECTION ( 'NONE',  ( -1.000000000000000000, -0.000000000000000000, 0.000000000000000000 ) ) ;
#18871 = ORIENTED_EDGE ( 'NONE', *, *, #30788, .F. ) ;
#18872 = SURFACE_SIDE_STYLE ('',( #11873 ) ) ;
#18873 = CARTESIAN_POINT ( 'NONE',  ( 0.000000000000000000, -111.7974656912329436, -9.465682155096647676 ) ) ;
#18874 = CIRCLE ( 'NONE', #32067, 59.00000000000002132 ) ;
#18875 = ORIENTED_EDGE ( 'NONE', *, *, #9099, .F. ) ;
#18876 = DIRECTION ( 'NONE',  ( 1.000000000000000000, 0.000000000000000000, -0.000000000000000000 ) ) ;
#18877 = AXIS2_PLACEMENT_3D ( 'NONE', #17430, #30709, #27662 ) ;
#18878 = CARTESIAN_POINT ( 'NONE',  ( -43.52407497442469264, 31.00000000000000355, 88.29422169633753015 ) ) ;
#18879 = AXIS2_PLACEMENT_3D ( 'NONE', #42294, #8715, #28808 ) ;
#18880 = LINE ( 'NONE', #42143, #34220 ) ;
#18881 = ORIENTED_EDGE ( 'NONE', *, *, #9173, .F. ) ;
#18882 = CARTESIAN_POINT ( 'NONE',  ( -30.10416666442597844, 40.00000000000000000, -1.963495399902747574 ) ) ;
#18883 = CARTESIAN_POINT ( 'NONE',  ( -37.12595630543398073, 40.00000000000000000, 18.22532657727797911 ) ) ;
#18884 = VERTEX_POINT ( 'NONE', #9562 ) ;
#18885 = EDGE_CURVE ( 'NONE', #20227, #31507, #13125, .T. ) ;
#18886 = ORIENTED_EDGE ( 'NONE', *, *, #38829, .F. ) ;
#18887 = CARTESIAN_POINT ( 'NONE',  ( 0.000000000000000000, 0.000000000000000000, 0.000000000000000000 ) ) ;
#18888 = DIRECTION ( 'NONE',  ( 1.000000000000000000, -0.000000000000000000, 0.000000000000000000 ) ) ;
#18889 = ADVANCED_FACE ( 'NONE', ( #23543 ), #2761, .T. ) ;
#18890 =( LENGTH_UNIT ( ) NAMED_UNIT ( * ) SI_UNIT ( .MILLI., .METRE. ) );
#18891 = EDGE_CURVE ( 'NONE', #9595, #14740, #33314, .T. ) ;
#18892 = EDGE_CURVE ( 'NONE', #22284, #41100, #39587, .T. ) ;
#18893 = EDGE_CURVE ( 'NONE', #14755, #9269, #2556, .T. ) ;
#18894 = DIRECTION ( 'NONE',  ( -1.000000000000000000, 0.000000000000000000, 0.000000000000000000 ) ) ;
#18895 = CARTESIAN_POINT ( 'NONE',  ( -3.996523416598931009E-15, 2.658563593772952281E-14, 10.00000000000000178 ) ) ;
#18896 = ORIENTED_EDGE ( 'NONE', *, *, #3884, .T. ) ;
#18897 = DIRECTION ( 'NONE',  ( -0.000000000000000000, -0.000000000000000000, 1.000000000000000000 ) ) ;
#18898 = ORIENTED_EDGE ( 'NONE', *, *, #30088, .F. ) ;
#18899 = CARTESIAN_POINT ( 'NONE',  ( 0.000000000000000000, 95.38615066514064722, -59.07414607872728141 ) ) ;
#18900 = DIRECTION ( 'NONE',  ( 1.000000000000000000, 0.000000000000000000, -6.546126324440850663E-16 ) ) ;
#18901 = CARTESIAN_POINT ( 'NONE',  ( 18.00000000000000355, -46.87740477351715640, -3.172455868805708956 ) ) ;
#18902 = CARTESIAN_POINT ( 'NONE',  ( 22.90854556226730310, -34.05525454449573175, -74.83297477053802993 ) ) ;
#18903 = ORIENTED_EDGE ( 'NONE', *, *, #8368, .T. ) ;
#18904 = ORIENTED_EDGE ( 'NONE', *, *, #25429, .T. ) ;
#18905 = AXIS2_PLACEMENT_3D ( 'NONE', #3391, #13908, #16763 ) ;
#18906 = DIRECTION ( 'NONE',  ( -1.000000000000000000, 0.000000000000000000, 0.000000000000000000 ) ) ;
#18907 = VERTEX_POINT ( 'NONE', #39423 ) ;
#18909 = ORIENTED_EDGE ( 'NONE', *, *, #37550, .T. ) ;
#18908 = CARTESIAN_POINT ( 'NONE',  ( 1.039096088315723056E-14, -6.912265343809663812E-14, -26.00000000000000355 ) ) ;
#18910 = VECTOR ( 'NONE', #31751, 1000.000000000000000 ) ;
#18911 = CARTESIAN_POINT ( 'NONE',  ( -49.95450512538511134, 31.00000000000000355, 13.28959769214884545 ) ) ;
#18913 = VERTEX_POINT ( 'NONE', #29214 ) ;
#18912 = AXIS2_PLACEMENT_3D ( 'NONE', #7149, #3646, #9580 ) ;
#18914 = FACE_OUTER_BOUND ( 'NONE', #41590, .T. ) ;
#18915 = CIRCLE ( 'NONE', #30736, 47.49900000000000944 ) ;
#18916 = DIRECTION ( 'NONE',  ( 0.000000000000000000, 0.000000000000000000, 1.000000000000000000 ) ) ;
#18917 = EDGE_CURVE ( 'NONE', #19384, #6563, #13283, .T. ) ;
#18918 = ORIENTED_EDGE ( 'NONE', *, *, #40, .T. ) ;
#18919 = CARTESIAN_POINT ( 'NONE',  ( -71.72626536479072001, 40.00000000000000711, -9.557116936239163252 ) ) ;
#18921 = CARTESIAN_POINT ( 'NONE',  ( 0.000000000000000000, 94.52951811191560694, 67.23221107124935259 ) ) ;
#18920 = DIRECTION ( 'NONE',  ( -1.000000000000000000, 0.000000000000000000, -0.000000000000000000 ) ) ;
#18922 = DIRECTION ( 'NONE',  ( -1.000000000000000000, 0.000000000000000000, 0.000000000000000000 ) ) ;
#18923 = ORIENTED_EDGE ( 'NONE', *, *, #14745, .F. ) ;
#18924 = CARTESIAN_POINT ( 'NONE',  ( 2.039745330509125010E-13, -150.5000000000013642, 6.999999999999586109 ) ) ;
#18925 = ORIENTED_EDGE ( 'NONE', *, *, #20258, .F. ) ;
#18926 = DIRECTION ( 'NONE',  ( 0.000000000000000000, 0.000000000000000000, 1.000000000000000000 ) ) ;
#18927 = FACE_BOUND ( 'NONE', #37026, .T. ) ;
#18928 = CIRCLE ( 'NONE', #4122, 31.49899999999999878 ) ;
#18929 = CARTESIAN_POINT ( 'NONE',  ( -56.48955861152074220, 31.00000000000000711, -43.32902275382048174 ) ) ;
#18931 = CARTESIAN_POINT ( 'NONE',  ( 17.99999999999999645, -94.52951811191606168, 67.23221107124869889 ) ) ;
#18930 = DIRECTION ( 'NONE',  ( 0.000000000000000000, -1.246648735278247733E-14, -1.000000000000000000 ) ) ;
#18932 = ORIENTED_EDGE ( 'NONE', *, *, #25551, .F. ) ;
#18933 = AXIS2_PLACEMENT_3D ( 'NONE', #18924, #22196, #32390 ) ;
#18934 = FACE_OUTER_BOUND ( 'NONE', #5583, .T. ) ;
#18935 = CIRCLE ( 'NONE', #7035, 120.5010000000000332 ) ;
#18936 = EDGE_LOOP ( 'NONE', ( #22277, #40130, #10621, #16698 ) ) ;
#18937 = CARTESIAN_POINT ( 'NONE',  ( 17.99999999999999645, -8.827181066045094227, -120.1772519049560231 ) ) ;
#18938 = CARTESIAN_POINT ( 'NONE',  ( 0.000000000000000000, -18.35539002514457252, 110.6858262410709273 ) ) ;
#18939 = EDGE_CURVE ( 'NONE', #17680, #35461, #20849, .T. ) ;
#18940 = CARTESIAN_POINT ( 'NONE',  ( 73.86091552538547944, 31.00000000000000000, 64.94433634442138725 ) ) ;
#18941 = CARTESIAN_POINT ( 'NONE',  ( -26.02152878260477564, 40.00000000000000000, 96.68563202207252516 ) ) ;
#18942 = ADVANCED_FACE ( 'NONE', ( #12630 ), #26151, .F. ) ;
#18943 = ADVANCED_FACE ( 'NONE', ( #42691 ), #19621, .F. ) ;
#18944 = AXIS2_PLACEMENT_3D ( 'NONE', #23496, #7294, #36756 ) ;
#18945 = DIRECTION ( 'NONE',  ( 1.000000000000000000, 0.000000000000000000, 0.000000000000000000 ) ) ;
#18946 = EDGE_CURVE ( 'NONE', #10833, #21049, #26388, .T. ) ;
#18947 = EDGE_LOOP ( 'NONE', ( #9516, #22274, #26783, #935 ) ) ;
#18948 = CARTESIAN_POINT ( 'NONE',  ( 18.00000000000000355, 46.87740477351718482, -3.172455868805370560 ) ) ;
#18949 = VERTEX_POINT ( 'NONE', #42912 ) ;
#18950 = TOROIDAL_SURFACE ( 'NONE', #21722, 11.08000000000000007, 0.08000000000000020983 ) ;
#18951 = DIRECTION ( 'NONE',  ( -1.000000000000000000, 0.000000000000000000, -0.000000000000000000 ) ) ;
#18953 = ORIENTED_EDGE ( 'NONE', *, *, #6026, .T. ) ;
#18952 = DIRECTION ( 'NONE',  ( 0.000000000000000000, -0.9980267284282708928, -0.06279051952932446223 ) ) ;
#18954 = DIRECTION ( 'NONE',  ( 1.000000000000000000, 0.000000000000000000, 0.000000000000000000 ) ) ;
#18955 = VERTEX_POINT ( 'NONE', #36367 ) ;
#18956 = CARTESIAN_POINT ( 'NONE',  ( 17.99999999999999645, 41.62036691425530677, 113.0850832732715787 ) ) ;
#18957 = DIRECTION ( 'NONE',  ( 1.000000000000000000, 0.000000000000000000, 0.000000000000000000 ) ) ;
#18958 = VECTOR ( 'NONE', #39249, 1000.000000000000000 ) ;
#18959 = CYLINDRICAL_SURFACE ( 'NONE', #36158, 59.00000000000000000 ) ;
#18960 = ORIENTED_EDGE ( 'NONE', *, *, #40878, .F. ) ;
#18961 = EDGE_CURVE ( 'NONE', #20768, #34974, #7557, .T. ) ;
#18962 = CARTESIAN_POINT ( 'NONE',  ( 18.71272080434062701, 31.00000000000000355, 21.38210947162711406 ) ) ;
#18963 = CARTESIAN_POINT ( 'NONE',  ( -10.00000000000000000, 0.000000000000000000, 0.000000000000000000 ) ) ;
#18965 = ORIENTED_EDGE ( 'NONE', *, *, #21503, .F. ) ;
#18964 = DIRECTION ( 'NONE',  ( 0.000000000000000000, 0.000000000000000000, 1.000000000000000000 ) ) ;
#18966 = VERTEX_POINT ( 'NONE', #127 ) ;
#18967 = DIRECTION ( 'NONE',  ( 0.000000000000000000, 0.8183027759081662467, 0.5747874102144109321 ) ) ;
#18968 = VECTOR ( 'NONE', #19697, 1000.000000000000000 ) ;
#18969 = DIRECTION ( 'NONE',  ( 0.000000000000000000, -0.2113826236296315608, 0.9774033898178652313 ) ) ;
#18970 = CARTESIAN_POINT ( 'NONE',  ( -26.91141215548883991, 40.00000000000000000, 30.57553017915055449 ) ) ;
#18971 = CARTESIAN_POINT ( 'NONE',  ( 0.000000000000000000, 107.2703412112699368, -32.88383143828351507 ) ) ;
#18972 = DIRECTION ( 'NONE',  ( 0.000000000000000000, 0.6845471059286846183, 0.7289686274214153272 ) ) ;
#18973 = AXIS2_PLACEMENT_3D ( 'NONE', #633, #30569, #37523 ) ;
#18974 = EDGE_CURVE ( 'NONE', #21541, #24620, #25693, .T. ) ;
#18975 = FACE_OUTER_BOUND ( 'NONE', #14695, .T. ) ;
#18976 = ORIENTED_EDGE ( 'NONE', *, *, #33861, .F. ) ;
#18977 = DIRECTION ( 'NONE',  ( 0.000000000000000000, 0.9048270524660175784, 0.4257792915650767673 ) ) ;
#18978 = ORIENTED_EDGE ( 'NONE', *, *, #11471, .T. ) ;
#18979 = CIRCLE ( 'NONE', #40484, 2.649999999999985700 ) ;
#18980 = CARTESIAN_POINT ( 'NONE',  ( 17.99999999999999645, 111.2721026680460596, 44.61974821237342326 ) ) ;
#18981 = CARTESIAN_POINT ( 'NONE',  ( 8.673617379884035472E-16, 4.618802153517012954, 0.000000000000000000 ) ) ;
#18982 = CARTESIAN_POINT ( 'NONE',  ( -29.26739590608564967, 31.00000000000000355, 25.68069354617348665 ) ) ;
#18983 = ORIENTED_EDGE ( 'NONE', *, *, #35187, .F. ) ;
#18984 = FILL_AREA_STYLE_COLOUR ( '', #30206 ) ;
#18985 = ORIENTED_EDGE ( 'NONE', *, *, #30859, .T. ) ;
#18986 = PRODUCT_DEFINITION_SHAPE ( 'NONE', 'NONE',  #43205 ) ;
#18987 = CARTESIAN_POINT ( 'NONE',  ( 17.99999999999999645, 96.25468616236661035, 72.49500943364525085 ) ) ;
#18988 = CARTESIAN_POINT ( 'NONE',  ( 29.96647033545507455, 31.00000000000000355, -88.27250603610892199 ) ) ;
#18989 = DIRECTION ( 'NONE',  ( 0.000000000000000000, 0.000000000000000000, -1.000000000000000000 ) ) ;
#18990 = ORIENTED_EDGE ( 'NONE', *, *, #40108, .F. ) ;
#18991 = CARTESIAN_POINT ( 'NONE',  ( 50.14038141241295676, 31.00000000000000355, 29.06424286984032435 ) ) ;
#18992 = EDGE_CURVE ( 'NONE', #37965, #3869, #11031, .T. ) ;
#18993 = CARTESIAN_POINT ( 'NONE',  ( -74.47060461443528823, 40.00000000000000711, 65.33029858165178894 ) ) ;
#18994 = ORIENTED_EDGE ( 'NONE', *, *, #2610, .F. ) ;
#18995 = CIRCLE ( 'NONE', #38456, 2.649999999999971934 ) ;
#18996 =( REPRESENTATION_RELATIONSHIP ('NONE','NONE', #330, #16840 ) REPRESENTATION_RELATIONSHIP_WITH_TRANSFORMATION ( #26827 )SHAPE_REPRESENTATION_RELATIONSHIP( ) );
#18997 = CARTESIAN_POINT ( 'NONE',  ( 1.600000000000000089, -12.75000000000000000, -1.199999999999999956 ) ) ;
#18998 = CARTESIAN_POINT ( 'NONE',  ( 47.90854556226721428, -12.05525454449572464, -74.83297477053847047 ) ) ;
#18999 = CARTESIAN_POINT ( 'NONE',  ( 0.000000000000000000, -24.22031524826050841, 109.5520369638036584 ) ) ;
#19001 = EDGE_LOOP ( 'NONE', ( #4889, #29601, #20364, #1989 ) ) ;
#19000 = CARTESIAN_POINT ( 'NONE',  ( 0.000000000000000000, -19.47322409167248480, -30.27859877001420941 ) ) ;
#19002 = CARTESIAN_POINT ( 'NONE',  ( 17.99999999999999645, 0.000000000000000000, 0.000000000000000000 ) ) ;
#19003 = DIRECTION ( 'NONE',  ( 0.000000000000000000, 0.000000000000000000, 1.000000000000000000 ) ) ;
#19004 = EDGE_CURVE ( 'NONE', #10253, #17463, #4674, .T. ) ;
#19005 = ORIENTED_EDGE ( 'NONE', *, *, #16994, .T. ) ;
#19006 = CARTESIAN_POINT ( 'NONE',  ( 70.67261647610648367, 39.99999999999999289, -24.00465245562410743 ) ) ;
#19007 = CARTESIAN_POINT ( 'NONE',  ( 17.99999999999999645, -18.25486108452607681, -25.66996392254292658 ) ) ;
#19008 = AXIS2_PLACEMENT_3D ( 'NONE', #9411, #32330, #42564 ) ;
#19009 = ORIENTED_EDGE ( 'NONE', *, *, #36140, .F. ) ;
#19010 = DIRECTION ( 'NONE',  ( 0.000000000000000000, 0.000000000000000000, 1.000000000000000000 ) ) ;
#19011 = ORIENTED_EDGE ( 'NONE', *, *, #33933, .F. ) ;
#19012 = ORIENTED_EDGE ( 'NONE', *, *, #15620, .T. ) ;
#19013 = DIRECTION ( 'NONE',  ( 1.000000000000000000, -3.336006684570782732E-17, 0.000000000000000000 ) ) ;
#19014 = VERTEX_POINT ( 'NONE', #41530 ) ;
#19015 = CARTESIAN_POINT ( 'NONE',  ( 8.999999999999998224, 28.35267316522815406, -22.18391138608678403 ) ) ;
#19016 = CARTESIAN_POINT ( 'NONE',  ( 17.99999999999999645, 56.51398178981825993, 96.92493144647468739 ) ) ;
#19017 = CARTESIAN_POINT ( 'NONE',  ( 2.500000000000000000, -1.178949249685214307, 2.042000000000001592 ) ) ;
#19018 = CARTESIAN_POINT ( 'NONE',  ( 0.000000000000000000, 0.000000000000000000, 0.000000000000000000 ) ) ;
#19019 = ORIENTED_EDGE ( 'NONE', *, *, #28081, .T. ) ;
#19020 = DIRECTION ( 'NONE',  ( 0.000000000000000000, 0.000000000000000000, -1.000000000000000000 ) ) ;
#19021 = UNCERTAINTY_MEASURE_WITH_UNIT (LENGTH_MEASURE( 1.000000000000000082E-05 ), #4648, 'distance_accuracy_value', 'NONE');
#19022 = ORIENTED_EDGE ( 'NONE', *, *, #40939, .T. ) ;
#19023 = CARTESIAN_POINT ( 'NONE',  ( 0.000000000000000000, -112.5120133921104753, -43.14554256761132223 ) ) ;
#19024 = ORIENTED_EDGE ( 'NONE', *, *, #3584, .T. ) ;
#19025 = DIRECTION ( 'NONE',  ( 0.000000000000000000, -0.9968120070307493474, -0.07978610555309334496 ) ) ;
#19026 = CARTESIAN_POINT ( 'NONE',  ( 2.059999999999998721, 0.000000000000000000, -0.3080913168122742518 ) ) ;
#19027 = DIRECTION ( 'NONE',  ( 1.053567635648676764E-14, -6.123233995736766036E-17, 1.000000000000000000 ) ) ;
#19028 = DIRECTION ( 'NONE',  ( 0.000000000000000000, -0.8747630845319559478, -0.4845508703326599775 ) ) ;
#19029 = CARTESIAN_POINT ( 'NONE',  ( 48.45771864870608425, 31.00000000000000355, 27.97524394371832202 ) ) ;
#19030 = CIRCLE ( 'NONE', #23193, 116.0000000000000000 ) ;
#19031 = ORIENTED_EDGE ( 'NONE', *, *, #30133, .T. ) ;
#19032 = CYLINDRICAL_SURFACE ( 'NONE', #6672, 59.00000000000000000 ) ;
#19033 = ORIENTED_EDGE ( 'NONE', *, *, #40077, .T. ) ;
#19034 = EDGE_CURVE ( 'NONE', #11917, #18562, #18740, .T. ) ;
#19035 = CARTESIAN_POINT ( 'NONE',  ( -7.547223091130065953, 40.00000000000000000, 57.33767041057931380 ) ) ;
#19036 = EDGE_CURVE ( 'NONE', #15115, #17938, #15968, .T. ) ;
#19037 = DIRECTION ( 'NONE',  ( 0.000000000000000000, -0.9510565162951500895, -0.3090169943749581094 ) ) ;
#19038 = DIRECTION ( 'NONE',  ( 0.000000000000000000, 0.5877852522924742473, -0.8090169943749466741 ) ) ;
#19039 = CYLINDRICAL_SURFACE ( 'NONE', #14196, 59.00000000000000000 ) ;
#19040 = CARTESIAN_POINT ( 'NONE',  ( 17.99999999999999645, 119.8996782608629985, 12.02323392193397211 ) ) ;
#19041 = EDGE_CURVE ( 'NONE', #33051, #34436, #3360, .T. ) ;
#19042 = CIRCLE ( 'NONE', #39877, 59.00000000000000000 ) ;
#19043 = ORIENTED_EDGE ( 'NONE', *, *, #20371, .F. ) ;
#19044 = CARTESIAN_POINT ( 'NONE',  ( -47.99616210117395099, 40.00000000000000000, 12.86278070621785119 ) ) ;
#19045 = CARTESIAN_POINT ( 'NONE',  ( 17.99999999999999645, 0.000000000000000000, 0.000000000000000000 ) ) ;
#19046 = DIRECTION ( 'NONE',  ( 0.000000000000000000, -0.9911528310040084166, 0.1327255272837126743 ) ) ;
#19047 = VERTEX_POINT ( 'NONE', #11240 ) ;
#19048 = EDGE_CURVE ( 'NONE', #32585, #10253, #36825, .T. ) ;
#19049 = DIRECTION ( 'NONE',  ( 1.000000000000000000, 0.000000000000000000, 0.000000000000000000 ) ) ;
#19050 = AXIS2_PLACEMENT_3D ( 'NONE', #21599, #4510, #38326 ) ;
#19051 = EDGE_CURVE ( 'NONE', #5141, #27385, #37516, .T. ) ;
#19052 = ORIENTED_EDGE ( 'NONE', *, *, #13241, .F. ) ;
#19053 = DIRECTION ( 'NONE',  ( -1.000000000000000000, -0.000000000000000000, 0.000000000000000000 ) ) ;
#19054 = ORIENTED_EDGE ( 'NONE', *, *, #11595, .F. ) ;
#19055 = AXIS2_PLACEMENT_3D ( 'NONE', #1038, #21405, #14831 ) ;
#19056 = EDGE_LOOP ( 'NONE', ( #3323, #9135, #7392, #8179 ) ) ;
#19057 = DIRECTION ( 'NONE',  ( 0.000000000000000000, -0.7525707698561306946, -0.6585113790650474197 ) ) ;
#19058 = CARTESIAN_POINT ( 'NONE',  ( 83.01093309086799366, 31.00000000000000000, 28.30804032755801458 ) ) ;
#19059 = ORIENTED_EDGE ( 'NONE', *, *, #2775, .T. ) ;
#19060 = CYLINDRICAL_SURFACE ( 'NONE', #37000, 47.49900000000000233 ) ;
#19061 = CARTESIAN_POINT ( 'NONE',  ( 109.0695705685756565, -106.4195705685758213, 6.999999999999666933 ) ) ;
#19062 = ORIENTED_EDGE ( 'NONE', *, *, #18428, .F. ) ;
#19063 = CARTESIAN_POINT ( 'NONE',  ( 18.00000000000000355, 0.000000000000000000, 0.000000000000000000 ) ) ;
#19064 = PRODUCT_DEFINITION_SHAPE ( 'NONE', 'NONE',  #43212 ) ;
#19065 = CARTESIAN_POINT ( 'NONE',  ( 5.200000000000002842, 3.306546357697854226E-16, 2.700000000000000622 ) ) ;
#19066 = EDGE_CURVE ( 'NONE', #27860, #32609, #27803, .T. ) ;
#19067 = DIRECTION ( 'NONE',  ( 0.000000000000000000, 0.3612416661871538093, -0.9324722294043554793 ) ) ;
#19068 = EDGE_CURVE ( 'NONE', #18244, #1564, #18082, .T. ) ;
#19070 = CARTESIAN_POINT ( 'NONE',  ( 0.000000000000000000, 0.000000000000000000, 0.000000000000000000 ) ) ;
#19069 = CARTESIAN_POINT ( 'NONE',  ( -17.77999999999999758, 0.000000000000000000, 0.000000000000000000 ) ) ;
#19071 = CARTESIAN_POINT ( 'NONE',  ( -16.73417733071809721, 31.00000000000000355, -12.82953315787133519 ) ) ;
#19072 = DIRECTION ( 'NONE',  ( 0.000000000000000000, 0.000000000000000000, 1.000000000000000000 ) ) ;
#19073 = ORIENTED_EDGE ( 'NONE', *, *, #7794, .T. ) ;
#19074 = AXIS2_PLACEMENT_3D ( 'NONE', #3810, #17195, #13911 ) ;
#19075 = DIRECTION ( 'NONE',  ( 0.000000000000000000, 0.000000000000000000, 1.000000000000000000 ) ) ;
#19076 = VERTEX_POINT ( 'NONE', #7942 ) ;
#19077 = CARTESIAN_POINT ( 'NONE',  ( -10.00000000000000000, 0.000000000000000000, 0.000000000000000000 ) ) ;
#19078 = DIRECTION ( 'NONE',  ( -1.000000000000000000, 0.000000000000000000, -0.000000000000000000 ) ) ;
#19079 = EDGE_LOOP ( 'NONE', ( #17241, #8596, #4426, #41976 ) ) ;
#19080 = CARTESIAN_POINT ( 'NONE',  ( 16.14498194198480618, 40.00000000000000000, 21.03343489346954698 ) ) ;
#19081 = STYLED_ITEM ( 'NONE', ( #16484 ), #11465 ) ;
#19082 = EDGE_CURVE ( 'NONE', #41484, #40947, #8284, .T. ) ;
#19083 = CARTESIAN_POINT ( 'NONE',  ( -42.09738266246711902, 40.00000000000000000, -2.828681863544772135 ) ) ;
#19084 = CIRCLE ( 'NONE', #9972, 36.00000000000000000 ) ;
#19085 = ORIENTED_EDGE ( 'NONE', *, *, #988, .F. ) ;
#19086 = ORIENTED_EDGE ( 'NONE', *, *, #15428, .F. ) ;
#19087 = CYLINDRICAL_SURFACE ( 'NONE', #41568, 116.0000000000000000 ) ;
#19088 = DIRECTION ( 'NONE',  ( 0.000000000000000000, 0.3641605752528230266, -0.9313361774523382097 ) ) ;
#19089 = CARTESIAN_POINT ( 'NONE',  ( 20.55500000000001748, 0.000000000000000000, 0.000000000000000000 ) ) ;
#19090 = CYLINDRICAL_SURFACE ( 'NONE', #26819, 116.0000000000000000 ) ;
#19091 = EDGE_CURVE ( 'NONE', #20435, #3075, #8174, .T. ) ;
#19092 = EDGE_CURVE ( 'NONE', #3822, #18385, #4892, .T. ) ;
#19093 = DIRECTION ( 'NONE',  ( 0.000000000000000000, -0.5528000653611833126, -0.8333139190825217257 ) ) ;
#19094 = VERTEX_POINT ( 'NONE', #4227 ) ;
#19095 = CARTESIAN_POINT ( 'NONE',  ( 17.99999999999999645, 0.000000000000000000, 0.000000000000000000 ) ) ;
#19096 = ORIENTED_EDGE ( 'NONE', *, *, #2501, .T. ) ;
#19097 = DIRECTION ( 'NONE',  ( 0.000000000000000000, 0.000000000000000000, 1.000000000000000000 ) ) ;
#19098 = DIRECTION ( 'NONE',  ( -1.000000000000000000, -0.000000000000000000, -0.000000000000000000 ) ) ;
#19099 = EDGE_CURVE ( 'NONE', #1834, #40651, #6182, .T. ) ;
#19100 = CARTESIAN_POINT ( 'NONE',  ( 17.99999999999999645, 83.49789599728902090, -86.88263557826680028 ) ) ;
#19101 = AXIS2_PLACEMENT_3D ( 'NONE', #38716, #26078, #28928 ) ;
#19102 = CARTESIAN_POINT ( 'NONE',  ( 17.99999999999999645, 16.77727049691110750, 27.19001440037552086 ) ) ;
#19103 = EDGE_CURVE ( 'NONE', #9794, #26508, #21093, .T. ) ;
#19104 = ORIENTED_EDGE ( 'NONE', *, *, #26522, .F. ) ;
#19105 = CARTESIAN_POINT ( 'NONE',  ( -29.64342647699677613, 40.00000000000000000, -87.27882330658468391 ) ) ;
#19106 = ORIENTED_EDGE ( 'NONE', *, *, #3995, .F. ) ;
#19107 = CARTESIAN_POINT ( 'NONE',  ( 9.000000000000001776, 0.6505223195690489346, -51.99593080916757515 ) ) ;
#19108 = CIRCLE ( 'NONE', #22593, 58.99999999999999289 ) ;
#19109 = VERTEX_POINT ( 'NONE', #18464 ) ;
#19111 = ORIENTED_EDGE ( 'NONE', *, *, #40881, .T. ) ;
#19110 = DIRECTION ( 'NONE',  ( 0.000000000000000000, 0.8993121301712202476, -0.4373073204588531770 ) ) ;
#19112 = CARTESIAN_POINT ( 'NONE',  ( -39.97893566998936166, 31.00000000000000355, -35.18630237794885574 ) ) ;
#19113 = VERTEX_POINT ( 'NONE', #34342 ) ;
#19114 = CARTESIAN_POINT ( 'NONE',  ( 17.99999999999999645, -88.00363688980601751, 82.31555682352626491 ) ) ;
#19115 = FACE_BOUND ( 'NONE', #22713, .T. ) ;
#19116 = ORIENTED_EDGE ( 'NONE', *, *, #24304, .T. ) ;
#19118 = CARTESIAN_POINT ( 'NONE',  ( 73.52353481979008620, 39.99999999999999289, 25.08131146963209090 ) ) ;
#19117 = CIRCLE ( 'NONE', #23281, 20.00000000000000711 ) ;
#19119 = EDGE_CURVE ( 'NONE', #1487, #5158, #23635, .T. ) ;
#19121 = CARTESIAN_POINT ( 'NONE',  ( 1.039096088315723056E-14, -6.912265343809663812E-14, -26.00000000000000355 ) ) ;
#19120 = CYLINDRICAL_SURFACE ( 'NONE', #34933, 59.00000000000000000 ) ;
#19122 = ADVANCED_FACE ( 'NONE', ( #38265 ), #25726, .T. ) ;
#19123 = DIRECTION ( 'NONE',  ( 0.000000000000000000, -2.128711519673234442E-14, -1.000000000000000000 ) ) ;
#19124 = ORIENTED_EDGE ( 'NONE', *, *, #18319, .T. ) ;
#19125 = DIRECTION ( 'NONE',  ( -1.000000000000000000, -0.000000000000000000, 0.000000000000000000 ) ) ;
#19126 = AXIS2_PLACEMENT_3D ( 'NONE', #14256, #242, #13615 ) ;
#19127 = VERTEX_POINT ( 'NONE', #8379 ) ;
#19128 = DIRECTION ( 'NONE',  ( -3.996523416598930318E-16, 2.658563593772947863E-15, 1.000000000000000000 ) ) ;
#19129 = DIRECTION ( 'NONE',  ( -1.000000000000000000, 3.469446951953614189E-17, 0.000000000000000000 ) ) ;
#19130 = CARTESIAN_POINT ( 'NONE',  ( -21.91107887650263564, 31.00000000000000355, 64.54935342160338507 ) ) ;
#19132 = CARTESIAN_POINT ( 'NONE',  ( 0.000000000000000000, 0.000000000000000000, 0.000000000000000000 ) ) ;
#19131 = DIRECTION ( 'NONE',  ( -1.000000000000000000, -0.000000000000000000, -0.000000000000000000 ) ) ;
#19133 = EDGE_CURVE ( 'NONE', #21485, #16671, #6914, .T. ) ;
#19134 = ORIENTED_EDGE ( 'NONE', *, *, #15135, .T. ) ;
#19135 = AXIS2_PLACEMENT_3D ( 'NONE', #14179, #20524, #13755 ) ;
#19136 = AXIS2_PLACEMENT_3D ( 'NONE', #2972, #39004, #32259 ) ;
#19137 = ORIENTED_EDGE ( 'NONE', *, *, #5296, .T. ) ;
#19138 = CYLINDRICAL_SURFACE ( 'NONE', #8936, 47.49900000000000233 ) ;
#19139 = LINE ( 'NONE', #29158, #4625 ) ;
#19140 = CARTESIAN_POINT ( 'NONE',  ( 30.72743980831337751, 31.00000000000000355, -90.12673907452091271 ) ) ;
#19141 = CARTESIAN_POINT ( 'NONE',  ( 97.09201668843398636, 39.99999999999999289, 6.474068422258194566 ) ) ;
#19142 = DIRECTION ( 'NONE',  ( 0.000000000000000000, -0.2486898871648622888, 0.9685831611286290777 ) ) ;
#19143 = AXIS2_PLACEMENT_3D ( 'NONE', #21228, #17314, #10717 ) ;
#19144 = EDGE_CURVE ( 'NONE', #1445, #12660, #40992, .T. ) ;
#19145 = VERTEX_POINT ( 'NONE', #21311 ) ;
#19146 = CARTESIAN_POINT ( 'NONE',  ( 2.344047193898588954, 3.265465875126468021, -5.031375706690542042E-16 ) ) ;
#19147 = VERTEX_POINT ( 'NONE', #34560 ) ;
#19148 = PRESENTATION_LAYER_ASSIGNMENT (  '', '', ( #37909 ) ) ;
#19149 = DIRECTION ( 'NONE',  ( 0.000000000000000000, 0.000000000000000000, 1.000000000000000000 ) ) ;
#19150 = EDGE_CURVE ( 'NONE', #637, #20538, #30591, .T. ) ;
#19151 = DIRECTION ( 'NONE',  ( 0.000000000000000000, -0.9407002666710364558, 0.3392388661180213427 ) ) ;
#19152 = DIRECTION ( 'NONE',  ( 0.000000000000000000, 0.000000000000000000, -1.000000000000000000 ) ) ;
#19153 = EDGE_LOOP ( 'NONE', ( #5556, #39010, #33210, #22750 ) ) ;
#19154 = CARTESIAN_POINT ( 'NONE',  ( 17.99999999999999645, 0.000000000000000000, 0.000000000000000000 ) ) ;
#19155 = CYLINDRICAL_SURFACE ( 'NONE', #42370, 59.00000000000000000 ) ;
#19156 = CARTESIAN_POINT ( 'NONE',  ( 106.4195705685756792, -106.4195705685758213, 9.999999999999669598 ) ) ;
#19157 = CIRCLE ( 'NONE', #30247, 36.00000000000000000 ) ;
#19158 = ORIENTED_EDGE ( 'NONE', *, *, #18961, .T. ) ;
#19159 = CARTESIAN_POINT ( 'NONE',  ( 26.53203760875093309, 31.00000000000000355, 7.134992448514335450 ) ) ;
#19160 = EDGE_CURVE ( 'NONE', #11466, #7939, #31989, .T. ) ;
#19161 = CARTESIAN_POINT ( 'NONE',  ( 0.000000000000000000, 24.72041153920732981, 40.55929306992697292 ) ) ;
#19162 = AXIS2_PLACEMENT_3D ( 'NONE', #36144, #6465, #19188 ) ;
#19164 = EDGE_LOOP ( 'NONE', ( #19225, #10973, #38895, #11 ) ) ;
#19163 = DIRECTION ( 'NONE',  ( 0.000000000000000000, 0.000000000000000000, 1.000000000000000000 ) ) ;
#19165 = VECTOR ( 'NONE', #30283, 1000.000000000000000 ) ;
#19166 = ORIENTED_EDGE ( 'NONE', *, *, #37415, .F. ) ;
#19167 = DIRECTION ( 'NONE',  ( 0.000000000000000000, -0.1590634960190789038, 0.9872683547213435551 ) ) ;
#19168 = DIRECTION ( 'NONE',  ( -1.000000000000000000, -0.000000000000000000, -0.000000000000000000 ) ) ;
#19169 = CARTESIAN_POINT ( 'NONE',  ( 47.09643503918425012, 40.00000000000000000, 3.164684800459844904 ) ) ;
#19170 = DIRECTION ( 'NONE',  ( -1.000000000000000000, -0.000000000000000000, -0.000000000000000000 ) ) ;
#19171 = EDGE_CURVE ( 'NONE', #14175, #9120, #31964, .T. ) ;
#19172 = EDGE_CURVE ( 'NONE', #27946, #8111, #4078, .T. ) ;
#19173 = DIRECTION ( 'NONE',  ( 0.000000000000000000, 0.000000000000000000, 1.000000000000000000 ) ) ;
#19174 = ADVANCED_FACE ( 'NONE', ( #19308 ), #5540, .F. ) ;
#19175 = ADVANCED_FACE ( 'NONE', ( #16234 ), #15808, .T. ) ;
#19176 = DIRECTION ( 'NONE',  ( -1.000000000000000000, 0.000000000000000000, 0.000000000000000000 ) ) ;
#19177 = ORIENTED_EDGE ( 'NONE', *, *, #40167, .T. ) ;
#19178 = ORIENTED_EDGE ( 'NONE', *, *, #9055, .T. ) ;
#19179 = CARTESIAN_POINT ( 'NONE',  ( -1.312671235360383548, -3.860931062424228788, -0.05923475698271369466 ) ) ;
#19180 = AXIS2_PLACEMENT_3D ( 'NONE', #715, #3759, #33901 ) ;
#19181 = ORIENTED_EDGE ( 'NONE', *, *, #8687, .F. ) ;
#19182 = CARTESIAN_POINT ( 'NONE',  ( 0.000000000000000000, 94.83915810436401728, 59.94836581341619564 ) ) ;
#19183 = CARTESIAN_POINT ( 'NONE',  ( -4.154094228333736538, -2.398367420967545627, -3.721909803043222276 ) ) ;
#19184 = CARTESIAN_POINT ( 'NONE',  ( -38.31599561464027914, 31.00000000000000355, 10.26995502114586678 ) ) ;
#19185 = CARTESIAN_POINT ( 'NONE',  ( 17.99999999999999645, 106.5605152861910909, -56.26142179985714620 ) ) ;
#19186 = ORIENTED_EDGE ( 'NONE', *, *, #32934, .F. ) ;
#19187 = AXIS2_PLACEMENT_3D ( 'NONE', #5605, #5399, #18763 ) ;
#19188 = DIRECTION ( 'NONE',  ( 1.000000000000000000, -3.035766082959414264E-17, 0.000000000000000000 ) ) ;
#19189 = CARTESIAN_POINT ( 'NONE',  ( -12.08748825390017068, 31.00000000000000355, -91.69541640458645304 ) ) ;
#19190 = VECTOR ( 'NONE', #18894, 1000.000000000000000 ) ;
#19191 = DIRECTION ( 'NONE',  ( 1.000000000000000000, 0.000000000000000000, 0.000000000000000000 ) ) ;
#19192 = ORIENTED_EDGE ( 'NONE', *, *, #35251, .F. ) ;
#19193 = CARTESIAN_POINT ( 'NONE',  ( 40.05902963217418744, 31.00000000000000355, -52.04757428483648596 ) ) ;
#19195 = AXIS2_PLACEMENT_3D ( 'NONE', #26771, #33959, #10620 ) ;
#19194 = CARTESIAN_POINT ( 'NONE',  ( 58.81396797841472335, 40.00000000000000000, 34.08301911901634895 ) ) ;
#19196 = CARTESIAN_POINT ( 'NONE',  ( 83.17098260925966713, 39.99999999999999289, 48.02127090943169208 ) ) ;
#19197 = CIRCLE ( 'NONE', #42832, 120.5010000000000190 ) ;
#19198 = VERTEX_POINT ( 'NONE', #5949 ) ;
#19199 = DIRECTION ( 'NONE',  ( -1.000000000000000000, -0.000000000000000000, -0.000000000000000000 ) ) ;
#19200 = DIRECTION ( 'NONE',  ( 0.000000000000000000, 0.000000000000000000, 1.000000000000000000 ) ) ;
#19201 = DIRECTION ( 'NONE',  ( 0.000000000000000000, 0.000000000000000000, 1.000000000000000000 ) ) ;
#19203 = VERTEX_POINT ( 'NONE', #32154 ) ;
#19202 = FACE_OUTER_BOUND ( 'NONE', #38329, .T. ) ;
#19204 = DIRECTION ( 'NONE',  ( -1.000000000000000000, 0.000000000000000000, 0.000000000000000000 ) ) ;
#19205 = DIRECTION ( 'NONE',  ( -1.000000000000000000, 0.000000000000000000, -0.000000000000000000 ) ) ;
#19206 = AXIS2_PLACEMENT_3D ( 'NONE', #1376, #5082, #14725 ) ;
#19207 = ORIENTED_EDGE ( 'NONE', *, *, #10225, .F. ) ;
#19208 = CARTESIAN_POINT ( 'NONE',  ( -79.27599250299880396, 40.00000000000000711, 10.45126230984107707 ) ) ;
#19209 = CYLINDRICAL_SURFACE ( 'NONE', #34025, 36.00000000000000000 ) ;
#19210 = EDGE_LOOP ( 'NONE', ( #7620, #21253, #1878, #18909 ) ) ;
#19211 = FACE_OUTER_BOUND ( 'NONE', #39396, .T. ) ;
#19212 = CIRCLE ( 'NONE', #329, 16.00000000000023448 ) ;
#19213 = ORIENTED_EDGE ( 'NONE', *, *, #14735, .T. ) ;
#19214 = CIRCLE ( 'NONE', #1727, 31.49900000000000233 ) ;
#19215 = ORIENTED_EDGE ( 'NONE', *, *, #30000, .T. ) ;
#19216 = DIRECTION ( 'NONE',  ( -1.000000000000000000, 0.000000000000000000, 0.000000000000000000 ) ) ;
#19217 = ORIENTED_EDGE ( 'NONE', *, *, #11419, .F. ) ;
#19218 = DIRECTION ( 'NONE',  ( 0.000000000000000000, -0.1253332335642905471, -0.9921147013144795412 ) ) ;
#19219 = DIRECTION ( 'NONE',  ( -1.000000000000000000, 0.000000000000000000, 0.000000000000000000 ) ) ;
#19220 = CIRCLE ( 'NONE', #3107, 120.5010000000000474 ) ;
#19221 = DIRECTION ( 'NONE',  ( -3.009274222672345096E-17, -1.000000000000000000, 2.455023325076454960E-18 ) ) ;
#19222 = EDGE_CURVE ( 'NONE', #25155, #5697, #9679, .T. ) ;
#19223 = ADVANCED_FACE ( 'NONE', ( #12105 ), #42387, .F. ) ;
#19224 = CARTESIAN_POINT ( 'NONE',  ( 18.00000000000000355, 0.000000000000000000, 0.000000000000000000 ) ) ;
#19225 = ORIENTED_EDGE ( 'NONE', *, *, #16824, .T. ) ;
#19226 = CARTESIAN_POINT ( 'NONE',  ( -132.0000507999999968, 0.000000000000000000, 0.000000000000000000 ) ) ;
#19227 = EDGE_CURVE ( 'NONE', #15182, #21901, #34752, .T. ) ;
#19229 = VERTEX_POINT ( 'NONE', #19520 ) ;
#19228 = CIRCLE ( 'NONE', #1046, 36.00000000000000000 ) ;
#19230 = CYLINDRICAL_SURFACE ( 'NONE', #9902, 120.5010000000000190 ) ;
#19231 = ORIENTED_EDGE ( 'NONE', *, *, #34366, .T. ) ;
#19232 = LINE ( 'NONE', #12663, #4326 ) ;
#19233 = CYLINDRICAL_SURFACE ( 'NONE', #20976, 59.00000000000000000 ) ;
#19234 = CARTESIAN_POINT ( 'NONE',  ( 4.000000000000003553, -2.309401076758513138, -3.504271511726786859 ) ) ;
#19235 = CARTESIAN_POINT ( 'NONE',  ( 61.18335543008118549, 31.00000000000000000, -20.78249587198964576 ) ) ;
#19236 = CARTESIAN_POINT ( 'NONE',  ( 17.99999999999999645, -46.83041522348565167, 101.9567785075599744 ) ) ;
#19237 = EDGE_CURVE ( 'NONE', #21205, #2350, #8586, .T. ) ;
#19239 = ORIENTED_EDGE ( 'NONE', *, *, #34295, .T. ) ;
#19238 = VECTOR ( 'NONE', #15616, 1000.000000000000000 ) ;
#19240 = CARTESIAN_POINT ( 'NONE',  ( -31.36635120280995537, 31.00000000000000355, -8.451140850656344128 ) ) ;
#19241 = CARTESIAN_POINT ( 'NONE',  ( 59.08215048199704711, 39.99999999999999289, 29.12166076727282515 ) ) ;
#19242 = AXIS2_PLACEMENT_3D ( 'NONE', #11158, #4810, #17302 ) ;
#19243 = AXIS2_PLACEMENT_3D ( 'NONE', #4156, #37761, #20812 ) ;
#19244 =( GEOMETRIC_REPRESENTATION_CONTEXT ( 3 ) GLOBAL_UNCERTAINTY_ASSIGNED_CONTEXT ( ( #32651 ) ) GLOBAL_UNIT_ASSIGNED_CONTEXT ( ( #3756, #40857, #33899 ) ) REPRESENTATION_CONTEXT ( 'NONE', 'WORKASPACE' ) );
#19245 = DIRECTION ( 'NONE',  ( 0.000000000000000000, 0.000000000000000000, 1.000000000000000000 ) ) ;
#19246 = CARTESIAN_POINT ( 'NONE',  ( -105.9879088449591933, 17.11489954122026447, -0.3807199291576673361 ) ) ;
#19247 = VECTOR ( 'NONE', #4432, 1000.000000000000000 ) ;
#19248 = AXIS2_PLACEMENT_3D ( 'NONE', #12787, #26317, #36104 ) ;
#19249 = CARTESIAN_POINT ( 'NONE',  ( 17.99999999999999645, 0.000000000000000000, 0.000000000000000000 ) ) ;
#19250 = DIRECTION ( 'NONE',  ( 0.000000000000000000, 0.9822872507286892763, -0.1873813145857214368 ) ) ;
#19251 = CIRCLE ( 'NONE', #383, 13.60000000000000142 ) ;
#19252 = ORIENTED_EDGE ( 'NONE', *, *, #27788, .T. ) ;
#19253 = CARTESIAN_POINT ( 'NONE',  ( 6.197074855318628117, 40.00000000000000000, 46.98549035852928313 ) ) ;
#19254 = DIRECTION ( 'NONE',  ( -1.000000000000000000, -0.000000000000000000, -0.000000000000000000 ) ) ;
#19255 = FACE_OUTER_BOUND ( 'NONE', #36705, .T. ) ;
#19256 = ORIENTED_EDGE ( 'NONE', *, *, #33658, .T. ) ;
#19257 = CARTESIAN_POINT ( 'NONE',  ( 18.00000000000000355, 46.87740477351718482, 16.82754413119463166 ) ) ;
#19258 = DIRECTION ( 'NONE',  ( 1.000000000000000000, 0.000000000000000000, -0.000000000000000000 ) ) ;
#19259 = EDGE_LOOP ( 'NONE', ( #17283, #21923 ) ) ;
#19260 = DIRECTION ( 'NONE',  ( -1.000000000000000000, 0.000000000000000000, -0.000000000000000000 ) ) ;
#19261 = VERTEX_POINT ( 'NONE', #18695 ) ;
#19262 = ORIENTED_EDGE ( 'NONE', *, *, #28638, .F. ) ;
#19263 = LINE ( 'NONE', #18649, #13963 ) ;
#19264 = CARTESIAN_POINT ( 'NONE',  ( 42.86165537668586722, 31.00000000000000355, -73.99543480067944756 ) ) ;
#19265 = ORIENTED_EDGE ( 'NONE', *, *, #3285, .F. ) ;
#19266 = DIRECTION ( 'NONE',  ( -1.000000000000000000, -0.000000000000000000, -0.000000000000000000 ) ) ;
#19267 = CIRCLE ( 'NONE', #24827, 13.60000000000000142 ) ;
#19268 = EDGE_CURVE ( 'NONE', #12118, #27792, #13877, .T. ) ;
#19270 = DIRECTION ( 'NONE',  ( 0.000000000000000000, 0.9213119778704113028, 0.3888241754733244848 ) ) ;
#19269 = CIRCLE ( 'NONE', #12281, 2.799122904894268071 ) ;
#19271 = VERTEX_POINT ( 'NONE', #15395 ) ;
#19272 = CIRCLE ( 'NONE', #9456, 31.49899999999999878 ) ;
#19273 = CARTESIAN_POINT ( 'NONE',  ( 18.00000000000000355, 0.000000000000000000, 0.000000000000000000 ) ) ;
#19274 = CARTESIAN_POINT ( 'NONE',  ( -96.33078216555149709, 40.00000000000000711, 32.58251675340183340 ) ) ;
#19275 = DIRECTION ( 'NONE',  ( -3.009274222672345096E-17, -1.000000000000000000, 2.455023325076454960E-18 ) ) ;
#19277 = FACE_OUTER_BOUND ( 'NONE', #22692, .T. ) ;
#19276 = CARTESIAN_POINT ( 'NONE',  ( 18.00000000000000355, 0.000000000000000000, 0.000000000000000000 ) ) ;
#19278 = AXIS2_PLACEMENT_3D ( 'NONE', #36152, #42690, #39421 ) ;
#19279 = EDGE_CURVE ( 'NONE', #41990, #28580, #38683, .T. ) ;
#19280 = CIRCLE ( 'NONE', #41539, 13.60000000000000142 ) ;
#19281 = CYLINDRICAL_SURFACE ( 'NONE', #37454, 59.00000000000000000 ) ;
#19282 = ORIENTED_EDGE ( 'NONE', *, *, #29664, .F. ) ;
#19283 = EDGE_CURVE ( 'NONE', #1575, #20648, #8810, .T. ) ;
#19284 =( NAMED_UNIT ( * ) PLANE_ANGLE_UNIT ( ) SI_UNIT ( $, .RADIAN. ) );
#19285 = CARTESIAN_POINT ( 'NONE',  ( 24.21999397792122366, 31.00000000000000355, 8.216913396989165008 ) ) ;
#19286 = VERTEX_POINT ( 'NONE', #22168 ) ;
#19287 = DIRECTION ( 'NONE',  ( 0.000000000000000000, 0.000000000000000000, 1.000000000000000000 ) ) ;
#19288 = EDGE_CURVE ( 'NONE', #26320, #21350, #43075, .T. ) ;
#19289 = CARTESIAN_POINT ( 'NONE',  ( 17.99999999999999645, -118.8387007424469601, -19.94628303336605768 ) ) ;
#19290 = VERTEX_POINT ( 'NONE', #9234 ) ;
#19291 = CARTESIAN_POINT ( 'NONE',  ( 34.56606645648713538, 40.00000000000000000, -4.560848911255810378 ) ) ;
#19292 = CARTESIAN_POINT ( 'NONE',  ( 28.69597684714337049, 40.00000000000000000, 25.25520295781286251 ) ) ;
#19293 = ORIENTED_EDGE ( 'NONE', *, *, #22832, .F. ) ;
#19294 = ORIENTED_EDGE ( 'NONE', *, *, #28816, .T. ) ;
#19295 = DIRECTION ( 'NONE',  ( -1.000000000000000000, -0.000000000000000000, 0.000000000000000000 ) ) ;
#19296 = FACE_OUTER_BOUND ( 'NONE', #7986, .T. ) ;
#19298 = SURFACE_SIDE_STYLE ('',( #43175 ) ) ;
#19297 = AXIS2_PLACEMENT_3D ( 'NONE', #13078, #8923, #22688 ) ;
#19299 = DIRECTION ( 'NONE',  ( 0.000000000000000000, -0.5076658003388292428, -0.8615540813938123987 ) ) ;
#19300 = VECTOR ( 'NONE', #8525, 1000.000000000000114 ) ;
#19301 = AXIS2_PLACEMENT_3D ( 'NONE', #21821, #38763, #15038 ) ;
#19302 = DIRECTION ( 'NONE',  ( -1.000000000000000000, -0.000000000000000000, -0.000000000000000000 ) ) ;
#19303 = CIRCLE ( 'NONE', #24162, 20.00000000000000000 ) ;
#19304 = CARTESIAN_POINT ( 'NONE',  ( 17.99999999999999645, -119.0898412705475522, 18.38751498043690802 ) ) ;
#19305 = ORIENTED_EDGE ( 'NONE', *, *, #25989, .T. ) ;
#19306 = DIRECTION ( 'NONE',  ( -1.000000000000000000, 0.000000000000000000, -0.000000000000000000 ) ) ;
#19307 = ORIENTED_EDGE ( 'NONE', *, *, #10869, .T. ) ;
#19308 = FACE_OUTER_BOUND ( 'NONE', #36238, .T. ) ;
#19309 = EDGE_CURVE ( 'NONE', #32279, #11569, #38914, .T. ) ;
#19310 = FACE_OUTER_BOUND ( 'NONE', #11352, .T. ) ;
#19311 = AXIS2_PLACEMENT_3D ( 'NONE', #32145, #11671, #2226 ) ;
#19312 = VECTOR ( 'NONE', #6647, 1000.000000000000114 ) ;
#19313 = DIRECTION ( 'NONE',  ( -1.000000000000000000, 0.000000000000000000, 0.000000000000000000 ) ) ;
#19314 = CYLINDRICAL_SURFACE ( 'NONE', #28289, 20.00000000000000711 ) ;
#19315 = EDGE_LOOP ( 'NONE', ( #42927, #29381, #778, #24500 ) ) ;
#19316 = CARTESIAN_POINT ( 'NONE',  ( 18.00000000000000355, 47.32430374665962347, -21.55018039121476647 ) ) ;
#19317 = ORIENTED_EDGE ( 'NONE', *, *, #6080, .F. ) ;
#19318 = DIRECTION ( 'NONE',  ( 0.000000000000000000, 0.4610925014493267859, -0.8873520750565710991 ) ) ;
#19319 = AXIS2_PLACEMENT_3D ( 'NONE', #20091, #25963, #16808 ) ;
#19320 = ORIENTED_EDGE ( 'NONE', *, *, #7900, .T. ) ;
#19322 = ORIENTED_EDGE ( 'NONE', *, *, #14682, .F. ) ;
#19321 = CARTESIAN_POINT ( 'NONE',  ( 6.075999999999997847, 0.000000000000000000, 0.000000000000000000 ) ) ;
#19323 = CIRCLE ( 'NONE', #453, 47.49900000000000233 ) ;
#19324 = CARTESIAN_POINT ( 'NONE',  ( -26.81486728382429519, 31.00000000000000355, -46.61672233255472975 ) ) ;
#19325 = EDGE_LOOP ( 'NONE', ( #36930, #15329 ) ) ;
#19326 = DIRECTION ( 'NONE',  ( -1.000000000000000000, 0.000000000000000000, -0.000000000000000000 ) ) ;
#19327 = ADVANCED_FACE ( 'NONE', ( #12320 ), #22800, .F. ) ;
#19328 = VERTEX_POINT ( 'NONE', #2443 ) ;
#19329 = DIRECTION ( 'NONE',  ( 0.000000000000000000, 0.9826841245925201918, 0.1852887240871181063 ) ) ;
#19330 = PRODUCT ( 'spur gear_iso_ISO - Spur gear 2M 50T 20PA 18FW ---S50B22H150L15.0N', 'spur gear_iso_ISO - Spur gear 2M 50T 20PA 18FW ---S50B22H150L15.0N', '', ( #32927 ) ) ;
#19331 = ORIENTED_EDGE ( 'NONE', *, *, #5368, .T. ) ;
#19332 = CARTESIAN_POINT ( 'NONE',  ( -31.21560191380782712, 40.00000000000000000, 63.07420938637471863 ) ) ;
#19334 = DIRECTION ( 'NONE',  ( 0.000000000000000000, -0.9510565162951565288, 0.3090169943749382919 ) ) ;
#19333 = DIRECTION ( 'NONE',  ( 0.000000000000000000, 0.000000000000000000, 1.000000000000000000 ) ) ;
#19335 = DIRECTION ( 'NONE',  ( 1.000000000000000000, 0.000000000000000000, 0.000000000000000000 ) ) ;
#19336 = ORIENTED_EDGE ( 'NONE', *, *, #13740, .F. ) ;
#19337 = DIRECTION ( 'NONE',  ( 0.000000000000000000, 0.000000000000000000, 1.000000000000000000 ) ) ;
#19338 = ORIENTED_EDGE ( 'NONE', *, *, #40546, .T. ) ;
#19339 = EDGE_CURVE ( 'NONE', #42086, #5899, #19460, .T. ) ;
#19340 = CIRCLE ( 'NONE', #1888, 2.649999999999957723 ) ;
#19341 = CARTESIAN_POINT ( 'NONE',  ( 0.000000000000000000, 120.3696465864706937, -5.624871700594833435 ) ) ;
#19342 = CARTESIAN_POINT ( 'NONE',  ( 17.99999999999999645, 0.000000000000000000, 0.000000000000000000 ) ) ;
#19343 = CIRCLE ( 'NONE', #18064, 47.49900000000000233 ) ;
#19344 = CARTESIAN_POINT ( 'NONE',  ( 64.36038921521112854, 31.00000000000000000, -37.17434371002195803 ) ) ;
#19346 = LINE ( 'NONE', #19768, #20702 ) ;
#19345 = FACE_BOUND ( 'NONE', #49, .T. ) ;
#19348 = EDGE_LOOP ( 'NONE', ( #33313, #10958, #8721, #13919 ) ) ;
#19347 = AXIS2_PLACEMENT_3D ( 'NONE', #36523, #12375, #19149 ) ;
#19349 = EDGE_CURVE ( 'NONE', #1677, #37721, #6380, .T. ) ;
#19350 = CIRCLE ( 'NONE', #5395, 13.59999999999999964 ) ;
#19351 = CIRCLE ( 'NONE', #38119, 116.0000000000000000 ) ;
#19352 = CIRCLE ( 'NONE', #10993, 116.0000000000000000 ) ;
#19353 = ORIENTED_EDGE ( 'NONE', *, *, #1222, .T. ) ;
#19354 = CARTESIAN_POINT ( 'NONE',  ( 17.99999999999999645, 23.87611429743662939, 20.54551452399628531 ) ) ;
#19355 = DIRECTION ( 'NONE',  ( 0.000000000000000000, 0.000000000000000000, 1.000000000000000000 ) ) ;
#19356 = CARTESIAN_POINT ( 'NONE',  ( -44.52253807734693680, 31.00000000000000355, 90.03212995789276363 ) ) ;
#19357 = CARTESIAN_POINT ( 'NONE',  ( 92.49871336443506209, 39.99999999999999289, 31.53380891771211125 ) ) ;
#19358 = DIRECTION ( 'NONE',  ( -1.000000000000000000, 0.000000000000000000, -0.000000000000000000 ) ) ;
#19359 = VERTEX_POINT ( 'NONE', #3721 ) ;
#19360 = CARTESIAN_POINT ( 'NONE',  ( 17.99999999999999645, -107.5680526044921947, 31.89649718262059608 ) ) ;
#19361 = ORIENTED_EDGE ( 'NONE', *, *, #41138, .F. ) ;
#19362 = EDGE_CURVE ( 'NONE', #31353, #30532, #22249, .T. ) ;
#19363 = DIRECTION ( 'NONE',  ( 1.000000000000000000, -0.000000000000000000, 0.000000000000000000 ) ) ;
#19364 = EDGE_CURVE ( 'NONE', #14757, #35069, #20152, .T. ) ;
#19365 = CIRCLE ( 'NONE', #1191, 20.00000000000000711 ) ;
#19366 = CARTESIAN_POINT ( 'NONE',  ( -4.121423858225412573, -12.61643262889541184, 0.000000000000000000 ) ) ;
#19367 = CARTESIAN_POINT ( 'NONE',  ( -106.4195705685756081, 106.4195705685752529, 9.999999999999998224 ) ) ;
#19368 = VERTEX_POINT ( 'NONE', #13606 ) ;
#19369 = FACE_BOUND ( 'NONE', #15720, .T. ) ;
#19370 = AXIS2_PLACEMENT_3D ( 'NONE', #16674, #1114, #4835 ) ;
#19371 = CARTESIAN_POINT ( 'NONE',  ( 0.000000000000000000, -69.72480978689985420, -92.70626138606085931 ) ) ;
#19372 = CIRCLE ( 'NONE', #29785, 59.00000000000000000 ) ;
#19373 = DIRECTION ( 'NONE',  ( 0.000000000000000000, -0.7705132427757817037, -0.6374239897486988493 ) ) ;
#19374 = AXIS2_PLACEMENT_3D ( 'NONE', #10714, #21016, #27309 ) ;
#19375 = AXIS2_PLACEMENT_3D ( 'NONE', #15862, #28537, #4944 ) ;
#19376 = AXIS2_PLACEMENT_3D ( 'NONE', #1837, #15198, #35213 ) ;
#19378 = VERTEX_POINT ( 'NONE', #33224 ) ;
#19377 = CARTESIAN_POINT ( 'NONE',  ( -103.7695705685756025, 106.4195705685752529, 9.999999999999998224 ) ) ;
#19379 = DIRECTION ( 'NONE',  ( 0.000000000000000000, -0.3140767120219556952, 0.9493976084683790617 ) ) ;
#19380 = DIRECTION ( 'NONE',  ( 0.000000000000000000, 0.000000000000000000, 1.000000000000000000 ) ) ;
#19381 = ADVANCED_FACE ( 'NONE', ( #10526 ), #9870, .F. ) ;
#19383 = VERTEX_POINT ( 'NONE', #17337 ) ;
#19382 = LINE ( 'NONE', #26337, #25191 ) ;
#19384 = VERTEX_POINT ( 'NONE', #36915 ) ;
#19385 = CARTESIAN_POINT ( 'NONE',  ( 3.239593890920906993, -13.56862304811759223, -1.199999999999999956 ) ) ;
#19386 = CARTESIAN_POINT ( 'NONE',  ( 0.000000000000000000, 0.000000000000000000, 0.000000000000000000 ) ) ;
#19387 = CARTESIAN_POINT ( 'NONE',  ( 36.21668514975058173, 40.00000000000000000, 31.87730689759005287 ) ) ;
#19388 = CYLINDRICAL_SURFACE ( 'NONE', #4131, 120.5010000000000190 ) ;
#19389 = CIRCLE ( 'NONE', #11721, 31.49899999999999523 ) ;
#19390 = DIRECTION ( 'NONE',  ( 0.000000000000000000, 0.000000000000000000, 1.000000000000000000 ) ) ;
#19391 = SHAPE_REPRESENTATION ( 'internal spur gear_iso_ISO - Internal spur gear 2M 118T 20PA 18FW ---S118S260OD 1.0AF', ( #13552 ), #9968 ) ;
#19392 = CARTESIAN_POINT ( 'NONE',  ( 12.55910585664918422, 0.7408941433508176022, -1.199999999999999956 ) ) ;
#19393 = VERTEX_POINT ( 'NONE', #26900 ) ;
#19394 = DIRECTION ( 'NONE',  ( 1.000000000000000000, 0.000000000000000000, 0.000000000000000000 ) ) ;
#19395 = VERTEX_POINT ( 'NONE', #40174 ) ;
#19396 = EDGE_CURVE ( 'NONE', #10739, #1839, #36857, .T. ) ;
#19397 = CARTESIAN_POINT ( 'NONE',  ( 17.99999999999999645, 66.49630760163600485, 90.36876423296011751 ) ) ;
#19398 = DIRECTION ( 'NONE',  ( 1.000000000000000000, 0.000000000000000000, 0.000000000000000000 ) ) ;
#19399 = EDGE_CURVE ( 'NONE', #40502, #19359, #16892, .T. ) ;
#19400 = CARTESIAN_POINT ( 'NONE',  ( 30.63689417572177831, 31.00000000000000355, 34.91779699477408627 ) ) ;
#19401 = CIRCLE ( 'NONE', #21506, 1.999999999999988010 ) ;
#19402 = DIRECTION ( 'NONE',  ( 0.000000000000000000, -0.6382441836448261574, 0.7698339834299012807 ) ) ;
#19403 = ORIENTED_EDGE ( 'NONE', *, *, #28676, .T. ) ;
#19404 = AXIS2_PLACEMENT_3D ( 'NONE', #2621, #15981, #29278 ) ;
#19405 = DIRECTION ( 'NONE',  ( -1.000000000000000000, 0.000000000000000000, 0.000000000000000000 ) ) ;
#19406 = CARTESIAN_POINT ( 'NONE',  ( -44.26264085333531995, 31.00000000000000711, 76.66224561662070869 ) ) ;
#19407 = AXIS2_PLACEMENT_3D ( 'NONE', #30659, #7728, #21091 ) ;
#19408 = CARTESIAN_POINT ( 'NONE',  ( 2.650000000000176215, -150.5000000000013642, 9.999999999999586109 ) ) ;
#19409 = ORIENTED_EDGE ( 'NONE', *, *, #21561, .F. ) ;
#19410 = CARTESIAN_POINT ( 'NONE',  ( 67.09393615762301977, 31.00000000000000000, 4.495243625008654043 ) ) ;
#19411 = CARTESIAN_POINT ( 'NONE',  ( -67.85934734800838442, 40.00000000000000711, 22.92939687791763248 ) ) ;
#19412 = CYLINDRICAL_SURFACE ( 'NONE', #35017, 2.649999999999971934 ) ;
#19413 = ORIENTED_EDGE ( 'NONE', *, *, #11420, .F. ) ;
#19414 = EDGE_CURVE ( 'NONE', #20981, #17808, #30174, .T. ) ;
#19415 = DIRECTION ( 'NONE',  ( 1.000000000000000000, 0.000000000000000000, 0.000000000000000000 ) ) ;
#19416 = DIRECTION ( 'NONE',  ( -1.000000000000000000, 0.000000000000000000, 0.000000000000000000 ) ) ;
#19417 = ADVANCED_FACE ( 'NONE', ( #39952 ), #10084, .F. ) ;
#19418 = AXIS2_PLACEMENT_3D ( 'NONE', #19981, #23462, #14272 ) ;
#19419 = EDGE_CURVE ( 'NONE', #23134, #9900, #26263, .T. ) ;
#19420 = EDGE_CURVE ( 'NONE', #26461, #8937, #232, .T. ) ;
#19422 = ORIENTED_EDGE ( 'NONE', *, *, #17077, .T. ) ;
#19421 = DIRECTION ( 'NONE',  ( -1.000000000000000000, 0.000000000000000000, 0.000000000000000000 ) ) ;
#19423 = CARTESIAN_POINT ( 'NONE',  ( 0.000000000000000000, -23.10276247328181398, 118.2656051737069021 ) ) ;
#19424 = DIRECTION ( 'NONE',  ( -1.000000000000000000, -0.000000000000000000, -0.000000000000000000 ) ) ;
#19425 = CARTESIAN_POINT ( 'NONE',  ( -18.69663849766352826, 40.00000000000000000, -69.77653669617104981 ) ) ;
#19426 = DIRECTION ( 'NONE',  ( 1.000000000000000000, -1.373900992973641868E-15, -6.546126324440886161E-16 ) ) ;
#19427 = ORIENTED_EDGE ( 'NONE', *, *, #37947, .T. ) ;
#19428 = CARTESIAN_POINT ( 'NONE',  ( -10.00000000000000000, 0.000000000000000000, 0.000000000000000000 ) ) ;
#19429 = AXIS2_PLACEMENT_3D ( 'NONE', #4392, #37349, #7470 ) ;
#19430 = DIRECTION ( 'NONE',  ( 1.000000000000000000, 1.836909530733573776E-16, 0.000000000000000000 ) ) ;
#19431 = VECTOR ( 'NONE', #10923, 1000.000000000000000 ) ;
#19432 = ORIENTED_EDGE ( 'NONE', *, *, #25527, .F. ) ;
#19433 = AXIS2_PLACEMENT_3D ( 'NONE', #42273, #25119, #25746 ) ;
#19434 = ORIENTED_EDGE ( 'NONE', *, *, #29652, .T. ) ;
#19435 = DIRECTION ( 'NONE',  ( -1.000000000000000000, 0.000000000000000000, 0.000000000000000000 ) ) ;
#19436 = VERTEX_POINT ( 'NONE', #23015 ) ;
#19437 = CIRCLE ( 'NONE', #29859, 116.0000000000000000 ) ;
#19438 = CARTESIAN_POINT ( 'NONE',  ( 8.999999999999998224, 111.2559044912524939, 32.83479428644713494 ) ) ;
#19439 = CARTESIAN_POINT ( 'NONE',  ( 0.000000000000000000, 25.61928775981044026, 45.25098998563485964 ) ) ;
#19440 = CARTESIAN_POINT ( 'NONE',  ( 17.99999999999999645, 97.89532456239497549, 54.81585448086229917 ) ) ;
#19441 = CYLINDRICAL_SURFACE ( 'NONE', #35941, 20.00000000000000355 ) ;
#19442 = EDGE_LOOP ( 'NONE', ( #22626, #31244 ) ) ;
#19443 = FACE_OUTER_BOUND ( 'NONE', #14648, .T. ) ;
#19444 = ORIENTED_EDGE ( 'NONE', *, *, #24910, .F. ) ;
#19445 = EDGE_CURVE ( 'NONE', #32816, #23373, #10396, .T. ) ;
#19446 = DIRECTION ( 'NONE',  ( 0.000000000000000000, 0.000000000000000000, 1.000000000000000000 ) ) ;
#19447 = ORIENTED_EDGE ( 'NONE', *, *, #18056, .F. ) ;
#19448 = DIRECTION ( 'NONE',  ( -1.000000000000000000, 0.000000000000000000, 0.000000000000000000 ) ) ;
#19449 = EDGE_CURVE ( 'NONE', #6140, #19619, #43026, .T. ) ;
#19450 = DIRECTION ( 'NONE',  ( 0.000000000000000000, 2.305124076552231752E-14, -1.000000000000000000 ) ) ;
#19451 = APPLICATION_PROTOCOL_DEFINITION ( 'draft international standard', 'automotive_design', 1998, #33984 ) ;
#19452 = CARTESIAN_POINT ( 'NONE',  ( 17.99999999999999645, -110.3490479609630910, -20.28201389785511211 ) ) ;
#19453 = CARTESIAN_POINT ( 'NONE',  ( 16.30650823456882748, 31.00000000000000355, -60.90571087954511142 ) ) ;
#19454 = CARTESIAN_POINT ( 'NONE',  ( 18.00000000000000355, 22.82995208772688756, 41.06517797613672371 ) ) ;
#19455 = CIRCLE ( 'NONE', #11791, 65.00000000000000000 ) ;
#19456 = ORIENTED_EDGE ( 'NONE', *, *, #7317, .F. ) ;
#19457 = AXIS2_PLACEMENT_3D ( 'NONE', #2142, #35526, #5644 ) ;
#19458 = CARTESIAN_POINT ( 'NONE',  ( 33.88265278290064941, 31.00000000000000355, 16.77599488388065652 ) ) ;
#19459 = CARTESIAN_POINT ( 'NONE',  ( 52.51402048354923835, 40.00000000000000000, 40.27907379435107060 ) ) ;
#19460 = CIRCLE ( 'NONE', #11069, 1.000000000000000444 ) ;
#19461 = CARTESIAN_POINT ( 'NONE',  ( 17.99999999999999645, 30.78424799127067502, 6.672111855473287001 ) ) ;
#19462 = CARTESIAN_POINT ( 'NONE',  ( -31.74999999999995737, 0.000000000000000000, 2.500000000000000444 ) ) ;
#19463 = ADVANCED_FACE ( 'NONE', ( #6817 ), #9669, .T. ) ;
#19464 = EDGE_CURVE ( 'NONE', #17146, #17054, #2032, .T. ) ;
#19465 = DIRECTION ( 'NONE',  ( -3.996523416598930318E-16, 2.658563593772947863E-15, 1.000000000000000000 ) ) ;
#19466 = DIRECTION ( 'NONE',  ( -1.000000000000000000, 0.000000000000000000, 0.000000000000000000 ) ) ;
#19467 = EDGE_CURVE ( 'NONE', #15523, #36745, #19730, .T. ) ;
#19468 = ORIENTED_EDGE ( 'NONE', *, *, #2722, .T. ) ;
#19469 = CARTESIAN_POINT ( 'NONE',  ( 36.61186797162192619, 40.00000000000000000, 28.07927795628900469 ) ) ;
#19470 = DIRECTION ( 'NONE',  ( 1.000000000000000000, 0.000000000000000000, 0.000000000000000000 ) ) ;
#19471 = CARTESIAN_POINT ( 'NONE',  ( 0.000000000000000000, 120.2856157092987957, -7.201503623195590009 ) ) ;
#19472 = ORIENTED_EDGE ( 'NONE', *, *, #2560, .T. ) ;
#19473 = CYLINDRICAL_SURFACE ( 'NONE', #34957, 116.0000000000000000 ) ;
#19474 = CARTESIAN_POINT ( 'NONE',  ( 17.99999999999999645, -103.5682682299985515, -43.14958040911633219 ) ) ;
#19475 = VERTEX_POINT ( 'NONE', #6589 ) ;
#19476 = DIRECTION ( 'NONE',  ( 0.000000000000000000, 0.000000000000000000, -1.000000000000000000 ) ) ;
#19477 = ORIENTED_EDGE ( 'NONE', *, *, #18395, .T. ) ;
#19478 = ORIENTED_EDGE ( 'NONE', *, *, #42316, .T. ) ;
#19479 = CARTESIAN_POINT ( 'NONE',  ( 17.99999999999999645, 0.000000000000000000, 0.000000000000000000 ) ) ;
#19480 = ADVANCED_FACE ( 'NONE', ( #19951 ), #11192, .T. ) ;
#19481 = CARTESIAN_POINT ( 'NONE',  ( 58.37089435908782065, 31.00000000000000000, -75.89027429297952665 ) ) ;
#19482 = EDGE_LOOP ( 'NONE', ( #11345, #19320, #22058, #8652 ) ) ;
#19483 = CARTESIAN_POINT ( 'NONE',  ( -4.000000000000000000, -2.512220745329312610, -3.469390707569719901 ) ) ;
#19484 = AXIS2_PLACEMENT_3D ( 'NONE', #24632, #10866, #40719 ) ;
#19485 = FACE_OUTER_BOUND ( 'NONE', #16789, .T. ) ;
#19486 = CARTESIAN_POINT ( 'NONE',  ( 17.99999999999999645, 0.000000000000000000, 0.000000000000000000 ) ) ;
#19487 = CIRCLE ( 'NONE', #25086, 120.5010000000000616 ) ;
#19488 = ORIENTED_EDGE ( 'NONE', *, *, #25003, .F. ) ;
#19489 = DIRECTION ( 'NONE',  ( 0.000000000000000000, 0.000000000000000000, 1.000000000000000000 ) ) ;
#19490 = DIRECTION ( 'NONE',  ( -1.000000000000000000, -0.000000000000000000, 0.000000000000000000 ) ) ;
#19491 = DIRECTION ( 'NONE',  ( 0.000000000000000000, 0.000000000000000000, 1.000000000000000000 ) ) ;
#19493 = FACE_OUTER_BOUND ( 'NONE', #40884, .T. ) ;
#19492 = FACE_OUTER_BOUND ( 'NONE', #26792, .T. ) ;
#19494 = EDGE_CURVE ( 'NONE', #35521, #25103, #27139, .T. ) ;
#19495 = DIRECTION ( 'NONE',  ( 0.000000000000000000, 0.000000000000000000, 1.000000000000000000 ) ) ;
#19496 = ORIENTED_EDGE ( 'NONE', *, *, #38450, .F. ) ;
#19497 =( NAMED_UNIT ( * ) SI_UNIT ( $, .STERADIAN. ) SOLID_ANGLE_UNIT ( ) );
#19498 = CARTESIAN_POINT ( 'NONE',  ( 16.14498194198480618, 31.00000000000000355, 21.03343489346954698 ) ) ;
#19499 = ORIENTED_EDGE ( 'NONE', *, *, #39345, .T. ) ;
#19500 = DIRECTION ( 'NONE',  ( 0.000000000000000000, 0.9510565162951523099, 0.3090169943749515591 ) ) ;
#19501 = CARTESIAN_POINT ( 'NONE',  ( 0.000000000000000000, -116.4607004671426438, -30.94182036827324112 ) ) ;
#19502 = ORIENTED_EDGE ( 'NONE', *, *, #8593, .T. ) ;
#19503 = DIRECTION ( 'NONE',  ( 0.000000000000000000, 0.000000000000000000, -1.000000000000000000 ) ) ;
#19504 = CARTESIAN_POINT ( 'NONE',  ( -32.63632984357925437, 40.00000000000000000, -25.02932899672474676 ) ) ;
#19505 = CARTESIAN_POINT ( 'NONE',  ( -14.91913624998189825, 40.00000000000000000, -30.37684071747814230 ) ) ;
#19506 = CIRCLE ( 'NONE', #16809, 20.00000000000001066 ) ;
#19507 = ORIENTED_EDGE ( 'NONE', *, *, #9038, .F. ) ;
#19508 = ORIENTED_EDGE ( 'NONE', *, *, #25211, .T. ) ;
#19509 = FACE_OUTER_BOUND ( 'NONE', #28644, .T. ) ;
#19510 = CARTESIAN_POINT ( 'NONE',  ( 0.000000000000000000, 0.000000000000000000, 0.000000000000000000 ) ) ;
#19511 = AXIS2_PLACEMENT_3D ( 'NONE', #39547, #9032, #9682 ) ;
#19512 = EDGE_CURVE ( 'NONE', #6774, #36535, #19487, .T. ) ;
#19513 = CARTESIAN_POINT ( 'NONE',  ( 17.99999999999999645, -88.00363688980601751, 82.31555682352626491 ) ) ;
#19514 = CIRCLE ( 'NONE', #16020, 0.5155456020628804703 ) ;
#19515 = CARTESIAN_POINT ( 'NONE',  ( -17.77999999999999758, 1.347111479062088405E-15, -11.00000000000000000 ) ) ;
#19516 = DIRECTION ( 'NONE',  ( 0.000000000000000000, -0.5528000653611833126, -0.8333139190825217257 ) ) ;
#19517 = ORIENTED_EDGE ( 'NONE', *, *, #33327, .T. ) ;
#19518 = CARTESIAN_POINT ( 'NONE',  ( 2.164352920501969098E-14, -1.058809993658036520E-13, -40.00000000000000000 ) ) ;
#19519 = ORIENTED_EDGE ( 'NONE', *, *, #1788, .T. ) ;
#19520 = CARTESIAN_POINT ( 'NONE',  ( 6.004904395537136175, 19.19999999999999574, 0.000000000000000000 ) ) ;
#19521 = LINE ( 'NONE', #22372, #22190 ) ;
#19522 = FACE_OUTER_BOUND ( 'NONE', #40283, .T. ) ;
#19523 = CARTESIAN_POINT ( 'NONE',  ( 17.99999999999999645, -99.97660604680010010, 67.26937820704857529 ) ) ;
#19524 = ORIENTED_EDGE ( 'NONE', *, *, #14377, .F. ) ;
#19525 = CYLINDRICAL_SURFACE ( 'NONE', #3334, 59.00000000000000000 ) ;
#19526 = ORIENTED_EDGE ( 'NONE', *, *, #5494, .T. ) ;
#19527 = DIRECTION ( 'NONE',  ( 0.000000000000000000, 0.000000000000000000, -1.000000000000000000 ) ) ;
#19528 = EDGE_CURVE ( 'NONE', #32115, #4308, #41474, .T. ) ;
#19529 = ORIENTED_EDGE ( 'NONE', *, *, #5102, .F. ) ;
#19531 = ORIENTED_EDGE ( 'NONE', *, *, #22562, .F. ) ;
#19530 = FACE_OUTER_BOUND ( 'NONE', #38056, .T. ) ;
#19532 = ADVANCED_FACE ( 'NONE', ( #17543 ), #4841, .T. ) ;
#19533 = CARTESIAN_POINT ( 'NONE',  ( 55.55275676652586725, 31.00000000000000355, 14.97830846782891356 ) ) ;
#19534 = ORIENTED_EDGE ( 'NONE', *, *, #36669, .F. ) ;
#19535 = LINE ( 'NONE', #5970, #13331 ) ;
#19536 = ADVANCED_FACE ( 'NONE', ( #37774 ), #11623, .T. ) ;
#19537 = VERTEX_POINT ( 'NONE', #37991 ) ;
#19538 = CARTESIAN_POINT ( 'NONE',  ( 17.99999999999999645, -29.03409033315590904, 12.21509719675380623 ) ) ;
#19539 = VERTEX_POINT ( 'NONE', #1341 ) ;
#19540 = CARTESIAN_POINT ( 'NONE',  ( -79.00001692107187523, 40.00000000000000711, 21.04436337234429999 ) ) ;
#19541 = AXIS2_PLACEMENT_3D ( 'NONE', #27221, #121, #24185 ) ;
#19542 = AXIS2_PLACEMENT_3D ( 'NONE', #21239, #33176, #425 ) ;
#19544 = CARTESIAN_POINT ( 'NONE',  ( -102.9608013043458072, -40.05525454449572464, 14.45886780445738218 ) ) ;
#19543 = FACE_OUTER_BOUND ( 'NONE', #16263, .T. ) ;
#19545 = CARTESIAN_POINT ( 'NONE',  ( -106.4195705685748550, -106.4195705685759776, 6.999999999999998224 ) ) ;
#19546 = VERTEX_POINT ( 'NONE', #21042 ) ;
#19547 = FACE_OUTER_BOUND ( 'NONE', #40610, .T. ) ;
#19548 = ORIENTED_EDGE ( 'NONE', *, *, #19150, .F. ) ;
#19549 = ADVANCED_FACE ( 'NONE', ( #21481 ), #34941, .F. ) ;
#19550 = DIRECTION ( 'NONE',  ( 0.000000000000000000, 1.000000000000000000, 0.000000000000000000 ) ) ;
#19551 = CARTESIAN_POINT ( 'NONE',  ( 0.000000000000000000, -108.8880088604279166, 39.99251838045924501 ) ) ;
#19552 = CARTESIAN_POINT ( 'NONE',  ( -62.77658523491555798, 31.00000000000000711, 48.16944601536268777 ) ) ;
#19554 = DIRECTION ( 'NONE',  ( 0.000000000000000000, 0.000000000000000000, 1.000000000000000000 ) ) ;
#19553 = CARTESIAN_POINT ( 'NONE',  ( -130.0000000000000284, 4.615443851143735910E-16, 367.6955262170047263 ) ) ;
#19555 = VERTEX_POINT ( 'NONE', #24734 ) ;
#19556 = PRESENTATION_STYLE_ASSIGNMENT (( #2068 ) ) ;
#19557 = AXIS2_PLACEMENT_3D ( 'NONE', #41678, #5466, #1745 ) ;
#19558 = ORIENTED_EDGE ( 'NONE', *, *, #32163, .F. ) ;
#19559 = CARTESIAN_POINT ( 'NONE',  ( 0.000000000000000000, -30.03615769709762517, 42.44795908868979950 ) ) ;
#19560 = LINE ( 'NONE', #6218, #13723 ) ;
#19561 = CARTESIAN_POINT ( 'NONE',  ( 63.29164158772582027, 31.00000000000000000, -71.97807289022838972 ) ) ;
#19562 = CARTESIAN_POINT ( 'NONE',  ( 84.84057271799511568, 39.99999999999999289, 49.13019966419678752 ) ) ;
#19563 = CARTESIAN_POINT ( 'NONE',  ( 17.99999999999999645, 0.000000000000000000, 0.000000000000000000 ) ) ;
#19564 = EDGE_CURVE ( 'NONE', #4914, #41377, #34734, .T. ) ;
#19565 = DIRECTION ( 'NONE',  ( -1.000000000000000000, 0.000000000000000000, 0.000000000000000000 ) ) ;
#19566 = ORIENTED_EDGE ( 'NONE', *, *, #38261, .T. ) ;
#19567 = DIRECTION ( 'NONE',  ( -1.000000000000000000, 1.577021341797098793E-16, 0.000000000000000000 ) ) ;
#19568 = ORIENTED_EDGE ( 'NONE', *, *, #35724, .F. ) ;
#19569 = CIRCLE ( 'NONE', #28600, 120.5010000000000332 ) ;
#19570 = DIRECTION ( 'NONE',  ( 1.000000000000000000, 0.000000000000000000, 0.000000000000000000 ) ) ;
#19571 = VECTOR ( 'NONE', #40019, 1000.000000000000000 ) ;
#19572 = AXIS2_PLACEMENT_3D ( 'NONE', #5862, #32701, #28393 ) ;
#19573 = CARTESIAN_POINT ( 'NONE',  ( 18.00000000000000355, 0.000000000000000000, 0.000000000000000000 ) ) ;
#19574 = CARTESIAN_POINT ( 'NONE',  ( 0.000000000000000000, 16.77566611177940104, -119.3275660838940553 ) ) ;
#19575 = ORIENTED_EDGE ( 'NONE', *, *, #38625, .F. ) ;
#19576 = FACE_BOUND ( 'NONE', #3671, .T. ) ;
#19577 = CARTESIAN_POINT ( 'NONE',  ( 0.000000000000000000, 35.20873326984126805, -31.88259874183992792 ) ) ;
#19578 = EDGE_CURVE ( 'NONE', #30346, #9874, #36166, .T. ) ;
#19579 = CYLINDRICAL_SURFACE ( 'NONE', #24353, 120.5010000000000190 ) ;
#19581 = ORIENTED_EDGE ( 'NONE', *, *, #7650, .F. ) ;
#19580 = CARTESIAN_POINT ( 'NONE',  ( -99.67789407897798526, 39.99999999999999289, -5.066036069491909544 ) ) ;
#19582 = EDGE_CURVE ( 'NONE', #38585, #16643, #43111, .T. ) ;
#19583 = CARTESIAN_POINT ( 'NONE',  ( -21.70016380022026681, 31.00000000000000355, -5.809120511592387182 ) ) ;
#19584 = DIRECTION ( 'NONE',  ( 1.000000000000000000, 0.000000000000000000, 0.000000000000000000 ) ) ;
#19586 = ORIENTED_EDGE ( 'NONE', *, *, #15106, .F. ) ;
#19585 = DIRECTION ( 'NONE',  ( 0.000000000000000000, 1.000000000000000000, -1.060184893785364939E-15 ) ) ;
#19587 = VERTEX_POINT ( 'NONE', #40600 ) ;
#19588 = DIRECTION ( 'NONE',  ( 0.000000000000000000, 0.000000000000000000, 1.000000000000000000 ) ) ;
#19589 = DIRECTION ( 'NONE',  ( 1.000000000000000000, 0.000000000000000000, 0.000000000000000000 ) ) ;
#19590 = CARTESIAN_POINT ( 'NONE',  ( -14.09736097164574709, 40.00000000000000000, -41.75563764761122343 ) ) ;
#19591 = DIRECTION ( 'NONE',  ( 0.000000000000000000, 0.000000000000000000, -1.000000000000000000 ) ) ;
#19592 = AXIS2_PLACEMENT_3D ( 'NONE', #33145, #42949, #166 ) ;
#19593 = CARTESIAN_POINT ( 'NONE',  ( -1.393927851585477606, 4.043713361053528743, -3.526374918436835149 ) ) ;
#19594 = CARTESIAN_POINT ( 'NONE',  ( -99.99999999999997158, 35.50000000000000711, 2.428179185498535730E-12 ) ) ;
#19595 = ORIENTED_EDGE ( 'NONE', *, *, #33877, .F. ) ;
#19596 = DIRECTION ( 'NONE',  ( 0.000000000000000000, 0.000000000000000000, -1.000000000000000000 ) ) ;
#19597 = ORIENTED_EDGE ( 'NONE', *, *, #36270, .F. ) ;
#19599 = ADVANCED_FACE ( 'NONE', ( #4172 ), #24312, .F. ) ;
#19598 = CIRCLE ( 'NONE', #31422, 59.00000000000000711 ) ;
#19600 = LINE ( 'NONE', #22893, #18371 ) ;
#19601 = CARTESIAN_POINT ( 'NONE',  ( -4.024497503033519941, -2.323544716729390558, -3.572167766733381544 ) ) ;
#19602 = CIRCLE ( 'NONE', #7007, 116.0000000000000000 ) ;
#19605 = EDGE_CURVE ( 'NONE', #20337, #20302, #10742, .T. ) ;
#19604 = CARTESIAN_POINT ( 'NONE',  ( 38.32544124395173668, 31.00000000000000355, -22.13982348525413002 ) ) ;
#19603 = CIRCLE ( 'NONE', #14021, 4.500000000000000888 ) ;
#19606 = CYLINDRICAL_SURFACE ( 'NONE', #3684, 36.00000000000000000 ) ;
#19607 = ORIENTED_EDGE ( 'NONE', *, *, #26538, .T. ) ;
#19608 = AXIS2_PLACEMENT_3D ( 'NONE', #15704, #19628, #42280 ) ;
#19609 = CARTESIAN_POINT ( 'NONE',  ( 0.000000000000000000, 47.22458491092827160, -5.098390039073737334 ) ) ;
#19610 = CARTESIAN_POINT ( 'NONE',  ( 57.06996419934371545, 31.00000000000000000, 65.05326946699807422 ) ) ;
#19611 = AXIS2_PLACEMENT_3D ( 'NONE', #36392, #26815, #10223 ) ;
#19612 = EDGE_CURVE ( 'NONE', #35443, #16220, #8993, .T. ) ;
#19613 = CARTESIAN_POINT ( 'NONE',  ( 0.000000000000000000, 0.000000000000000000, 0.000000000000000000 ) ) ;
#19614 = ORIENTED_EDGE ( 'NONE', *, *, #15023, .F. ) ;
#19615 = CARTESIAN_POINT ( 'NONE',  ( 34.31975892712151222, 31.00000000000000355, 59.64049725130579560 ) ) ;
#19616 = CARTESIAN_POINT ( 'NONE',  ( 60.82800096160986669, 39.99999999999999289, 30.10617641797072963 ) ) ;
#19617 = DIRECTION ( 'NONE',  ( -1.000000000000000000, 0.000000000000000000, -0.000000000000000000 ) ) ;
#19618 = EDGE_CURVE ( 'NONE', #4417, #952, #41256, .T. ) ;
#19619 = VERTEX_POINT ( 'NONE', #11401 ) ;
#19620 =( NAMED_UNIT ( * ) SI_UNIT ( $, .STERADIAN. ) SOLID_ANGLE_UNIT ( ) );
#19621 = CYLINDRICAL_SURFACE ( 'NONE', #1263, 59.00000000000000000 ) ;
#19622 = FACE_OUTER_BOUND ( 'NONE', #7416, .T. ) ;
#19624 = VERTEX_POINT ( 'NONE', #31471 ) ;
#19623 = CARTESIAN_POINT ( 'NONE',  ( 4.211140560182196957, 2.431303136016536470, -3.745885042887433514 ) ) ;
#19625 = DIRECTION ( 'NONE',  ( -1.000000000000000000, 0.000000000000000000, -0.000000000000000000 ) ) ;
#19626 = CIRCLE ( 'NONE', #7033, 52.00000000000000000 ) ;
#19627 = ORIENTED_EDGE ( 'NONE', *, *, #13118, .F. ) ;
#19628 = DIRECTION ( 'NONE',  ( -1.000000000000000000, -0.000000000000000000, -0.000000000000000000 ) ) ;
#19629 = ADVANCED_FACE ( 'NONE', ( #1557 ), #1120, .F. ) ;
#19630 = CARTESIAN_POINT ( 'NONE',  ( 74.30822294231431613, 39.99999999999999289, -9.796771932235298408 ) ) ;
#19631 = LINE ( 'NONE', #6714, #33348 ) ;
#19632 = CIRCLE ( 'NONE', #10536, 120.5010000000000474 ) ;
#19633 = AXIS2_PLACEMENT_3D ( 'NONE', #41380, #8663, #31166 ) ;
#19634 = ORIENTED_EDGE ( 'NONE', *, *, #36140, .T. ) ;
#19635 = DIRECTION ( 'NONE',  ( 0.000000000000000000, 0.000000000000000000, 1.000000000000000000 ) ) ;
#19636 = ADVANCED_FACE ( 'NONE', ( #4614 ), #38630, .T. ) ;
#19637 = DIRECTION ( 'NONE',  ( -1.000000000000000000, 0.000000000000000000, 0.000000000000000000 ) ) ;
#19638 = AXIS2_PLACEMENT_3D ( 'NONE', #11515, #21593, #31573 ) ;
#19639 = EDGE_CURVE ( 'NONE', #9213, #4169, #9708, .T. ) ;
#19640 = VERTEX_POINT ( 'NONE', #8974 ) ;
#19641 = EDGE_LOOP ( 'NONE', ( #23098, #30894, #26738, #26990 ) ) ;
#19642 = DIRECTION ( 'NONE',  ( 0.000000000000000000, 0.000000000000000000, 1.000000000000000000 ) ) ;
#19643 = ORIENTED_EDGE ( 'NONE', *, *, #35137, .T. ) ;
#19644 = AXIS2_PLACEMENT_3D ( 'NONE', #14271, #33892, #10552 ) ;
#19645 = DIRECTION ( 'NONE',  ( -1.000000000000000000, -0.000000000000000000, -0.000000000000000000 ) ) ;
#19646 = DIRECTION ( 'NONE',  ( 1.000000000000000000, 0.000000000000000000, 0.000000000000000000 ) ) ;
#19647 = DIRECTION ( 'NONE',  ( 0.000000000000000000, 0.000000000000000000, 1.000000000000000000 ) ) ;
#19648 = CARTESIAN_POINT ( 'NONE',  ( 18.00000000000000355, -51.19683565102450729, 9.104066087303294807 ) ) ;
#19649 = ORIENTED_EDGE ( 'NONE', *, *, #31170, .F. ) ;
#19650 = DIRECTION ( 'NONE',  ( -1.000000000000000000, -0.000000000000000000, -0.000000000000000000 ) ) ;
#19651 = EDGE_LOOP ( 'NONE', ( #19005, #18420, #17384, #690 ) ) ;
#19652 = DIRECTION ( 'NONE',  ( -1.000000000000000000, -0.000000000000000000, 0.000000000000000000 ) ) ;
#19653 = EDGE_CURVE ( 'NONE', #40785, #42378, #34093, .T. ) ;
#19654 = EDGE_CURVE ( 'NONE', #501, #21663, #14596, .T. ) ;
#19655 = ORIENTED_EDGE ( 'NONE', *, *, #1519, .T. ) ;
#19656 = DIRECTION ( 'NONE',  ( 1.000000000000000000, -0.000000000000000000, -0.000000000000000000 ) ) ;
#19657 = EDGE_CURVE ( 'NONE', #31940, #20361, #33374, .T. ) ;
#19658 = EDGE_CURVE ( 'NONE', #2020, #29479, #29221, .T. ) ;
#19659 = CARTESIAN_POINT ( 'NONE',  ( 0.000000000000000000, -105.7179949885870514, 37.57629584241652054 ) ) ;
#19660 = APPLICATION_PROTOCOL_DEFINITION ( 'draft international standard', 'automotive_design', 1998, #7795 ) ;
#19661 = DIRECTION ( 'NONE',  ( 1.000000000000000000, 0.000000000000000000, 0.000000000000000000 ) ) ;
#19662 = CARTESIAN_POINT ( 'NONE',  ( 20.30000058474805869, 31.00000000000000355, -59.80472289869057789 ) ) ;
#19663 = AXIS2_PLACEMENT_3D ( 'NONE', #1576, #11423, #28229 ) ;
#19664 = AXIS2_PLACEMENT_3D ( 'NONE', #2301, #39177, #12396 ) ;
#19665 = ORIENTED_EDGE ( 'NONE', *, *, #29006, .T. ) ;
#19666 = CARTESIAN_POINT ( 'NONE',  ( 9.106956811745659408, 31.00000000000000355, -33.78410985267935018 ) ) ;
#19667 = CIRCLE ( 'NONE', #7800, 59.00000000000000711 ) ;
#19668 = CARTESIAN_POINT ( 'NONE',  ( -69.75709431192164800, 40.00000000000000711, -9.183449035091399537 ) ) ;
#19669 = AXIS2_PLACEMENT_3D ( 'NONE', #18666, #31698, #11651 ) ;
#19670 = CARTESIAN_POINT ( 'NONE',  ( 0.000000000000000000, 112.1427988504408404, -3.502162136922268409 ) ) ;
#19671 = CARTESIAN_POINT ( 'NONE',  ( -19.99999999999988276, -4.164463357862395064E-14, -25.99999999999999645 ) ) ;
#19672 = CARTESIAN_POINT ( 'NONE',  ( 17.99999999999999645, 19.69434969228073484, 24.58291258574055860 ) ) ;
#19673 = DIRECTION ( 'NONE',  ( 0.000000000000000000, 0.000000000000000000, 1.000000000000000000 ) ) ;
#19674 = EDGE_CURVE ( 'NONE', #16359, #39974, #34782, .T. ) ;
#19675 = ORIENTED_EDGE ( 'NONE', *, *, #3600, .T. ) ;
#19676 = CARTESIAN_POINT ( 'NONE',  ( -3.108867721649295035, 40.00000000000000000, 47.60416666525765095 ) ) ;
#19677 = FACE_OUTER_BOUND ( 'NONE', #25695, .T. ) ;
#19678 = DIRECTION ( 'NONE',  ( 0.000000000000000000, 0.000000000000000000, 1.000000000000000000 ) ) ;
#19679 = ORIENTED_EDGE ( 'NONE', *, *, #18512, .F. ) ;
#19680 = DIRECTION ( 'NONE',  ( 0.000000000000000000, -0.7705132427757949154, 0.6374239897486827511 ) ) ;
#19681 = CARTESIAN_POINT ( 'NONE',  ( 17.99999999999999645, 104.6166166098452379, -50.11350645393572023 ) ) ;
#19682 = VERTEX_POINT ( 'NONE', #15343 ) ;
#19683 = CARTESIAN_POINT ( 'NONE',  ( 17.99999999999999645, -31.17727234463623631, -111.7317219465823115 ) ) ;
#19684 = ORIENTED_EDGE ( 'NONE', *, *, #29609, .T. ) ;
#19685 = VECTOR ( 'NONE', #4309, 1000.000000000000000 ) ;
#19686 = AXIS2_PLACEMENT_3D ( 'NONE', #16865, #6785, #24048 ) ;
#19687 = ORIENTED_EDGE ( 'NONE', *, *, #11867, .T. ) ;
#19688 = DIRECTION ( 'NONE',  ( -1.000000000000000000, 0.000000000000000000, -0.000000000000000000 ) ) ;
#19689 = VECTOR ( 'NONE', #12734, 1000.000000000000000 ) ;
#19690 = CARTESIAN_POINT ( 'NONE',  ( 43.66223835209735427, 31.00000000000000355, 88.82794485014694885 ) ) ;
#19691 = ORIENTED_EDGE ( 'NONE', *, *, #7534, .T. ) ;
#19692 = CARTESIAN_POINT ( 'NONE',  ( 0.000000000000000000, -26.29521155129837595, -17.34211205339375184 ) ) ;
#19693 = VECTOR ( 'NONE', #18806, 1000.000000000000000 ) ;
#19694 = CARTESIAN_POINT ( 'NONE',  ( 0.000000000000000000, 0.000000000000000000, 0.000000000000000000 ) ) ;
#19695 = CARTESIAN_POINT ( 'NONE',  ( 17.99999999999999645, -73.78980555658542073, -95.26571049922065981 ) ) ;
#19696 = EDGE_LOOP ( 'NONE', ( #1612, #37638 ) ) ;
#19697 = DIRECTION ( 'NONE',  ( -3.009274222672345096E-17, -1.000000000000000000, 2.455023325076454960E-18 ) ) ;
#19698 = CIRCLE ( 'NONE', #3632, 14.91999999999999815 ) ;
#19699 = CARTESIAN_POINT ( 'NONE',  ( -153.1499999999986699, -2.921326824731410475E-13, 10.00000000000004441 ) ) ;
#19700 = EDGE_CURVE ( 'NONE', #5899, #42086, #1321, .T. ) ;
#19701 = EDGE_CURVE ( 'NONE', #39322, #31605, #31305, .T. ) ;
#19703 = DIRECTION ( 'NONE',  ( -1.000000000000000000, -0.000000000000000000, -0.000000000000000000 ) ) ;
#19702 = CARTESIAN_POINT ( 'NONE',  ( -9.000000000000005329, 14.91999999999999815, 0.000000000000000000 ) ) ;
#19704 = EDGE_CURVE ( 'NONE', #22705, #14740, #42424, .T. ) ;
#19705 = EDGE_CURVE ( 'NONE', #30314, #6504, #22741, .T. ) ;
#19706 = DIRECTION ( 'NONE',  ( 0.000000000000000000, 0.000000000000000000, 1.000000000000000000 ) ) ;
#19707 = ORIENTED_EDGE ( 'NONE', *, *, #22592, .T. ) ;
#19708 = EDGE_CURVE ( 'NONE', #15184, #13428, #28635, .T. ) ;
#19709 = CARTESIAN_POINT ( 'NONE',  ( 24.89583333603155069, 31.00000000000000355, -1.636246165087041016 ) ) ;
#19710 = ORIENTED_EDGE ( 'NONE', *, *, #35905, .T. ) ;
#19711 = CARTESIAN_POINT ( 'NONE',  ( 17.99999999999999645, 107.2885202478266251, 54.86040852957351888 ) ) ;
#19712 = CARTESIAN_POINT ( 'NONE',  ( 0.000000000000000000, 0.000000000000000000, 0.000000000000000000 ) ) ;
#19713 = ORIENTED_EDGE ( 'NONE', *, *, #36497, .F. ) ;
#19714 = ADVANCED_FACE ( 'NONE', ( #15127 ), #28432, .T. ) ;
#19715 = CARTESIAN_POINT ( 'NONE',  ( -6.075999999999999623, 0.000000000000000000, 15.08402000000000065 ) ) ;
#19716 = CARTESIAN_POINT ( 'NONE',  ( -39.95047694894377344, 40.00000000000000000, -5.256506769647570465 ) ) ;
#19717 = CARTESIAN_POINT ( 'NONE',  ( 46.89194940766294906, 40.00000000000000000, 6.259973086888630078 ) ) ;
#19718 = VECTOR ( 'NONE', #41392, 1000.000000000000000 ) ;
#19719 = ORIENTED_EDGE ( 'NONE', *, *, #8988, .F. ) ;
#19720 = VERTEX_POINT ( 'NONE', #35150 ) ;
#19721 = FACE_OUTER_BOUND ( 'NONE', #35648, .T. ) ;
#19722 = DIRECTION ( 'NONE',  ( 0.000000000000000000, 0.000000000000000000, 1.000000000000000000 ) ) ;
#19723 = AXIS2_PLACEMENT_3D ( 'NONE', #28552, #38118, #18758 ) ;
#19724 = DIRECTION ( 'NONE',  ( -1.000000000000000000, -0.000000000000000000, -0.000000000000000000 ) ) ;
#19725 = CARTESIAN_POINT ( 'NONE',  ( 18.00000000000000355, 11.90021268425555512, 45.45261810511218670 ) ) ;
#19726 = CARTESIAN_POINT ( 'NONE',  ( 17.99999999999999645, 25.52601536738592358, 19.21447964122706509 ) ) ;
#19727 = EDGE_LOOP ( 'NONE', ( #16053, #30867, #9948, #8224 ) ) ;
#19728 = DIRECTION ( 'NONE',  ( -1.000000000000000000, 0.000000000000000000, 0.000000000000000000 ) ) ;
#19729 = ORIENTED_EDGE ( 'NONE', *, *, #24596, .T. ) ;
#19730 = LINE ( 'NONE', #3076, #38260 ) ;
#19731 = CIRCLE ( 'NONE', #12064, 120.5010000000000190 ) ;
#19732 = CARTESIAN_POINT ( 'NONE',  ( 9.000000000000001776, 109.3506818544115617, -38.70953859160898247 ) ) ;
#19733 = VERTEX_POINT ( 'NONE', #12056 ) ;
#19734 = EDGE_CURVE ( 'NONE', #37965, #5452, #18142, .T. ) ;
#19735 = CARTESIAN_POINT ( 'NONE',  ( 17.99999999999999645, 0.000000000000000000, 0.000000000000000000 ) ) ;
#19736 = DIRECTION ( 'NONE',  ( -1.000000000000000000, 0.000000000000000000, -0.000000000000000000 ) ) ;
#19737 = VERTEX_POINT ( 'NONE', #22111 ) ;
#19738 = FACE_OUTER_BOUND ( 'NONE', #12457, .T. ) ;
#19739 = ORIENTED_EDGE ( 'NONE', *, *, #19364, .F. ) ;
#19740 = LINE ( 'NONE', #19107, #27018 ) ;
#19741 = EDGE_LOOP ( 'NONE', ( #27086, #8093, #16552, #14806 ) ) ;
#19743 = EDGE_LOOP ( 'NONE', ( #11969, #7126 ) ) ;
#19742 = CARTESIAN_POINT ( 'NONE',  ( 17.99999999999999645, 78.75547124681369837, 91.20343606297029737 ) ) ;
#19744 = CARTESIAN_POINT ( 'NONE',  ( 3.791180027291366716, 31.00000000000000355, 59.39995347152935778 ) ) ;
#19745 = ORIENTED_EDGE ( 'NONE', *, *, #23857, .F. ) ;
#19746 = CARTESIAN_POINT ( 'NONE',  ( -0.6666666666666666297, -4.233901974057276973, -3.300726591567087365 ) ) ;
#19747 = VERTEX_POINT ( 'NONE', #15756 ) ;
#19748 = CARTESIAN_POINT ( 'NONE',  ( 17.99999999999999645, -41.33768078145432412, -104.3046912715545318 ) ) ;
#19749 = VERTEX_POINT ( 'NONE', #5269 ) ;
#19750 = AXIS2_PLACEMENT_3D ( 'NONE', #34591, #40911, #1637 ) ;
#19751 = CARTESIAN_POINT ( 'NONE',  ( -60.98551593176824070, 40.00000000000000711, 53.34359504439791522 ) ) ;
#19753 = CARTESIAN_POINT ( 'NONE',  ( 0.000000000000000000, -24.47917365149914204, -45.87777302070959706 ) ) ;
#19752 = DIRECTION ( 'NONE',  ( 0.000000000000000000, 0.000000000000000000, -1.000000000000000000 ) ) ;
#19754 = EDGE_CURVE ( 'NONE', #8245, #34731, #32715, .T. ) ;
#19755 = ADVANCED_FACE ( 'NONE', ( #18636 ), #32523, .F. ) ;
#19756 = DIRECTION ( 'NONE',  ( -1.000000000000000000, 0.000000000000000000, -0.000000000000000000 ) ) ;
#19757 = ORIENTED_EDGE ( 'NONE', *, *, #28082, .F. ) ;
#19758 = CARTESIAN_POINT ( 'NONE',  ( 6.200000000000007283, -19.19999999999998508, 2.351321854362917290E-15 ) ) ;
#19759 =( GEOMETRIC_REPRESENTATION_CONTEXT ( 3 ) GLOBAL_UNCERTAINTY_ASSIGNED_CONTEXT ( ( #41772 ) ) GLOBAL_UNIT_ASSIGNED_CONTEXT ( ( #4708, #1636, #17630 ) ) REPRESENTATION_CONTEXT ( 'NONE', 'WORKASPACE' ) );
#19760 = EDGE_LOOP ( 'NONE', ( #21140, #15384, #20277, #29234 ) ) ;
#19761 = PRESENTATION_STYLE_ASSIGNMENT (( #9901 ) ) ;
#19762 = EDGE_CURVE ( 'NONE', #6492, #31141, #13937, .T. ) ;
#19763 = AXIS2_PLACEMENT_3D ( 'NONE', #26995, #29849, #9956 ) ;
#19764 = CARTESIAN_POINT ( 'NONE',  ( 17.99999999999999645, 1.592040838891559450E-14, -130.0000000000000000 ) ) ;
#19765 = DIRECTION ( 'NONE',  ( -1.000000000000000000, 0.000000000000000000, 0.000000000000000000 ) ) ;
#19766 = CARTESIAN_POINT ( 'NONE',  ( -36.24314215638268877, 31.00000000000000355, -73.49571118816069770 ) ) ;
#19768 = CARTESIAN_POINT ( 'NONE',  ( 9.000000000000000000, -34.45183346761142928, 10.44371441202643247 ) ) ;
#19767 = CARTESIAN_POINT ( 'NONE',  ( 0.000000000000000000, 0.000000000000000000, 0.000000000000000000 ) ) ;
#19769 = EDGE_LOOP ( 'NONE', ( #25904, #34549, #26224, #34894 ) ) ;
#19770 = EDGE_CURVE ( 'NONE', #41289, #10692, #22302, .T. ) ;
#19771 = DIRECTION ( 'NONE',  ( 1.000000000000000000, 1.836909530733573776E-16, 0.000000000000000000 ) ) ;
#19772 = EDGE_CURVE ( 'NONE', #18380, #23300, #16719, .T. ) ;
#19773 = ORIENTED_EDGE ( 'NONE', *, *, #41944, .F. ) ;
#19774 = CARTESIAN_POINT ( 'NONE',  ( 2.500000000000000000, 0.000000000000000000, 0.000000000000000000 ) ) ;
#19775 = DIRECTION ( 'NONE',  ( 1.000000000000000000, 0.000000000000000000, 0.000000000000000000 ) ) ;
#19776 = CARTESIAN_POINT ( 'NONE',  ( -24.28006566512905451, 31.00000000000000355, -91.10131089348453770 ) ) ;
#19777 = VECTOR ( 'NONE', #16265, 1000.000000000000227 ) ;
#19778 = CYLINDRICAL_SURFACE ( 'NONE', #25414, 59.00000000000000000 ) ;
#19779 = AXIS2_PLACEMENT_3D ( 'NONE', #27069, #30122, #7408 ) ;
#19780 = CARTESIAN_POINT ( 'NONE',  ( -109.0695705685749175, 106.4195705685765745, 10.00000000000033751 ) ) ;
#19781 = ORIENTED_EDGE ( 'NONE', *, *, #40787, .T. ) ;
#19782 = CARTESIAN_POINT ( 'NONE',  ( 17.99999999999999645, 112.1702510623870097, 2.471285140324554153 ) ) ;
#19783 = ORIENTED_EDGE ( 'NONE', *, *, #21279, .F. ) ;
#19784 = CARTESIAN_POINT ( 'NONE',  ( -10.00000000000000000, 0.000000000000000000, 0.000000000000000000 ) ) ;
#19785 = CARTESIAN_POINT ( 'NONE',  ( 17.99999999999999645, 0.000000000000000000, 0.000000000000000000 ) ) ;
#19786 = DIRECTION ( 'NONE',  ( -1.000000000000000000, 0.000000000000000000, 0.000000000000000000 ) ) ;
#19787 = VERTEX_POINT ( 'NONE', #19893 ) ;
#19788 = DIRECTION ( 'NONE',  ( -1.000000000000000000, -0.000000000000000000, -0.000000000000000000 ) ) ;
#19789 = CARTESIAN_POINT ( 'NONE',  ( 17.99999999999999645, 0.000000000000000000, 0.000000000000000000 ) ) ;
#19790 = DIRECTION ( 'NONE',  ( 1.000000000000000000, 0.000000000000000000, 0.000000000000000000 ) ) ;
#19791 = VECTOR ( 'NONE', #31768, 1000.000000000000000 ) ;
#19793 = VERTEX_POINT ( 'NONE', #3673 ) ;
#19792 = DIRECTION ( 'NONE',  ( -1.000000000000000000, -0.000000000000000000, -0.000000000000000000 ) ) ;
#19794 = CARTESIAN_POINT ( 'NONE',  ( -29.88476798293162418, 31.00000000000000355, 10.10044382456042911 ) ) ;
#19795 = DIRECTION ( 'NONE',  ( 1.000000000000000000, -0.000000000000000000, -0.000000000000000000 ) ) ;
#19796 = VECTOR ( 'NONE', #32589, 1000.000000000000000 ) ;
#19798 = ORIENTED_EDGE ( 'NONE', *, *, #9475, .T. ) ;
#19797 = DIRECTION ( 'NONE',  ( 1.000000000000000000, -0.000000000000000000, -0.000000000000000000 ) ) ;
#19799 = EDGE_LOOP ( 'NONE', ( #17439, #10805, #39943, #16233 ) ) ;
#19800 = DIRECTION ( 'NONE',  ( 0.000000000000000000, -0.5963673585384914322, -0.8027116379309710004 ) ) ;
#19801 = DIRECTION ( 'NONE',  ( -1.000000000000000000, -0.000000000000000000, 0.000000000000000000 ) ) ;
#19802 = CARTESIAN_POINT ( 'NONE',  ( -22.33566874673302038, 40.00000000000000000, 45.10700316350094141 ) ) ;
#19803 = CARTESIAN_POINT ( 'NONE',  ( 18.00000000000000355, -44.61570720899106846, 14.73072383765551940 ) ) ;
#19804 = CIRCLE ( 'NONE', #30216, 0.08000000000000020983 ) ;
#19805 = DIRECTION ( 'NONE',  ( 0.000000000000000000, 0.3612416661871537538, -0.9324722294043554793 ) ) ;
#19806 = AXIS2_PLACEMENT_3D ( 'NONE', #613, #4316, #27059 ) ;
#19807 = EDGE_CURVE ( 'NONE', #880, #24356, #19514, .T. ) ;
#19808 = DIRECTION ( 'NONE',  ( 1.000000000000000000, 0.000000000000000000, 0.000000000000000000 ) ) ;
#19809 = ORIENTED_EDGE ( 'NONE', *, *, #39111, .F. ) ;
#19810 = DIRECTION ( 'NONE',  ( 0.000000000000000000, 0.2631025642275218179, -0.9647678688145158166 ) ) ;
#19811 = EDGE_CURVE ( 'NONE', #15086, #3942, #42451, .T. ) ;
#19812 = VERTEX_POINT ( 'NONE', #23813 ) ;
#19813 = VECTOR ( 'NONE', #30972, 1000.000000000000000 ) ;
#19814 = DIRECTION ( 'NONE',  ( 0.000000000000000000, -3.528251137579946599E-15, -1.000000000000000000 ) ) ;
#19815 = CYLINDRICAL_SURFACE ( 'NONE', #37298, 47.49900000000000233 ) ;
#19816 = CARTESIAN_POINT ( 'NONE',  ( 28.34477777927418529, 31.00000000000000355, 36.93558740410973229 ) ) ;
#19817 = DIRECTION ( 'NONE',  ( -1.000000000000000000, -0.000000000000000000, -0.000000000000000000 ) ) ;
#19818 = ORIENTED_EDGE ( 'NONE', *, *, #22902, .T. ) ;
#19819 = EDGE_CURVE ( 'NONE', #14877, #6394, #33166, .T. ) ;
#19820 = AXIS2_PLACEMENT_3D ( 'NONE', #28410, #24941, #8519 ) ;
#19821 = EDGE_CURVE ( 'NONE', #9926, #10843, #11855, .T. ) ;
#19822 = LINE ( 'NONE', #8908, #12172 ) ;
#19823 = ORIENTED_EDGE ( 'NONE', *, *, #20734, .T. ) ;
#19824 = CARTESIAN_POINT ( 'NONE',  ( 38.45889818826288575, 31.00000000000000355, 77.98987599019784511 ) ) ;
#19825 = AXIS2_PLACEMENT_3D ( 'NONE', #42627, #22203, #12776 ) ;
#19826 = ADVANCED_FACE ( 'NONE', ( #36418 ), #40122, .F. ) ;
#19827 = CARTESIAN_POINT ( 'NONE',  ( -4.203833317240879275, -1.627343821129593859, -3.597273115243890818 ) ) ;
#19828 = ORIENTED_EDGE ( 'NONE', *, *, #27314, .F. ) ;
#19829 = CARTESIAN_POINT ( 'NONE',  ( -30.31917247938466176, 31.00000000000000355, 52.30862930534038924 ) ) ;
#19830 = CARTESIAN_POINT ( 'NONE',  ( -18.22940504111446458, 40.00000000000000000, 67.64968002090884625 ) ) ;
#19831 = CARTESIAN_POINT ( 'NONE',  ( 42.89041025189590783, 40.00000000000000000, 86.97820559439793442 ) ) ;
#19832 = ORIENTED_EDGE ( 'NONE', *, *, #35248, .F. ) ;
#19833 = ORIENTED_EDGE ( 'NONE', *, *, #356, .T. ) ;
#19834 = CARTESIAN_POINT ( 'NONE',  ( -1.274258131565027874, -3.883108878240886241, -3.220599429844051009 ) ) ;
#19835 = AXIS2_PLACEMENT_3D ( 'NONE', #33477, #7073, #40646 ) ;
#19836 = CARTESIAN_POINT ( 'NONE',  ( 0.000000000000000000, 150.5000000000000284, 6.999999999999998224 ) ) ;
#19837 = DIRECTION ( 'NONE',  ( 1.000000000000000000, -0.000000000000000000, -0.000000000000000000 ) ) ;
#19838 = AXIS2_PLACEMENT_3D ( 'NONE', #14620, #15055, #4537 ) ;
#19840 = ORIENTED_EDGE ( 'NONE', *, *, #16142, .T. ) ;
#19839 = CARTESIAN_POINT ( 'NONE',  ( 3.999999999999999112, 2.309401076758497595, -3.504271511726784194 ) ) ;
#19841 = FACE_OUTER_BOUND ( 'NONE', #31850, .T. ) ;
#19842 = ORIENTED_EDGE ( 'NONE', *, *, #16759, .T. ) ;
#19843 = LINE ( 'NONE', #16792, #15442 ) ;
#19844 = EDGE_CURVE ( 'NONE', #8139, #42638, #4851, .T. ) ;
#19845 = VECTOR ( 'NONE', #25077, 1000.000000000000000 ) ;
#19846 = CARTESIAN_POINT ( 'NONE',  ( -68.16583574478268304, 40.00000000000000711, -18.25112749842637427 ) ) ;
#19847 = CARTESIAN_POINT ( 'NONE',  ( 18.00000000000000355, -29.60891106212762125, -37.14118181634796656 ) ) ;
#19848 = ADVANCED_FACE ( 'NONE', ( #26422 ), #12899, .F. ) ;
#19849 = ORIENTED_EDGE ( 'NONE', *, *, #10236, .F. ) ;
#19850 = DIRECTION ( 'NONE',  ( -1.000000000000000000, -0.000000000000000000, -0.000000000000000000 ) ) ;
#19851 = EDGE_CURVE ( 'NONE', #6394, #8087, #31335, .T. ) ;
#19852 = DIRECTION ( 'NONE',  ( -1.000000000000000000, -0.000000000000000000, -0.000000000000000000 ) ) ;
#19853 = ORIENTED_EDGE ( 'NONE', *, *, #16508, .T. ) ;
#19854 = CARTESIAN_POINT ( 'NONE',  ( 47.87658044097961607, 31.00000000000000000, -82.67148682534870829 ) ) ;
#19855 = ORIENTED_EDGE ( 'NONE', *, *, #31707, .T. ) ;
#19856 = CARTESIAN_POINT ( 'NONE',  ( 17.99999999999999645, 0.000000000000000000, 0.000000000000000000 ) ) ;
#19857 = ORIENTED_EDGE ( 'NONE', *, *, #25694, .F. ) ;
#19858 = FACE_OUTER_BOUND ( 'NONE', #34814, .T. ) ;
#19859 = DIRECTION ( 'NONE',  ( -1.000000000000000000, 0.000000000000000000, 0.000000000000000000 ) ) ;
#19860 = CARTESIAN_POINT ( 'NONE',  ( 18.00000000000000355, 27.43636312076376527, -38.14186064215121519 ) ) ;
#19861 = DIRECTION ( 'NONE',  ( 0.000000000000000000, -0.9618256431728219313, 0.2736629900720729536 ) ) ;
#19862 = AXIS2_PLACEMENT_3D ( 'NONE', #33938, #18066, #5120 ) ;
#19863 = DIRECTION ( 'NONE',  ( 0.000000000000000000, 0.000000000000000000, 1.000000000000000000 ) ) ;
#19865 = ORIENTED_EDGE ( 'NONE', *, *, #32657, .F. ) ;
#19864 = VECTOR ( 'NONE', #5811, 1000.000000000000000 ) ;
#19866 = FACE_OUTER_BOUND ( 'NONE', #35811, .T. ) ;
#19867 = ADVANCED_FACE ( 'NONE', ( #6331 ), #27073, .F. ) ;
#19868 = ORIENTED_EDGE ( 'NONE', *, *, #29944, .F. ) ;
#19869 = LINE ( 'NONE', #5665, #34287 ) ;
#19870 = CARTESIAN_POINT ( 'NONE',  ( -7.088330391075835735, 31.00000000000000355, -20.85399598300688595 ) ) ;
#19871 = ORIENTED_EDGE ( 'NONE', *, *, #14324, .T. ) ;
#19872 = CARTESIAN_POINT ( 'NONE',  ( 17.99999999999999645, -17.33727698085101565, -110.8498592715975519 ) ) ;
#19873 = CIRCLE ( 'NONE', #32387, 120.5010000000000190 ) ;
#19874 = LINE ( 'NONE', #6308, #27235 ) ;
#19875 = ITEM_DEFINED_TRANSFORMATION ( 'NONE', 'NONE', #11463,  #13552 ) ;
#19876 = EDGE_CURVE ( 'NONE', #13970, #27094, #33402, .T. ) ;
#19878 = AXIS2_PLACEMENT_3D ( 'NONE', #11955, #5592, #22429 ) ;
#19877 = DIRECTION ( 'NONE',  ( -1.000000000000000000, -0.000000000000000000, -0.000000000000000000 ) ) ;
#19879 = CARTESIAN_POINT ( 'NONE',  ( 14.80739997004469366, 31.00000000000000355, 55.25628696611591550 ) ) ;
#19880 = EDGE_CURVE ( 'NONE', #30171, #24364, #36193, .T. ) ;
#19881 = ORIENTED_EDGE ( 'NONE', *, *, #4066, .T. ) ;
#19882 = CARTESIAN_POINT ( 'NONE',  ( -10.89792128226954127, 31.00000000000000355, -32.25956908330170592 ) ) ;
#19883 = EDGE_CURVE ( 'NONE', #22806, #16567, #647, .T. ) ;
#19884 = CARTESIAN_POINT ( 'NONE',  ( -69.89583333424914713, 40.00000000000000711, 4.581489278091138040 ) ) ;
#19885 = VECTOR ( 'NONE', #55, 1000.000000000000000 ) ;
#19886 = CARTESIAN_POINT ( 'NONE',  ( 18.00000000000000355, 0.000000000000000000, 0.000000000000000000 ) ) ;
#19887 = PRESENTATION_LAYER_ASSIGNMENT (  '', '', ( #28942 ) ) ;
#19888 = LINE ( 'NONE', #841, #12821 ) ;
#19889 = VECTOR ( 'NONE', #13676, 1000.000000000000000 ) ;
#19890 = LINE ( 'NONE', #9380, #35608 ) ;
#19891 = ORIENTED_EDGE ( 'NONE', *, *, #33751, .F. ) ;
#19892 = CARTESIAN_POINT ( 'NONE',  ( 42.20483333784007840, 40.00000000000000000, -14.33818270462009359 ) ) ;
#19893 = CARTESIAN_POINT ( 'NONE',  ( -20.00000000000000000, 0.000000000000000000, -20.00000000000000000 ) ) ;
#19895 = EDGE_CURVE ( 'NONE', #21604, #3997, #21630, .T. ) ;
#19894 = DIRECTION ( 'NONE',  ( -3.614007241618348771E-16, 1.000000000000000000, 0.000000000000000000 ) ) ;
#19896 = CIRCLE ( 'NONE', #4528, 59.00000000000000000 ) ;
#19897 = ORIENTED_EDGE ( 'NONE', *, *, #22924, .F. ) ;
#19898 = CIRCLE ( 'NONE', #1035, 116.0000000000000000 ) ;
#19899 = ADVANCED_FACE ( 'NONE', ( #19677 ), #32944, .F. ) ;
#19900 = CARTESIAN_POINT ( 'NONE',  ( 23.00000000000001421, -1.165156337948619932E-13, -39.99999999999999289 ) ) ;
#19901 = DIRECTION ( 'NONE',  ( -3.009274222672345096E-17, -1.000000000000000000, 2.455023325076454960E-18 ) ) ;
#19902 = EDGE_CURVE ( 'NONE', #5158, #8622, #42808, .T. ) ;
#19903 = AXIS2_PLACEMENT_3D ( 'NONE', #10123, #23693, #30212 ) ;
#19904 = ORIENTED_EDGE ( 'NONE', *, *, #11149, .T. ) ;
#19905 = DIRECTION ( 'NONE',  ( 1.000000000000000000, -3.009274222672345096E-17, 0.000000000000000000 ) ) ;
#19906 = ORIENTED_EDGE ( 'NONE', *, *, #18574, .T. ) ;
#19907 = VECTOR ( 'NONE', #26477, 1000.000000000000000 ) ;
#19908 = ORIENTED_EDGE ( 'NONE', *, *, #3600, .F. ) ;
#19909 = CARTESIAN_POINT ( 'NONE',  ( -106.4195705685748550, -106.4195705685759776, 6.999999999999998224 ) ) ;
#19910 = CARTESIAN_POINT ( 'NONE',  ( 94.26586287999620595, 31.00000000000000000, 25.37251369639959364 ) ) ;
#19911 = ORIENTED_EDGE ( 'NONE', *, *, #35361, .T. ) ;
#19912 = DIRECTION ( 'NONE',  ( 1.000000000000000000, -0.000000000000000000, -0.000000000000000000 ) ) ;
#19913 = CARTESIAN_POINT ( 'NONE',  ( 0.000000000000000000, -13.00789606333550097, 115.2683592318614672 ) ) ;
#19914 = FACE_BOUND ( 'NONE', #28544, .T. ) ;
#19915 = ORIENTED_EDGE ( 'NONE', *, *, #280, .F. ) ;
#19916 = FACE_OUTER_BOUND ( 'NONE', #31402, .T. ) ;
#19917 = ADVANCED_FACE ( 'NONE', ( #6531 ), #26635, .F. ) ;
#19918 = CIRCLE ( 'NONE', #15736, 59.00000000000000711 ) ;
#19919 = DIRECTION ( 'NONE',  ( 1.000000000000000000, 0.000000000000000000, 0.000000000000000000 ) ) ;
#19920 = CIRCLE ( 'NONE', #10839, 59.00000000000000711 ) ;
#19922 = CARTESIAN_POINT ( 'NONE',  ( 0.000000000000000000, 0.000000000000000000, 0.000000000000000000 ) ) ;
#19921 = CARTESIAN_POINT ( 'NONE',  ( 8.999999999999998224, 106.6051926090976991, -45.73109345704713746 ) ) ;
#19923 = AXIS2_PLACEMENT_3D ( 'NONE', #27749, #40570, #7642 ) ;
#19924 = CIRCLE ( 'NONE', #3128, 59.00000000000000000 ) ;
#19925 = DIRECTION ( 'NONE',  ( 0.000000000000000000, 1.000000000000000000, 0.000000000000000000 ) ) ;
#19926 = AXIS2_PLACEMENT_3D ( 'NONE', #19224, #35739, #28397 ) ;
#19927 = EDGE_LOOP ( 'NONE', ( #38983, #16117, #37323, #670 ) ) ;
#19928 = AXIS2_PLACEMENT_3D ( 'NONE', #456, #7663, #24065 ) ;
#19929 = EDGE_CURVE ( 'NONE', #18075, #39315, #42355, .T. ) ;
#19930 = CARTESIAN_POINT ( 'NONE',  ( -23.02120395722396395, 31.00000000000000355, 17.66995642160909696 ) ) ;
#19931 = ORIENTED_EDGE ( 'NONE', *, *, #2655, .F. ) ;
#19932 = CIRCLE ( 'NONE', #1067, 20.00000000000000355 ) ;
#19933 = CARTESIAN_POINT ( 'NONE',  ( 17.99999999999999645, 0.000000000000000000, 0.000000000000000000 ) ) ;
#19934 = ADVANCED_FACE ( 'NONE', ( #7414 ), #14418, .T. ) ;
#19935 = DIRECTION ( 'NONE',  ( -1.000000000000000000, 0.000000000000000000, -0.000000000000000000 ) ) ;
#19936 = EDGE_LOOP ( 'NONE', ( #35209, #14577, #23318, #9193 ) ) ;
#19937 = CARTESIAN_POINT ( 'NONE',  ( 0.000000000000000000, 0.000000000000000000, 0.000000000000000000 ) ) ;
#19938 = CARTESIAN_POINT ( 'NONE',  ( -5.542584477697039880, 40.00000000000000000, -42.01772079774592328 ) ) ;
#19939 = CARTESIAN_POINT ( 'NONE',  ( 44.12914893502614433, 40.00000000000000000, -14.89880614700436645 ) ) ;
#19940 = CIRCLE ( 'NONE', #20663, 12.50000000000000000 ) ;
#19941 = ORIENTED_EDGE ( 'NONE', *, *, #20947, .F. ) ;
#19942 = ORIENTED_EDGE ( 'NONE', *, *, #16760, .F. ) ;
#19943 = DIRECTION ( 'NONE',  ( 0.000000000000000000, -0.8183027759081622499, -0.5747874102144165942 ) ) ;
#19944 = CARTESIAN_POINT ( 'NONE',  ( 3.413765605486547727, -14.29811891091961229, -1.199999999999999956 ) ) ;
#19945 = DIRECTION ( 'NONE',  ( 0.000000000000000000, 1.000000000000000000, 0.000000000000000000 ) ) ;
#19946 = FACE_OUTER_BOUND ( 'NONE', #39609, .T. ) ;
#19947 = CARTESIAN_POINT ( 'NONE',  ( 2.500000000000000000, -2.357898499370432166, 3.035766082959412415E-15 ) ) ;
#19948 = ORIENTED_EDGE ( 'NONE', *, *, #31707, .F. ) ;
#19949 = DIRECTION ( 'NONE',  ( 1.000000000000000000, 0.000000000000000000, 0.000000000000000000 ) ) ;
#19950 = ORIENTED_EDGE ( 'NONE', *, *, #16250, .T. ) ;
#19951 = FACE_OUTER_BOUND ( 'NONE', #28977, .T. ) ;
#19952 = CARTESIAN_POINT ( 'NONE',  ( 17.99999999999999645, 112.5120133921107737, 43.14554256761054063 ) ) ;
#19953 = EDGE_CURVE ( 'NONE', #28718, #32806, #4558, .T. ) ;
#19954 = ORIENTED_EDGE ( 'NONE', *, *, #33676, .F. ) ;
#19955 = ADVANCED_FACE ( 'NONE', ( #34679 ), #13984, .F. ) ;
#19956 = DIRECTION ( 'NONE',  ( -1.000000000000000000, 0.000000000000000000, 0.000000000000000000 ) ) ;
#19957 = ADVANCED_FACE ( 'NONE', ( #40996 ), #41203, .F. ) ;
#19958 = EDGE_CURVE ( 'NONE', #21901, #20287, #24027, .T. ) ;
#19959 = EDGE_CURVE ( 'NONE', #37344, #34259, #32627, .T. ) ;
#19960 = CARTESIAN_POINT ( 'NONE',  ( 17.99999999999999645, -108.8684555192048435, 27.12806418649580564 ) ) ;
#19961 = ORIENTED_EDGE ( 'NONE', *, *, #22006, .F. ) ;
#19962 = CARTESIAN_POINT ( 'NONE',  ( -4.000000000000000000, 2.309401076758498483, -0.4999999999999927280 ) ) ;
#19963 = EDGE_LOOP ( 'NONE', ( #35391, #38967, #23446, #39056 ) ) ;
#19964 = VECTOR ( 'NONE', #17458, 1000.000000000000000 ) ;
#19965 = CARTESIAN_POINT ( 'NONE',  ( -19.99999999999999645, 40.00000000000000000, 1.283214542831032867 ) ) ;
#19966 = AXIS2_PLACEMENT_3D ( 'NONE', #40278, #3825, #4052 ) ;
#19967 = ORIENTED_EDGE ( 'NONE', *, *, #27345, .T. ) ;
#19968 = AXIS2_PLACEMENT_3D ( 'NONE', #18246, #41300, #1815 ) ;
#19970 = ORIENTED_EDGE ( 'NONE', *, *, #40732, .T. ) ;
#19969 = CARTESIAN_POINT ( 'NONE',  ( 12.50000000000000000, 0.000000000000000000, -25.00000000000000000 ) ) ;
#19971 = CARTESIAN_POINT ( 'NONE',  ( -40.14822235767833547, 31.00000000000000355, 45.62378674120104449 ) ) ;
#19972 = VERTEX_POINT ( 'NONE', #14641 ) ;
#19973 = LINE ( 'NONE', #13622, #40447 ) ;
#19974 = AXIS2_PLACEMENT_3D ( 'NONE', #25745, #18144, #31841 ) ;
#19975 = VERTEX_POINT ( 'NONE', #37294 ) ;
#19976 = CARTESIAN_POINT ( 'NONE',  ( 0.000000000000000000, 0.000000000000000000, 6.999999999999998224 ) ) ;
#19977 = CIRCLE ( 'NONE', #1111, 20.00000000000000711 ) ;
#19978 = EDGE_LOOP ( 'NONE', ( #10063, #9636, #24652, #23560 ) ) ;
#19979 = CARTESIAN_POINT ( 'NONE',  ( 5.085823974618865151, 40.00000000000000000, 79.40009828669005287 ) ) ;
#19981 = CARTESIAN_POINT ( 'NONE',  ( 18.00000000000000355, 0.000000000000000000, 0.000000000000000000 ) ) ;
#19980 = DIRECTION ( 'NONE',  ( 0.000000000000000000, 0.000000000000000000, 1.000000000000000000 ) ) ;
#19982 = DIRECTION ( 'NONE',  ( -1.000000000000000000, 0.000000000000000000, 0.000000000000000000 ) ) ;
#19983 = ORIENTED_EDGE ( 'NONE', *, *, #26258, .T. ) ;
#19984 = CARTESIAN_POINT ( 'NONE',  ( 0.000000000000000000, 51.93417535146740249, 2.615612846549354664 ) ) ;
#19985 = ORIENTED_EDGE ( 'NONE', *, *, #5831, .T. ) ;
#19986 = APPLICATION_PROTOCOL_DEFINITION ( 'draft international standard', 'automotive_design', 1998, #35625 ) ;
#19987 = DIRECTION ( 'NONE',  ( 3.009274222672345096E-17, 1.000000000000000000, -2.455023325076454960E-18 ) ) ;
#19988 = CARTESIAN_POINT ( 'NONE',  ( -34.66105084696506822, 31.00000000000000355, 70.31756248751102589 ) ) ;
#19989 = EDGE_CURVE ( 'NONE', #31004, #12380, #27948, .T. ) ;
#19991 = CARTESIAN_POINT ( 'NONE',  ( 18.00000000000000355, 0.000000000000000000, 0.000000000000000000 ) ) ;
#19990 = DIRECTION ( 'NONE',  ( 0.000000000000000000, 0.000000000000000000, 1.000000000000000000 ) ) ;
#19992 = VECTOR ( 'NONE', #23579, 1000.000000000000000 ) ;
#19993 = VERTEX_POINT ( 'NONE', #846 ) ;
#19994 = CIRCLE ( 'NONE', #26940, 120.5010000000000190 ) ;
#19995 = CIRCLE ( 'NONE', #1130, 12.49999999999993427 ) ;
#19996 = AXIS2_PLACEMENT_3D ( 'NONE', #39355, #9063, #2275 ) ;
#19997 = FACE_OUTER_BOUND ( 'NONE', #17586, .T. ) ;
#19998 = VECTOR ( 'NONE', #22159, 1000.000000000000000 ) ;
#19999 = EDGE_LOOP ( 'NONE', ( #21113, #10549, #19840, #2313 ) ) ;
#20000 = CARTESIAN_POINT ( 'NONE',  ( 9.999999999999998224, 0.000000000000000000, 0.000000000000000000 ) ) ;
#20001 = DIRECTION ( 'NONE',  ( 0.000000000000000000, -0.4610925014493325591, 0.8873520750565681015 ) ) ;
#20002 = CARTESIAN_POINT ( 'NONE',  ( 0.000000000000000000, 75.72520367775197769, -82.78868281115903471 ) ) ;
#20003 = AXIS2_PLACEMENT_3D ( 'NONE', #34832, #21365, #15448 ) ;
#20004 = DIRECTION ( 'NONE',  ( -1.000000000000000000, 0.000000000000000000, 0.000000000000000000 ) ) ;
#20005 = VECTOR ( 'NONE', #27679, 1000.000000000000000 ) ;
#20006 = DIRECTION ( 'NONE',  ( 0.000000000000000000, 0.000000000000000000, 1.000000000000000000 ) ) ;
#20007 = EDGE_LOOP ( 'NONE', ( #40597, #35587, #740, #40144 ) ) ;
#20008 = CARTESIAN_POINT ( 'NONE',  ( 0.000000000000000000, 119.0898412705476943, -18.38751498043618682 ) ) ;
#20009 = ORIENTED_EDGE ( 'NONE', *, *, #1846, .F. ) ;
#20010 = DIRECTION ( 'NONE',  ( -1.847415842360817977E-16, 1.000000000000000000, 0.000000000000000000 ) ) ;
#20011 = CIRCLE ( 'NONE', #10928, 51.99999999999999289 ) ;
#20012 = CARTESIAN_POINT ( 'NONE',  ( 0.000000000000000000, -116.0452958106482981, 32.46506308663420270 ) ) ;
#20013 = EDGE_CURVE ( 'NONE', #42401, #32464, #561, .T. ) ;
#20014 = EDGE_CURVE ( 'NONE', #16388, #14749, #43141, .T. ) ;
#20015 = DIRECTION ( 'NONE',  ( -1.000000000000000000, -0.000000000000000000, -0.000000000000000000 ) ) ;
#20016 = ORIENTED_EDGE ( 'NONE', *, *, #16437, .T. ) ;
#20017 = ORIENTED_EDGE ( 'NONE', *, *, #24716, .T. ) ;
#20018 = CARTESIAN_POINT ( 'NONE',  ( 17.99999999999999645, -84.62908780824929522, 85.78116633471262276 ) ) ;
#20019 = CARTESIAN_POINT ( 'NONE',  ( 17.99999999999999645, 31.81777574834302058, 2.898764365605871696 ) ) ;
#20020 = EDGE_CURVE ( 'NONE', #39452, #8913, #14199, .T. ) ;
#20021 = CARTESIAN_POINT ( 'NONE',  ( 0.000000000000000000, -22.82995208772658557, -41.06517797613689424 ) ) ;
#20023 = ORIENTED_EDGE ( 'NONE', *, *, #38434, .T. ) ;
#20022 = CARTESIAN_POINT ( 'NONE',  ( 0.000000000000000000, 0.000000000000000000, 0.000000000000000000 ) ) ;
#20024 = CARTESIAN_POINT ( 'NONE',  ( 17.12248163736668261, 31.00000000000000355, 34.87662400048955647 ) ) ;
#20025 = DIRECTION ( 'NONE',  ( 0.000000000000000000, 4.445596433350732597E-14, -1.000000000000000000 ) ) ;
#20026 = AXIS2_PLACEMENT_3D ( 'NONE', #23070, #29379, #22226 ) ;
#20027 = TOROIDAL_SURFACE ( 'NONE', #40864, 15.08402000000000065, 0.08402000000000148239 ) ;
#20029 = ORIENTED_EDGE ( 'NONE', *, *, #6196, .F. ) ;
#20028 = CYLINDRICAL_SURFACE ( 'NONE', #39044, 51.99999999999999289 ) ;
#20030 = ORIENTED_EDGE ( 'NONE', *, *, #12645, .F. ) ;
#20031 = CARTESIAN_POINT ( 'NONE',  ( 18.00000000000000355, -44.75336757549789013, 14.30704879393590012 ) ) ;
#20032 = CARTESIAN_POINT ( 'NONE',  ( 0.000000000000000000, 0.000000000000000000, 0.000000000000000000 ) ) ;
#20033 = CARTESIAN_POINT ( 'NONE',  ( 54.79583221321230724, 40.00000000000000000, -14.58025558542526490 ) ) ;
#20034 = AXIS2_PLACEMENT_3D ( 'NONE', #23854, #31665, #34495 ) ;
#20035 = DIRECTION ( 'NONE',  ( -1.000000000000000000, -0.000000000000000000, 0.000000000000000000 ) ) ;
#20036 = ADVANCED_FACE ( 'NONE', ( #24682 ), #40769, .F. ) ;
#20037 = VECTOR ( 'NONE', #288, 1000.000000000000000 ) ;
#20038 = DIRECTION ( 'NONE',  ( 1.000000000000000000, 1.836909530733573776E-16, 0.000000000000000000 ) ) ;
#20039 = FACE_OUTER_BOUND ( 'NONE', #11593, .T. ) ;
#20040 = ORIENTED_EDGE ( 'NONE', *, *, #41748, .T. ) ;
#20041 = LINE ( 'NONE', #26988, #26516 ) ;
#20043 = ORIENTED_EDGE ( 'NONE', *, *, #23886, .T. ) ;
#20042 = CIRCLE ( 'NONE', #33917, 59.00000000000000711 ) ;
#20044 = FACE_OUTER_BOUND ( 'NONE', #32136, .T. ) ;
#20045 = DIRECTION ( 'NONE',  ( -1.000000000000000000, 0.000000000000000000, -0.000000000000000000 ) ) ;
#20046 = CARTESIAN_POINT ( 'NONE',  ( -49.46937513889707105, 31.00000000000000355, 6.524320044134898744 ) ) ;
#20047 = FACE_OUTER_BOUND ( 'NONE', #1701, .T. ) ;
#20048 = ORIENTED_EDGE ( 'NONE', *, *, #11236, .T. ) ;
#20049 = EDGE_CURVE ( 'NONE', #9442, #10476, #35426, .T. ) ;
#20050 = PRODUCT_DEFINITION_SHAPE ( 'NONE', 'NONE',  #43201 ) ;
#20051 = CARTESIAN_POINT ( 'NONE',  ( 17.99999999999999645, 30.74337109795219547, -8.695908345466218492 ) ) ;
#20052 = ORIENTED_EDGE ( 'NONE', *, *, #18739, .T. ) ;
#20053 = CARTESIAN_POINT ( 'NONE',  ( -1.472621547668719444, 40.00000000000000000, -22.39583333634585571 ) ) ;
#20054 = VERTEX_POINT ( 'NONE', #31207 ) ;
#20055 = CARTESIAN_POINT ( 'NONE',  ( 17.99999999999999645, 69.90696807222488474, 98.15042952503540619 ) ) ;
#20056 = ORIENTED_EDGE ( 'NONE', *, *, #35187, .T. ) ;
#20057 = CARTESIAN_POINT ( 'NONE',  ( -16.51797447735581059, 31.00000000000000355, -62.05742538355529803 ) ) ;
#20058 = CARTESIAN_POINT ( 'NONE',  ( -60.39136959355892031, 40.00000000000000711, -16.27924862580663046 ) ) ;
#20059 = CARTESIAN_POINT ( 'NONE',  ( 17.99999999999999645, -111.1352304691226607, -15.40237066878709449 ) ) ;
#20060 = AXIS2_PLACEMENT_3D ( 'NONE', #15749, #42530, #12255 ) ;
#20061 = AXIS2_PLACEMENT_3D ( 'NONE', #38858, #21902, #25380 ) ;
#20062 = ORIENTED_EDGE ( 'NONE', *, *, #26147, .F. ) ;
#20063 = ORIENTED_EDGE ( 'NONE', *, *, #5961, .T. ) ;
#20064 = AXIS2_PLACEMENT_3D ( 'NONE', #40495, #14792, #20927 ) ;
#20065 = DIRECTION ( 'NONE',  ( 1.000000000000000000, 0.000000000000000000, 0.000000000000000000 ) ) ;
#20066 = AXIS2_PLACEMENT_3D ( 'NONE', #36269, #42398, #9881 ) ;
#20067 = DIRECTION ( 'NONE',  ( 1.000000000000000000, 0.000000000000000000, 0.000000000000000000 ) ) ;
#20068 = DIRECTION ( 'NONE',  ( 0.000000000000000000, 0.000000000000000000, 1.000000000000000000 ) ) ;
#20069 = VECTOR ( 'NONE', #32415, 1000.000000000000000 ) ;
#20071 = ORIENTED_EDGE ( 'NONE', *, *, #39567, .F. ) ;
#20070 = DIRECTION ( 'NONE',  ( -1.000000000000000000, -0.000000000000000000, -0.000000000000000000 ) ) ;
#20072 = ADVANCED_FACE ( 'NONE', ( #8059 ), #4796, .T. ) ;
#20073 = DIRECTION ( 'NONE',  ( -1.000000000000000000, 0.000000000000000000, 0.000000000000000000 ) ) ;
#20074 = ORIENTED_EDGE ( 'NONE', *, *, #1469, .F. ) ;
#20075 = CARTESIAN_POINT ( 'NONE',  ( -10.00000000000000000, 0.000000000000000000, 0.000000000000000000 ) ) ;
#20076 = PRODUCT_RELATED_PRODUCT_CATEGORY ( 'part', '', ( #42610 ) ) ;
#20077 = CARTESIAN_POINT ( 'NONE',  ( 22.58587702529213104, 40.00000000000000000, 84.29678642628191199 ) ) ;
#20078 = DIRECTION ( 'NONE',  ( -3.009274222672345096E-17, -1.000000000000000000, 2.455023325076455345E-18 ) ) ;
#20079 = AXIS2_PLACEMENT_3D ( 'NONE', #14379, #7809, #27249 ) ;
#20080 = ORIENTED_EDGE ( 'NONE', *, *, #23616, .T. ) ;
#20081 = DIRECTION ( 'NONE',  ( 0.000000000000000000, -0.9618256431728160472, -0.2736629900720938813 ) ) ;
#20082 = DIRECTION ( 'NONE',  ( 1.000000000000000000, 0.000000000000000000, 0.000000000000000000 ) ) ;
#20083 = EDGE_CURVE ( 'NONE', #40347, #6169, #38907, .T. ) ;
#20084 = ORIENTED_EDGE ( 'NONE', *, *, #29566, .F. ) ;
#20085 = ADVANCED_FACE ( 'NONE', ( #20540 ), #33810, .T. ) ;
#20086 = ORIENTED_EDGE ( 'NONE', *, *, #35757, .T. ) ;
#20087 = CYLINDRICAL_SURFACE ( 'NONE', #29559, 116.0000000000000000 ) ;
#20088 = ORIENTED_EDGE ( 'NONE', *, *, #26626, .T. ) ;
#20089 = CARTESIAN_POINT ( 'NONE',  ( 25.13348990051749965, 40.00000000000000000, -8.510361017570636122 ) ) ;
#20090 = CARTESIAN_POINT ( 'NONE',  ( 17.99999999999999645, 31.80866420683990725, 2.997093558041416195 ) ) ;
#20091 = CARTESIAN_POINT ( 'NONE',  ( 17.99999999999999645, 0.000000000000000000, 0.000000000000000000 ) ) ;
#20092 = VECTOR ( 'NONE', #6176, 1000.000000000000000 ) ;
#20093 = CARTESIAN_POINT ( 'NONE',  ( 18.00000000000000355, 42.41764978026607480, -20.20639853260305685 ) ) ;
#20094 = DIRECTION ( 'NONE',  ( 0.000000000000000000, 0.000000000000000000, 1.000000000000000000 ) ) ;
#20095 = ORIENTED_EDGE ( 'NONE', *, *, #29330, .T. ) ;
#20096 = AXIS2_PLACEMENT_3D ( 'NONE', #7617, #4328, #7175 ) ;
#20097 = CYLINDRICAL_SURFACE ( 'NONE', #34215, 20.00000000000000000 ) ;
#20098 = VECTOR ( 'NONE', #21859, 1000.000000000000000 ) ;
#20099 = ORIENTED_EDGE ( 'NONE', *, *, #37764, .F. ) ;
#20100 = AXIS2_PLACEMENT_3D ( 'NONE', #7285, #36963, #34129 ) ;
#20101 = CARTESIAN_POINT ( 'NONE',  ( 0.000000000000000000, 43.55304910509406824, 28.41006711800000062 ) ) ;
#20102 = CARTESIAN_POINT ( 'NONE',  ( 0.000000000000000000, 44.75336757549779776, 14.30704879393622164 ) ) ;
#20103 = ORIENTED_EDGE ( 'NONE', *, *, #23649, .F. ) ;
#20104 = CARTESIAN_POINT ( 'NONE',  ( 11.90854556226686789, -40.05525454449572464, -74.83297477053821467 ) ) ;
#20105 = AXIS2_PLACEMENT_3D ( 'NONE', #26047, #16450, #36055 ) ;
#20106 = DIRECTION ( 'NONE',  ( -1.000000000000000000, 0.000000000000000000, -0.000000000000000000 ) ) ;
#20107 = APPLICATION_PROTOCOL_DEFINITION ( 'draft international standard', 'automotive_design', 1998, #18697 ) ;
#20108 = DIRECTION ( 'NONE',  ( 0.000000000000000000, -0.3641605752528292994, 0.9313361774523356562 ) ) ;
#20109 = CARTESIAN_POINT ( 'NONE',  ( 70.67261647610648367, 31.00000000000000000, -24.00465245562410743 ) ) ;
#20110 = EDGE_CURVE ( 'NONE', #17062, #8370, #8702, .T. ) ;
#20111 = ORIENTED_EDGE ( 'NONE', *, *, #11978, .T. ) ;
#20112 = CARTESIAN_POINT ( 'NONE',  ( -31.59164309906361368, 31.00000000000000355, 4.115917706319392799 ) ) ;
#20113 = CARTESIAN_POINT ( 'NONE',  ( -21.91107887650263564, 40.00000000000000000, 64.54935342160338507 ) ) ;
#20114 = DIRECTION ( 'NONE',  ( -1.000000000000000000, -0.000000000000000000, -0.000000000000000000 ) ) ;
#20115 = CARTESIAN_POINT ( 'NONE',  ( 18.00000000000000355, 0.000000000000000000, 0.000000000000000000 ) ) ;
#20116 = ORIENTED_EDGE ( 'NONE', *, *, #11129, .F. ) ;
#20117 = DIRECTION ( 'NONE',  ( -1.000000000000000000, 0.000000000000000000, -0.000000000000000000 ) ) ;
#20118 = LINE ( 'NONE', #1716, #3475 ) ;
#20119 = AXIS2_PLACEMENT_3D ( 'NONE', #39203, #15919, #42486 ) ;
#20120 = ADVANCED_FACE ( 'NONE', ( #15928 ), #15504, .F. ) ;
#20121 = AXIS2_PLACEMENT_3D ( 'NONE', #8628, #15002, #38509 ) ;
#20122 = ORIENTED_EDGE ( 'NONE', *, *, #12191, .T. ) ;
#20123 = CARTESIAN_POINT ( 'NONE',  ( 25.16436199730139123, 40.00000000000000000, 51.02488717759543135 ) ) ;
#20124 = AXIS2_PLACEMENT_3D ( 'NONE', #16482, #3753, #3110 ) ;
#20125 = CARTESIAN_POINT ( 'NONE',  ( 5.384454397937118664, 0.000000000000000000, -4.484454397937119197 ) ) ;
#20126 = FACE_OUTER_BOUND ( 'NONE', #26920, .T. ) ;
#20127 = CIRCLE ( 'NONE', #37491, 116.0000000000000000 ) ;
#20128 = ORIENTED_EDGE ( 'NONE', *, *, #10418, .F. ) ;
#20129 = DIRECTION ( 'NONE',  ( -1.000000000000000000, 0.000000000000000000, 0.000000000000000000 ) ) ;
#20130 = AXIS2_PLACEMENT_3D ( 'NONE', #31260, #7678, #31676 ) ;
#20131 = CARTESIAN_POINT ( 'NONE',  ( 17.99999999999999645, -31.80866420683992857, 2.997093558041182160 ) ) ;
#20132 = ORIENTED_EDGE ( 'NONE', *, *, #13054, .T. ) ;
#20133 = LINE ( 'NONE', #16641, #2585 ) ;
#20134 = ORIENTED_EDGE ( 'NONE', *, *, #25814, .F. ) ;
#20135 = ADVANCED_FACE ( 'NONE', ( #22486 ), #38372, .F. ) ;
#20136 = EDGE_LOOP ( 'NONE', ( #5062, #23506, #35947, #19353 ) ) ;
#20137 = FACE_OUTER_BOUND ( 'NONE', #11422, .T. ) ;
#20138 = CARTESIAN_POINT ( 'NONE',  ( 24.72345498302141920, 31.00000000000000355, -91.84610802666480822 ) ) ;
#20139 = VERTEX_POINT ( 'NONE', #32477 ) ;
#20140 = CARTESIAN_POINT ( 'NONE',  ( 0.000000000000000000, -47.49120266317495975, 0.8606222198173691940 ) ) ;
#20141 = DIRECTION ( 'NONE',  ( 1.000000000000000000, 0.000000000000000000, 0.000000000000000000 ) ) ;
#20142 = EDGE_CURVE ( 'NONE', #32971, #17775, #9132, .T. ) ;
#20143 = DIRECTION ( 'NONE',  ( -1.058513553088275437E-16, -1.000000000000000000, 8.813324511995299047E-17 ) ) ;
#20144 = ORIENTED_EDGE ( 'NONE', *, *, #19701, .F. ) ;
#20145 = CYLINDRICAL_SURFACE ( 'NONE', #20378, 24.99999999999999289 ) ;
#20146 = FACE_OUTER_BOUND ( 'NONE', #26284, .T. ) ;
#20147 = CIRCLE ( 'NONE', #7554, 11.00000000000000000 ) ;
#20148 = CIRCLE ( 'NONE', #6862, 20.00000000000000711 ) ;
#20150 = CARTESIAN_POINT ( 'NONE',  ( -9.000000000000005329, 0.000000000000000000, 14.91999999999999815 ) ) ;
#20149 = CYLINDRICAL_SURFACE ( 'NONE', #11339, 120.5010000000000190 ) ;
#20151 = DIRECTION ( 'NONE',  ( -1.000000000000000000, 0.000000000000000000, 0.000000000000000000 ) ) ;
#20152 = CIRCLE ( 'NONE', #1291, 2.500000000000002665 ) ;
#20153 = ORIENTED_EDGE ( 'NONE', *, *, #36812, .F. ) ;
#20154 = CARTESIAN_POINT ( 'NONE',  ( -40.10416666498607441, 31.00000000000000355, -2.617993869485698344 ) ) ;
#20155 = ADVANCED_FACE ( 'NONE', ( #8930 ), #31624, .F. ) ;
#20156 = EDGE_LOOP ( 'NONE', ( #5674, #29333, #28270, #15174 ) ) ;
#20157 = DIRECTION ( 'NONE',  ( 1.000000000000000000, -1.373900992973641868E-15, -6.546126324440886161E-16 ) ) ;
#20158 = ADVANCED_FACE ( 'NONE', ( #8490 ), #29016, .F. ) ;
#20159 = DIRECTION ( 'NONE',  ( 1.000000000000000000, -0.000000000000000000, -0.000000000000000000 ) ) ;
#20160 = VERTEX_POINT ( 'NONE', #12640 ) ;
#20161 = DIRECTION ( 'NONE',  ( 0.000000000000000000, 0.000000000000000000, 1.000000000000000000 ) ) ;
#20162 = CARTESIAN_POINT ( 'NONE',  ( 33.70925502316616473, 40.00000000000000000, 11.43906998022225707 ) ) ;
#20163 = CARTESIAN_POINT ( 'NONE',  ( 45.11287655886649617, 40.00000000000000000, -12.00022417491798521 ) ) ;
#20164 = ORIENTED_EDGE ( 'NONE', *, *, #29007, .F. ) ;
#20165 = ORIENTED_EDGE ( 'NONE', *, *, #37005, .F. ) ;
#20166 = DIRECTION ( 'NONE',  ( 0.000000000000000000, 0.000000000000000000, 1.000000000000000000 ) ) ;
#20167 = CYLINDRICAL_SURFACE ( 'NONE', #13783, 20.00000000000000355 ) ;
#20168 = CARTESIAN_POINT ( 'NONE',  ( 17.99999999999999645, -51.27532863109303918, -99.79535634195178773 ) ) ;
#20169 = EDGE_CURVE ( 'NONE', #16736, #4843, #20148, .T. ) ;
#20170 = EDGE_LOOP ( 'NONE', ( #3295, #24775, #40706, #9074 ) ) ;
#20171 = DIRECTION ( 'NONE',  ( -1.000000000000000000, -0.000000000000000000, -0.000000000000000000 ) ) ;
#20172 = ORIENTED_EDGE ( 'NONE', *, *, #34298, .F. ) ;
#20173 = DIRECTION ( 'NONE',  ( -1.000000000000000000, 0.000000000000000000, 0.000000000000000000 ) ) ;
#20174 = CARTESIAN_POINT ( 'NONE',  ( -6.199999999999993960, -19.19999999999999218, 2.351321854362917684E-15 ) ) ;
#20175 = VERTEX_POINT ( 'NONE', #34891 ) ;
#20176 = AXIS2_PLACEMENT_3D ( 'NONE', #40458, #40245, #7088 ) ;
#20177 = AXIS2_PLACEMENT_3D ( 'NONE', #5162, #18755, #32424 ) ;
#20178 = FACE_OUTER_BOUND ( 'NONE', #17613, .T. ) ;
#20179 = CARTESIAN_POINT ( 'NONE',  ( 0.000000000000000000, 0.000000000000000000, 0.000000000000000000 ) ) ;
#20180 = EDGE_LOOP ( 'NONE', ( #24785, #19855, #29231, #12919 ) ) ;
#20181 = DIRECTION ( 'NONE',  ( 0.000000000000000000, 0.9574220383620042352, 0.2886919473396248326 ) ) ;
#20182 = ORIENTED_EDGE ( 'NONE', *, *, #6550, .F. ) ;
#20183 = AXIS2_PLACEMENT_3D ( 'NONE', #1985, #25995, #9385 ) ;
#20184 = DIRECTION ( 'NONE',  ( 0.000000000000000000, 0.000000000000000000, -1.000000000000000000 ) ) ;
#20185 = EDGE_CURVE ( 'NONE', #37133, #4351, #4042, .T. ) ;
#20186 = VERTEX_POINT ( 'NONE', #12437 ) ;
#20188 = ORIENTED_EDGE ( 'NONE', *, *, #5891, .F. ) ;
#20187 = CARTESIAN_POINT ( 'NONE',  ( 17.99999999999999645, 0.000000000000000000, 0.000000000000000000 ) ) ;
#20189 = CARTESIAN_POINT ( 'NONE',  ( 65.23019871247133494, 31.00000000000000000, 17.57949444736449252 ) ) ;
#20190 = ADVANCED_FACE ( 'NONE', ( #35727 ), #39008, .T. ) ;
#20191 = ORIENTED_EDGE ( 'NONE', *, *, #630, .F. ) ;
#20192 = CARTESIAN_POINT ( 'NONE',  ( -3.333333333333332149, -2.694301256218264218, -3.300726591567082036 ) ) ;
#20193 = ORIENTED_EDGE ( 'NONE', *, *, #11346, .T. ) ;
#20194 = CARTESIAN_POINT ( 'NONE',  ( 17.99999999999999645, 2.007101075700415738, -31.43498920425966858 ) ) ;
#20195 = ORIENTED_EDGE ( 'NONE', *, *, #8397, .F. ) ;
#20196 = CARTESIAN_POINT ( 'NONE',  ( 56.68048384767583769, 39.99999999999999289, -64.44707192207098956 ) ) ;
#20198 = DIRECTION ( 'NONE',  ( 0.000000000000000000, 0.2486898871648553500, -0.9685831611286310761 ) ) ;
#20197 = LINE ( 'NONE', #39976, #30772 ) ;
#20199 = DIRECTION ( 'NONE',  ( 0.000000000000000000, 0.000000000000000000, 1.000000000000000000 ) ) ;
#20200 = VERTEX_POINT ( 'NONE', #5853 ) ;
#20201 = CARTESIAN_POINT ( 'NONE',  ( 9.000000000000001776, 44.25018368420781911, -27.31155879685132604 ) ) ;
#20202 = ORIENTED_EDGE ( 'NONE', *, *, #11413, .F. ) ;
#20203 = ORIENTED_EDGE ( 'NONE', *, *, #21847, .F. ) ;
#20204 = CYLINDRICAL_SURFACE ( 'NONE', #32370, 47.49900000000000233 ) ;
#20205 = EDGE_CURVE ( 'NONE', #9994, #31505, #18364, .T. ) ;
#20206 = CARTESIAN_POINT ( 'NONE',  ( 23.52215716829092074, 31.00000000000000355, -69.29398394448777765 ) ) ;
#20207 = EDGE_CURVE ( 'NONE', #15962, #20548, #22279, .T. ) ;
#20208 = DIRECTION ( 'NONE',  ( 0.000000000000000000, 0.000000000000000000, 1.000000000000000000 ) ) ;
#20209 = AXIS2_PLACEMENT_3D ( 'NONE', #13888, #37188, #10811 ) ;
#20210 = ORIENTED_EDGE ( 'NONE', *, *, #11833, .F. ) ;
#20211 = ADVANCED_FACE ( 'NONE', ( #25953 ), #19209, .T. ) ;
#20212 = EDGE_CURVE ( 'NONE', #9730, #34509, #27099, .T. ) ;
#20213 = ADVANCED_FACE ( 'NONE', ( #1720 ), #28591, .F. ) ;
#20214 = DIRECTION ( 'NONE',  ( 0.000000000000000000, 0.9213119778704114138, 0.3888241754733244848 ) ) ;
#20215 = VERTEX_POINT ( 'NONE', #19007 ) ;
#20216 = DIRECTION ( 'NONE',  ( -1.000000000000000000, -0.000000000000000000, -0.000000000000000000 ) ) ;
#20217 = LINE ( 'NONE', #33270, #29716 ) ;
#20218 = DIRECTION ( 'NONE',  ( -1.000000000000000000, -0.000000000000000000, -0.000000000000000000 ) ) ;
#20219 = DIRECTION ( 'NONE',  ( 0.000000000000000000, -0.9048270524660235736, 0.4257792915650641663 ) ) ;
#20220 = ORIENTED_EDGE ( 'NONE', *, *, #4554, .F. ) ;
#20221 = DIRECTION ( 'NONE',  ( -1.000000000000000000, -0.000000000000000000, -0.000000000000000000 ) ) ;
#20222 = VERTEX_POINT ( 'NONE', #20282 ) ;
#20223 = FACE_OUTER_BOUND ( 'NONE', #2851, .T. ) ;
#20224 = DIRECTION ( 'NONE',  ( 0.000000000000000000, 0.000000000000000000, 1.000000000000000000 ) ) ;
#20225 = CARTESIAN_POINT ( 'NONE',  ( 0.000000000000000000, 1.178949249685212974, -2.042000000000001148 ) ) ;
#20226 = EDGE_LOOP ( 'NONE', ( #3984, #4830, #5306, #26849 ) ) ;
#20227 = VERTEX_POINT ( 'NONE', #33342 ) ;
#20228 = DIRECTION ( 'NONE',  ( -1.000000000000000000, -0.000000000000000000, -0.000000000000000000 ) ) ;
#20229 = DIRECTION ( 'NONE',  ( -1.000000000000000000, -0.000000000000000000, 0.000000000000000000 ) ) ;
#20230 = EDGE_CURVE ( 'NONE', #11400, #34568, #40065, .T. ) ;
#20231 = CARTESIAN_POINT ( 'NONE',  ( 0.000000000000000000, 13.57797752207971520, -33.34124362422459598 ) ) ;
#20232 = AXIS2_PLACEMENT_3D ( 'NONE', #9945, #12812, #6454 ) ;
#20234 = ORIENTED_EDGE ( 'NONE', *, *, #42958, .F. ) ;
#20233 = FACE_OUTER_BOUND ( 'NONE', #7729, .T. ) ;
#20235 = CARTESIAN_POINT ( 'NONE',  ( 27.04960320298028620, 31.00000000000000355, -23.64836272119223892 ) ) ;
#20236 = EDGE_CURVE ( 'NONE', #8971, #33317, #13725, .T. ) ;
#20237 = AXIS2_PLACEMENT_3D ( 'NONE', #5700, #22124, #42753 ) ;
#20238 = DIRECTION ( 'NONE',  ( -3.996523416598930318E-16, 2.658563593772947863E-15, 1.000000000000000000 ) ) ;
#20240 = ORIENTED_EDGE ( 'NONE', *, *, #1542, .T. ) ;
#20239 = CARTESIAN_POINT ( 'NONE',  ( -104.2750351721725650, 31.00000000000000000, -4.541977405098627685 ) ) ;
#20241 = ORIENTED_EDGE ( 'NONE', *, *, #22301, .T. ) ;
#20242 = CARTESIAN_POINT ( 'NONE',  ( 0.000000000000000000, 0.000000000000000000, 0.000000000000000000 ) ) ;
#20243 = DIRECTION ( 'NONE',  ( 0.000000000000000000, 0.000000000000000000, 1.000000000000000000 ) ) ;
#20244 = CARTESIAN_POINT ( 'NONE',  ( -49.80813925210025417, 40.00000000000000000, -17.00652635548005520 ) ) ;
#20245 = CARTESIAN_POINT ( 'NONE',  ( 17.99999999999999645, -96.25468616236712194, 72.49500943364458294 ) ) ;
#20246 = DIRECTION ( 'NONE',  ( 0.000000000000000000, 1.000000000000000000, 0.000000000000000000 ) ) ;
#20247 = ORIENTED_EDGE ( 'NONE', *, *, #29007, .T. ) ;
#20248 = DIRECTION ( 'NONE',  ( 0.000000000000000000, 0.000000000000000000, 1.000000000000000000 ) ) ;
#20249 = VERTEX_POINT ( 'NONE', #2977 ) ;
#20250 = FACE_OUTER_BOUND ( 'NONE', #27654, .T. ) ;
#20251 = DIRECTION ( 'NONE',  ( 1.000000000000000000, -0.000000000000000000, 0.000000000000000000 ) ) ;
#20252 = CARTESIAN_POINT ( 'NONE',  ( -33.94102792873697183, 31.00000000000000355, -38.68473105385043453 ) ) ;
#20253 = ADVANCED_FACE ( 'NONE', ( #33546 ), #39434, .T. ) ;
#20254 = DIRECTION ( 'NONE',  ( 0.000000000000000000, 0.000000000000000000, 1.000000000000000000 ) ) ;
#20255 = ORIENTED_EDGE ( 'NONE', *, *, #5843, .F. ) ;
#20256 = EDGE_CURVE ( 'NONE', #12073, #1655, #36168, .T. ) ;
#20257 = ADVANCED_FACE ( 'NONE', ( #30289 ), #26381, .F. ) ;
#20258 = EDGE_CURVE ( 'NONE', #18, #16718, #21573, .T. ) ;
#20259 = LINE ( 'NONE', #30263, #17798 ) ;
#20260 = ORIENTED_EDGE ( 'NONE', *, *, #33949, .F. ) ;
#20261 = CARTESIAN_POINT ( 'NONE',  ( 95.10416666600561086, 31.00000000000000000, 6.217735451873073416 ) ) ;
#20262 = VECTOR ( 'NONE', #29523, 1000.000000000000000 ) ;
#20263 = AXIS2_PLACEMENT_3D ( 'NONE', #25039, #34800, #8188 ) ;
#20264 = EDGE_LOOP ( 'NONE', ( #16122, #17507, #20255, #36764 ) ) ;
#20265 = CIRCLE ( 'NONE', #4200, 31.49899999999999878 ) ;
#20266 = DIRECTION ( 'NONE',  ( 0.000000000000000000, 0.000000000000000000, 1.000000000000000000 ) ) ;
#20267 = CARTESIAN_POINT ( 'NONE',  ( 24.27443280711675300, 31.00000000000000355, -71.15176282235542260 ) ) ;
#20268 = CARTESIAN_POINT ( 'NONE',  ( 4.991138515316659863, 40.00000000000000000, -74.59332054773635434 ) ) ;
#20269 = AXIS2_PLACEMENT_3D ( 'NONE', #6114, #13336, #42737 ) ;
#20270 = EDGE_CURVE ( 'NONE', #39541, #18421, #26386, .T. ) ;
#20271 = CARTESIAN_POINT ( 'NONE',  ( 0.000000000000000000, -23.21237537461669120, -109.7700237000594541 ) ) ;
#20272 = VERTEX_POINT ( 'NONE', #12851 ) ;
#20273 = VERTEX_POINT ( 'NONE', #16581 ) ;
#20274 = CARTESIAN_POINT ( 'NONE',  ( 17.99999999999999645, -119.7318547011700502, -13.59315897125848238 ) ) ;
#20275 = DIRECTION ( 'NONE',  ( 0.000000000000000000, 0.000000000000000000, 1.000000000000000000 ) ) ;
#20277 = ORIENTED_EDGE ( 'NONE', *, *, #36157, .T. ) ;
#20276 = DIRECTION ( 'NONE',  ( 0.000000000000000000, 0.000000000000000000, 1.000000000000000000 ) ) ;
#20278 = CYLINDRICAL_SURFACE ( 'NONE', #28861, 120.5010000000000190 ) ;
#20279 = ORIENTED_EDGE ( 'NONE', *, *, #322, .T. ) ;
#20280 = CARTESIAN_POINT ( 'NONE',  ( 17.99999999999999645, -27.24480646643618442, 15.80846360676574669 ) ) ;
#20281 = CARTESIAN_POINT ( 'NONE',  ( -28.35539204363714205, 40.00000000000000000, 83.52787551312086123 ) ) ;
#20282 = CARTESIAN_POINT ( 'NONE',  ( 0.000000000000000000, -64.58410930313456788, -101.7319213743688664 ) ) ;
#20283 = ORIENTED_EDGE ( 'NONE', *, *, #17623, .T. ) ;
#20284 = AXIS2_PLACEMENT_3D ( 'NONE', #29459, #42722, #9800 ) ;
#20285 = CARTESIAN_POINT ( 'NONE',  ( 17.99999999999999645, 29.02167576844106023, 108.3790330702170621 ) ) ;
#20286 = DIRECTION ( 'NONE',  ( -1.000000000000000000, -0.000000000000000000, 0.000000000000000000 ) ) ;
#20287 = VERTEX_POINT ( 'NONE', #22694 ) ;
#20288 = VECTOR ( 'NONE', #32663, 1000.000000000000000 ) ;
#20289 = CARTESIAN_POINT ( 'NONE',  ( 17.99999999999999645, 120.3696465864706227, 5.624871700596478341 ) ) ;
#20290 = ORIENTED_EDGE ( 'NONE', *, *, #27078, .F. ) ;
#20291 = DIRECTION ( 'NONE',  ( -1.000000000000000000, 0.000000000000000000, 0.000000000000000000 ) ) ;
#20293 = ORIENTED_EDGE ( 'NONE', *, *, #37718, .F. ) ;
#20292 = CIRCLE ( 'NONE', #2806, 116.0000000000000000 ) ;
#20294 = CARTESIAN_POINT ( 'NONE',  ( 24.91045342551595354, 40.00000000000000000, 12.31387362277309272 ) ) ;
#20295 = CARTESIAN_POINT ( 'NONE',  ( 17.99999999999999645, 0.000000000000000000, 0.000000000000000000 ) ) ;
#20296 = VECTOR ( 'NONE', #41272, 1000.000000000000000 ) ;
#20297 = CYLINDRICAL_SURFACE ( 'NONE', #6721, 22.99999999999987921 ) ;
#20298 = CIRCLE ( 'NONE', #10510, 139.4999999999992610 ) ;
#20299 = DIRECTION ( 'NONE',  ( -1.000000000000000000, 0.000000000000000000, 0.000000000000000000 ) ) ;
#20300 = CIRCLE ( 'NONE', #32100, 2.649999999999971934 ) ;
#20301 = DIRECTION ( 'NONE',  ( 0.000000000000000000, 0.3612416661871471479, 0.9324722294043581439 ) ) ;
#20302 = VERTEX_POINT ( 'NONE', #2769 ) ;
#20304 = DIRECTION ( 'NONE',  ( 0.000000000000000000, 0.000000000000000000, 1.000000000000000000 ) ) ;
#20303 = FACE_OUTER_BOUND ( 'NONE', #22918, .T. ) ;
#20305 = VERTEX_POINT ( 'NONE', #140 ) ;
#20306 = LINE ( 'NONE', #40318, #23180 ) ;
#20307 = CARTESIAN_POINT ( 'NONE',  ( 17.99999999999999645, 0.000000000000000000, 0.000000000000000000 ) ) ;
#20308 = ORIENTED_EDGE ( 'NONE', *, *, #33563, .T. ) ;
#20309 = DIRECTION ( 'NONE',  ( -1.000000000000000000, 0.000000000000000000, -0.000000000000000000 ) ) ;
#20310 = EDGE_CURVE ( 'NONE', #18884, #12306, #29646, .T. ) ;
#20311 = DIRECTION ( 'NONE',  ( -1.000000000000000000, 0.000000000000000000, 0.000000000000000000 ) ) ;
#20312 = EDGE_CURVE ( 'NONE', #6385, #16988, #42925, .T. ) ;
#20313 = CARTESIAN_POINT ( 'NONE',  ( -10.00000000000000178, 0.000000000000000000, 0.000000000000000000 ) ) ;
#20314 = CARTESIAN_POINT ( 'NONE',  ( 63.32575250126041055, 31.00000000000000000, 16.95471465585521997 ) ) ;
#20315 = VERTEX_POINT ( 'NONE', #26588 ) ;
#20316 = CARTESIAN_POINT ( 'NONE',  ( 41.46880187713386334, 31.00000000000000355, 24.04226233541373858 ) ) ;
#20317 = CARTESIAN_POINT ( 'NONE',  ( 21.49215960483416410, 40.00000000000000000, -80.26604385357094884 ) ) ;
#20318 = CIRCLE ( 'NONE', #18250, 13.60000000000000142 ) ;
#20319 = EDGE_CURVE ( 'NONE', #22974, #6539, #16132, .T. ) ;
#20320 = AXIS2_PLACEMENT_3D ( 'NONE', #28508, #14761, #28709 ) ;
#20321 = CARTESIAN_POINT ( 'NONE',  ( 8.999999999999998224, 115.6826031496112392, 8.575274253897841703 ) ) ;
#20322 = AXIS2_PLACEMENT_3D ( 'NONE', #33179, #26862, #17890 ) ;
#20323 = EDGE_CURVE ( 'NONE', #21384, #1441, #29434, .T. ) ;
#20324 = DIRECTION ( 'NONE',  ( 0.000000000000000000, 0.000000000000000000, 1.000000000000000000 ) ) ;
#20325 = VECTOR ( 'NONE', #26531, 1000.000000000000000 ) ;
#20326 = ORIENTED_EDGE ( 'NONE', *, *, #40197, .T. ) ;
#20327 = FACE_BOUND ( 'NONE', #23997, .T. ) ;
#20328 = DIRECTION ( 'NONE',  ( -1.000000000000000000, -0.000000000000000000, -0.000000000000000000 ) ) ;
#20329 = ORIENTED_EDGE ( 'NONE', *, *, #28780, .F. ) ;
#20330 = CARTESIAN_POINT ( 'NONE',  ( 52.68777711438346500, 40.00000000000000000, 17.88338314711659294 ) ) ;
#20331 = CARTESIAN_POINT ( 'NONE',  ( 1.039096088315723056E-14, -6.912265343809663812E-14, -26.00000000000000355 ) ) ;
#20332 = LINE ( 'NONE', #415, #35408 ) ;
#20333 = CIRCLE ( 'NONE', #31459, 59.00000000000000711 ) ;
#20334 = ORIENTED_EDGE ( 'NONE', *, *, #37251, .F. ) ;
#20335 = FACE_OUTER_BOUND ( 'NONE', #9189, .T. ) ;
#20336 = DIRECTION ( 'NONE',  ( 0.000000000000000000, 0.000000000000000000, 1.000000000000000000 ) ) ;
#20337 = VERTEX_POINT ( 'NONE', #36377 ) ;
#20338 = DIRECTION ( 'NONE',  ( 0.000000000000000000, 0.000000000000000000, 1.000000000000000000 ) ) ;
#20339 = ORIENTED_EDGE ( 'NONE', *, *, #42519, .T. ) ;
#20340 = ORIENTED_EDGE ( 'NONE', *, *, #18398, .F. ) ;
#20341 = DIRECTION ( 'NONE',  ( -1.000000000000000000, 0.000000000000000000, 0.000000000000000000 ) ) ;
#20342 = CARTESIAN_POINT ( 'NONE',  ( -86.84058463553202500, 31.00000000000000711, 29.36381822872188607 ) ) ;
#20343 = VERTEX_POINT ( 'NONE', #23552 ) ;
#20344 = CYLINDRICAL_SURFACE ( 'NONE', #30081, 31.49899999999999878 ) ;
#20345 = CARTESIAN_POINT ( 'NONE',  ( 0.000000000000000000, -51.85248208264520287, 3.914090171286016773 ) ) ;
#20346 = CARTESIAN_POINT ( 'NONE',  ( 0.000000000000000000, -111.1352304691226607, -15.40237066878709449 ) ) ;
#20347 = ORIENTED_EDGE ( 'NONE', *, *, #4541, .F. ) ;
#20348 = CARTESIAN_POINT ( 'NONE',  ( 0.000000000000000000, 0.000000000000000000, 0.000000000000000000 ) ) ;
#20349 = AXIS2_PLACEMENT_3D ( 'NONE', #10337, #913, #3744 ) ;
#20350 = AXIS2_PLACEMENT_3D ( 'NONE', #20032, #26978, #33940 ) ;
#20351 = CARTESIAN_POINT ( 'NONE',  ( 0.000000000000000000, -31.94619804602753277, -16.59639811537390131 ) ) ;
#20353 = DIRECTION ( 'NONE',  ( -0.9470131699890049770, -3.405258028344997528E-16, -0.3211947320043963550 ) ) ;
#20352 = DIRECTION ( 'NONE',  ( -1.000000000000000000, -0.000000000000000000, -0.000000000000000000 ) ) ;
#20354 = CIRCLE ( 'NONE', #5679, 36.00000000000000000 ) ;
#20355 = ADVANCED_FACE ( 'NONE', ( #36817 ), #9776, .F. ) ;
#20356 = FACE_OUTER_BOUND ( 'NONE', #29475, .T. ) ;
#20357 = EDGE_CURVE ( 'NONE', #15352, #9771, #4788, .T. ) ;
#20358 = ORIENTED_EDGE ( 'NONE', *, *, #4888, .T. ) ;
#20359 = DIRECTION ( 'NONE',  ( 0.7071067811865437980, 0.000000000000000000, -0.7071067811865512365 ) ) ;
#20360 = CARTESIAN_POINT ( 'NONE',  ( 34.98270738856093232, 31.00000000000000355, 4.602016392115340970 ) ) ;
#20361 = VERTEX_POINT ( 'NONE', #6074 ) ;
#20362 = CARTESIAN_POINT ( 'NONE',  ( 18.00000000000000355, 0.000000000000000000, 0.000000000000000000 ) ) ;
#20363 = DIRECTION ( 'NONE',  ( 1.000000000000000000, 0.000000000000000000, 0.000000000000000000 ) ) ;
#20364 = ORIENTED_EDGE ( 'NONE', *, *, #22670, .F. ) ;
#20365 = CYLINDRICAL_SURFACE ( 'NONE', #2028, 36.00000000000000000 ) ;
#20366 = CARTESIAN_POINT ( 'NONE',  ( -13.51098712749246467, 40.00000000000000000, -50.41620372279128048 ) ) ;
#20367 = CARTESIAN_POINT ( 'NONE',  ( 45.87644943786595064, 40.00000000000000000, 12.37342411884007731 ) ) ;
#20368 = EDGE_CURVE ( 'NONE', #6747, #24285, #12471, .T. ) ;
#20369 = VERTEX_POINT ( 'NONE', #36589 ) ;
#20370 = CARTESIAN_POINT ( 'NONE',  ( 18.00000000000000355, 36.34385289850631295, -29.77717097092038756 ) ) ;
#20371 = EDGE_CURVE ( 'NONE', #19640, #33033, #19631, .T. ) ;
#20372 = DIRECTION ( 'NONE',  ( 0.000000000000000000, 0.000000000000000000, 1.000000000000000000 ) ) ;
#20373 = DIRECTION ( 'NONE',  ( -1.000000000000000000, -0.000000000000000000, 0.000000000000000000 ) ) ;
#20374 = VERTEX_POINT ( 'NONE', #13939 ) ;
#20375 = CARTESIAN_POINT ( 'NONE',  ( -16.73417733071809721, 40.00000000000000000, -12.82953315787133519 ) ) ;
#20376 = ORIENTED_EDGE ( 'NONE', *, *, #33693, .F. ) ;
#20377 = CARTESIAN_POINT ( 'NONE',  ( -1.600000000000000089, -12.75000000000000000, 0.000000000000000000 ) ) ;
#20378 = AXIS2_PLACEMENT_3D ( 'NONE', #33404, #3487, #21870 ) ;
#20379 = CARTESIAN_POINT ( 'NONE',  ( 1.734723475976807094E-15, 4.618802153517012954, -0.4999999999999995559 ) ) ;
#20380 = VECTOR ( 'NONE', #7457, 1000.000000000000000 ) ;
#20381 = ORIENTED_EDGE ( 'NONE', *, *, #34059, .F. ) ;
#20382 = CYLINDRICAL_SURFACE ( 'NONE', #3286, 64.99999999999998579 ) ;
#20383 = CIRCLE ( 'NONE', #11306, 20.00000000000000711 ) ;
#20384 = DIRECTION ( 'NONE',  ( 0.000000000000000000, 1.000000000000000000, 1.224646799147353207E-16 ) ) ;
#20385 = ORIENTED_EDGE ( 'NONE', *, *, #28256, .T. ) ;
#20386 = CARTESIAN_POINT ( 'NONE',  ( 17.99999999999999645, -24.22031524826050841, 109.5520369638036584 ) ) ;
#20387 = ORIENTED_EDGE ( 'NONE', *, *, #20014, .T. ) ;
#20388 = CARTESIAN_POINT ( 'NONE',  ( 0.000000000000000000, 0.000000000000000000, 0.000000000000000000 ) ) ;
#20389 = ADVANCED_FACE ( 'NONE', ( #30515 ), #30927, .T. ) ;
#20390 = ADVANCED_FACE ( 'NONE', ( #24204 ), #33983, .F. ) ;
#20391 = VECTOR ( 'NONE', #41929, 1000.000000000000114 ) ;
#20392 = EDGE_LOOP ( 'NONE', ( #39666, #13085, #35192, #3881 ) ) ;
#20394 = EDGE_LOOP ( 'NONE', ( #41022, #41518, #16367, #20144 ) ) ;
#20393 = DIRECTION ( 'NONE',  ( 3.996523416598993920E-16, 2.658563593772947074E-15, 1.000000000000000000 ) ) ;
#20395 = CARTESIAN_POINT ( 'NONE',  ( -61.89998375878432313, 31.00000000000000711, 3.952486745199417673 ) ) ;
#20397 = EDGE_CURVE ( 'NONE', #11355, #23147, #14564, .T. ) ;
#20396 = ORIENTED_EDGE ( 'NONE', *, *, #34512, .F. ) ;
#20398 = CARTESIAN_POINT ( 'NONE',  ( -2.000000000000002665, -3.464101615137770374, -3.142992957459237680 ) ) ;
#20399 = ORIENTED_EDGE ( 'NONE', *, *, #52, .T. ) ;
#20400 = CARTESIAN_POINT ( 'NONE',  ( 0.000000000000000000, -13.00789606333398218, -115.2683592318616235 ) ) ;
#20401 = PRODUCT_DEFINITION_SHAPE ( 'NONE', 'NONE',  #3027 ) ;
#20402 = ORIENTED_EDGE ( 'NONE', *, *, #4930, .F. ) ;
#20403 = CARTESIAN_POINT ( 'NONE',  ( -81.90010630563853056, 40.00000000000000711, 5.248159452637418454 ) ) ;
#20405 = DIRECTION ( 'NONE',  ( -1.000000000000000000, 0.000000000000000000, 0.000000000000000000 ) ) ;
#20404 = CARTESIAN_POINT ( 'NONE',  ( 17.99999999999999645, 30.71634675606053833, 8.790889055186667633 ) ) ;
#20406 = CARTESIAN_POINT ( 'NONE',  ( 2.500000000000000000, 2.357898499370431722, -2.818925648462311528E-15 ) ) ;
#20407 = ORIENTED_EDGE ( 'NONE', *, *, #8340, .T. ) ;
#20408 = CARTESIAN_POINT ( 'NONE',  ( 17.99999999999999645, 82.63181128086846172, -81.41243003646886223 ) ) ;
#20409 = EDGE_CURVE ( 'NONE', #29751, #39905, #15963, .T. ) ;
#20410 = ORIENTED_EDGE ( 'NONE', *, *, #21536, .F. ) ;
#20411 = AXIS2_PLACEMENT_3D ( 'NONE', #17252, #27467, #30744 ) ;
#20412 = DIRECTION ( 'NONE',  ( 0.000000000000000000, -0.8747630845319559478, -0.4845508703326597000 ) ) ;
#20413 = DIRECTION ( 'NONE',  ( -1.000000000000000000, -0.000000000000000000, 0.000000000000000000 ) ) ;
#20414 = CIRCLE ( 'NONE', #23897, 59.00000000000000711 ) ;
#20415 = CARTESIAN_POINT ( 'NONE',  ( -80.23695839127151430, 31.00000000000000711, 39.56677620416681407 ) ) ;
#20416 = CARTESIAN_POINT ( 'NONE',  ( 17.99999999999999645, 0.000000000000000000, 0.000000000000000000 ) ) ;
#20417 = EDGE_LOOP ( 'NONE', ( #33492, #29920, #31347, #30960 ) ) ;
#20418 = CIRCLE ( 'NONE', #1562, 0.4000000000000001887 ) ;
#20419 = CARTESIAN_POINT ( 'NONE',  ( -10.00000000000000178, 0.000000000000000000, -12.59999999999999964 ) ) ;
#20420 = EDGE_CURVE ( 'NONE', #14987, #28874, #27676, .T. ) ;
#20421 = AXIS2_PLACEMENT_3D ( 'NONE', #1963, #12036, #21874 ) ;
#20422 = VERTEX_POINT ( 'NONE', #11093 ) ;
#20423 = CARTESIAN_POINT ( 'NONE',  ( 4.211140560182196957, 2.431303136016536470, -3.745885042887433514 ) ) ;
#20424 = EDGE_CURVE ( 'NONE', #41658, #35069, #1013, .T. ) ;
#20425 = CARTESIAN_POINT ( 'NONE',  ( 17.99999999999999645, 0.000000000000000000, 0.000000000000000000 ) ) ;
#20426 = SURFACE_SIDE_STYLE ('',( #726 ) ) ;
#20427 = EDGE_CURVE ( 'NONE', #19378, #6343, #6209, .T. ) ;
#20428 = CARTESIAN_POINT ( 'NONE',  ( -58.65872368235312706, -12.05525454449572109, -38.66963954070958209 ) ) ;
#20429 = EDGE_LOOP ( 'NONE', ( #26946, #37347, #30651, #14689 ) ) ;
#20430 = DIRECTION ( 'NONE',  ( -1.000000000000000000, -0.000000000000000000, -0.000000000000000000 ) ) ;
#20431 = VERTEX_POINT ( 'NONE', #11300 ) ;
#20432 = PLANE ( 'NONE',  #35346 ) ;
#20433 = CARTESIAN_POINT ( 'NONE',  ( 0.000000000000000000, 23.85344185397197947, 113.5209818126991621 ) ) ;
#20434 = CARTESIAN_POINT ( 'NONE',  ( 0.000000000000000000, -50.95304419620816816, -10.38206564895716255 ) ) ;
#20435 = VERTEX_POINT ( 'NONE', #7139 ) ;
#20436 = ORIENTED_EDGE ( 'NONE', *, *, #28137, .F. ) ;
#20437 = DIRECTION ( 'NONE',  ( 3.996523416598930318E-16, -2.658563593772947863E-15, -1.000000000000000000 ) ) ;
#20438 = LINE ( 'NONE', #10809, #22838 ) ;
#20439 = AXIS2_PLACEMENT_3D ( 'NONE', #7816, #5186, #25303 ) ;
#20440 = CYLINDRICAL_SURFACE ( 'NONE', #6917, 120.5010000000000190 ) ;
#20442 = VERTEX_POINT ( 'NONE', #21373 ) ;
#20441 = CYLINDRICAL_SURFACE ( 'NONE', #3385, 59.00000000000000000 ) ;
#20443 = CARTESIAN_POINT ( 'NONE',  ( 33.88265278290064941, 31.00000000000000355, 16.77599488388065652 ) ) ;
#20444 = EDGE_CURVE ( 'NONE', #17801, #4036, #27509, .T. ) ;
#20445 = FACE_OUTER_BOUND ( 'NONE', #1793, .T. ) ;
#20446 = PRODUCT_DEFINITION ( 'UNKNOWN', '', #26098, #22503 ) ;
#20447 = AXIS2_PLACEMENT_3D ( 'NONE', #1891, #15259, #14594 ) ;
#20449 = VERTEX_POINT ( 'NONE', #14363 ) ;
#20448 = DIRECTION ( 'NONE',  ( 0.000000000000000000, 0.000000000000000000, 1.000000000000000000 ) ) ;
#20450 = EDGE_LOOP ( 'NONE', ( #43118, #28414, #23646, #32321 ) ) ;
#20451 = CARTESIAN_POINT ( 'NONE',  ( 17.99999999999999645, 120.2856157092987957, -7.201503623195590009 ) ) ;
#20452 = LINE ( 'NONE', #40465, #28752 ) ;
#20454 = CARTESIAN_POINT ( 'NONE',  ( -50.71442127988192539, 40.00000000000000000, -13.67646662467582352 ) ) ;
#20453 = AXIS2_PLACEMENT_3D ( 'NONE', #164, #3658, #17257 ) ;
#20455 = CARTESIAN_POINT ( 'NONE',  ( 0.000000000000000000, 0.000000000000000000, 0.000000000000000000 ) ) ;
#20456 = PRODUCT_DEFINITION_CONTEXT ( 'detailed design', #7795, 'design' ) ;
#20457 = FACE_OUTER_BOUND ( 'NONE', #1163, .T. ) ;
#20458 = ORIENTED_EDGE ( 'NONE', *, *, #37223, .F. ) ;
#20459 = DIRECTION ( 'NONE',  ( 1.000000000000000000, 0.000000000000000000, 0.000000000000000000 ) ) ;
#20460 = EDGE_CURVE ( 'NONE', #34731, #37525, #14154, .T. ) ;
#20461 = ORIENTED_EDGE ( 'NONE', *, *, #2146, .T. ) ;
#20462 = ADVANCED_FACE ( 'NONE', ( #40946 ), #31155, .T. ) ;
#20463 = DIRECTION ( 'NONE',  ( -1.000000000000000000, -0.000000000000000000, -0.000000000000000000 ) ) ;
#20464 = DIRECTION ( 'NONE',  ( -1.000000000000000000, -0.000000000000000000, 0.000000000000000000 ) ) ;
#20465 = CARTESIAN_POINT ( 'NONE',  ( 8.201713468707295007, 31.00000000000000355, -62.30543997111072940 ) ) ;
#20466 = FACE_OUTER_BOUND ( 'NONE', #26412, .T. ) ;
#20467 = EDGE_LOOP ( 'NONE', ( #35159, #25358, #22776, #27595 ) ) ;
#20468 = CARTESIAN_POINT ( 'NONE',  ( 0.000000000000000000, 0.000000000000000000, 0.000000000000000000 ) ) ;
#20469 = EDGE_LOOP ( 'NONE', ( #34120, #17949, #26480, #20399 ) ) ;
#20470 = ADVANCED_FACE ( 'NONE', ( #27445, #7792 ), #1243, .F. ) ;
#20471 = CIRCLE ( 'NONE', #10661, 20.00000000000000355 ) ;
#20472 = CARTESIAN_POINT ( 'NONE',  ( 19.04566582976364941, 40.00000000000000000, -14.62000746238684989 ) ) ;
#20473 = ORIENTED_EDGE ( 'NONE', *, *, #18344, .T. ) ;
#20474 = CARTESIAN_POINT ( 'NONE',  ( 17.99999999999999645, 41.62036691425679180, -113.0850832732710529 ) ) ;
#20475 = ADVANCED_FACE ( 'NONE', ( #21152 ), #1450, .F. ) ;
#20476 = LINE ( 'NONE', #27428, #27603 ) ;
#20477 = CARTESIAN_POINT ( 'NONE',  ( 39.32569335900156204, 31.00000000000000355, 68.32161714268157482 ) ) ;
#20478 = CARTESIAN_POINT ( 'NONE',  ( 58.79931003850258975, 40.00000000000000000, 51.72161244498203558 ) ) ;
#20479 = DIRECTION ( 'NONE',  ( 1.000000000000000000, 0.000000000000000000, 0.000000000000000000 ) ) ;
#20480 = PRESENTATION_LAYER_ASSIGNMENT (  '', '', ( #19081 ) ) ;
#20481 = ORIENTED_EDGE ( 'NONE', *, *, #3159, .T. ) ;
#20482 = DIRECTION ( 'NONE',  ( 0.000000000000000000, -0.7980172272802448230, 0.6026346363792492999 ) ) ;
#20483 = ORIENTED_EDGE ( 'NONE', *, *, #25551, .T. ) ;
#20484 = CIRCLE ( 'NONE', #194, 59.00000000000001421 ) ;
#20485 = CARTESIAN_POINT ( 'NONE',  ( 0.000000000000000000, -32.49609705003715732, 15.49205204337262920 ) ) ;
#20486 = PLANE ( 'NONE',  #26848 ) ;
#20488 = ORIENTED_EDGE ( 'NONE', *, *, #5591, .F. ) ;
#20487 = DIRECTION ( 'NONE',  ( -1.000000000000000000, -0.000000000000000000, -0.000000000000000000 ) ) ;
#20489 = CARTESIAN_POINT ( 'NONE',  ( 17.99999999999999645, -105.3681574666266414, 38.54638589714855357 ) ) ;
#20490 = ORIENTED_EDGE ( 'NONE', *, *, #13196, .T. ) ;
#20491 = CARTESIAN_POINT ( 'NONE',  ( 4.000000000000000000, -2.309401076758516691, -0.4999999999999995559 ) ) ;
#20492 = VECTOR ( 'NONE', #39121, 1000.000000000000000 ) ;
#20493 = CARTESIAN_POINT ( 'NONE',  ( -22.78857244739539212, 40.00000000000000000, 85.10612709700112077 ) ) ;
#20494 = CYLINDRICAL_SURFACE ( 'NONE', #616, 116.0000000000000000 ) ;
#20495 = EDGE_LOOP ( 'NONE', ( #32434, #35745, #16933, #34188 ) ) ;
#20496 = ADVANCED_FACE ( 'NONE', ( #37031 ), #20494, .F. ) ;
#20497 = CARTESIAN_POINT ( 'NONE',  ( 0.000000000000000000, -38.92705108641711576, -27.21837053747839263 ) ) ;
#20498 = EDGE_CURVE ( 'NONE', #2185, #29068, #39614, .T. ) ;
#20499 = CARTESIAN_POINT ( 'NONE',  ( 0.000000000000000000, 0.000000000000000000, -4.694516984716113228 ) ) ;
#20500 = EDGE_CURVE ( 'NONE', #40959, #24696, #10391, .T. ) ;
#20501 = EDGE_CURVE ( 'NONE', #14470, #10268, #22232, .T. ) ;
#20502 = CIRCLE ( 'NONE', #18427, 51.99999999999999289 ) ;
#20503 = ORIENTED_EDGE ( 'NONE', *, *, #13219, .T. ) ;
#20504 = CIRCLE ( 'NONE', #13512, 20.00000000000000355 ) ;
#20505 = ORIENTED_EDGE ( 'NONE', *, *, #8448, .F. ) ;
#20506 = DIRECTION ( 'NONE',  ( -3.996523416598930318E-16, 2.658563593772947863E-15, 1.000000000000000000 ) ) ;
#20507 = VERTEX_POINT ( 'NONE', #35476 ) ;
#20508 = CARTESIAN_POINT ( 'NONE',  ( 26.10672890669277990, 40.00000000000000000, 8.893381768402427667 ) ) ;
#20509 = DIRECTION ( 'NONE',  ( 0.000000000000000000, 0.000000000000000000, 1.000000000000000000 ) ) ;
#20510 = DIRECTION ( 'NONE',  ( 0.000000000000000000, 0.000000000000000000, 1.000000000000000000 ) ) ;
#20511 = DIRECTION ( 'NONE',  ( 0.000000000000000000, 0.000000000000000000, 1.000000000000000000 ) ) ;
#20512 = CARTESIAN_POINT ( 'NONE',  ( 17.99999999999999645, 30.78424799127067502, 6.672111855473287001 ) ) ;
#20513 = VERTEX_POINT ( 'NONE', #18528 ) ;
#20515 = CARTESIAN_POINT ( 'NONE',  ( 9.000000000000001776, 40.47821179127761582, -32.64221760512715775 ) ) ;
#20514 = DIRECTION ( 'NONE',  ( 1.000000000000000000, -0.000000000000000000, -0.000000000000000000 ) ) ;
#20516 = EDGE_LOOP ( 'NONE', ( #24179, #22335, #14392, #28632 ) ) ;
#20517 = DIRECTION ( 'NONE',  ( 0.000000000000000000, 0.000000000000000000, 1.000000000000000000 ) ) ;
#20518 = CARTESIAN_POINT ( 'NONE',  ( -5.732510072307491988, 31.00000000000000355, -21.37570426403446078 ) ) ;
#20519 = ORIENTED_EDGE ( 'NONE', *, *, #12188, .T. ) ;
#20520 = DIRECTION ( 'NONE',  ( 0.000000000000000000, 0.000000000000000000, 1.000000000000000000 ) ) ;
#20521 = CARTESIAN_POINT ( 'NONE',  ( 0.000000000000000000, 21.55123232222630492, -118.5581519187670096 ) ) ;
#20522 = CIRCLE ( 'NONE', #26075, 116.0000000000000000 ) ;
#20523 = ITEM_DEFINED_TRANSFORMATION ( 'NONE', 'NONE', #3017,  #13552 ) ;
#20524 = DIRECTION ( 'NONE',  ( -1.000000000000000000, 0.000000000000000000, 0.000000000000000000 ) ) ;
#20525 = CARTESIAN_POINT ( 'NONE',  ( -35.92146702467432817, 31.00000000000000355, -62.19081021767443218 ) ) ;
#20526 = CIRCLE ( 'NONE', #28174, 120.5010000000000332 ) ;
#20527 = EDGE_LOOP ( 'NONE', ( #10704, #20835, #27838, #31280 ) ) ;
#20528 = CARTESIAN_POINT ( 'NONE',  ( 11.72132095739929625, 31.00000000000000355, -43.45763713126748229 ) ) ;
#20529 = AXIS2_PLACEMENT_3D ( 'NONE', #28825, #32085, #22094 ) ;
#20530 = CARTESIAN_POINT ( 'NONE',  ( 5.399612364985509672, 40.00000000000000000, -82.60416666586320389 ) ) ;
#20531 = DIRECTION ( 'NONE',  ( -1.000000000000000000, -0.000000000000000000, -0.000000000000000000 ) ) ;
#20532 = CARTESIAN_POINT ( 'NONE',  ( -125.9999999999995026, 1.156432136281054424E-12, 369.6955262170048400 ) ) ;
#20533 = ORIENTED_EDGE ( 'NONE', *, *, #26092, .T. ) ;
#20534 = CARTESIAN_POINT ( 'NONE',  ( 17.99999999999999645, -107.2703412112692689, -32.88383143828572486 ) ) ;
#20535 = CYLINDRICAL_SURFACE ( 'NONE', #20965, 116.0000000000000000 ) ;
#20536 = PRODUCT_DEFINITION_FORMATION_WITH_SPECIFIED_SOURCE ( 'ANY', '', #30486, .NOT_KNOWN. ) ;
#20537 = VECTOR ( 'NONE', #40805, 1000.000000000000000 ) ;
#20538 = VERTEX_POINT ( 'NONE', #4956 ) ;
#20539 = CARTESIAN_POINT ( 'NONE',  ( -49.88601606984090608, 40.00000000000000000, -6.565487524765669214 ) ) ;
#20540 = FACE_OUTER_BOUND ( 'NONE', #38767, .T. ) ;
#20541 = AXIS2_PLACEMENT_3D ( 'NONE', #4594, #11383, #37757 ) ;
#20542 = DIRECTION ( 'NONE',  ( 0.000000000000000000, 0.000000000000000000, 1.000000000000000000 ) ) ;
#20543 = ORIENTED_EDGE ( 'NONE', *, *, #32909, .T. ) ;
#20544 = CARTESIAN_POINT ( 'NONE',  ( -106.4195705685756081, 106.4195705685752529, 6.999999999999998224 ) ) ;
#20545 = CARTESIAN_POINT ( 'NONE',  ( 103.7695705685734708, 106.4195705685780382, 10.00000000000025224 ) ) ;
#20546 = EDGE_CURVE ( 'NONE', #16328, #23341, #32684, .T. ) ;
#20547 = ADVANCED_FACE ( 'NONE', ( #42012 ), #35683, .T. ) ;
#20548 = VERTEX_POINT ( 'NONE', #24858 ) ;
#20549 = CARTESIAN_POINT ( 'NONE',  ( 0.000000000000000000, 0.000000000000000000, 0.000000000000000000 ) ) ;
#20550 = EDGE_LOOP ( 'NONE', ( #856, #37221, #3221, #29725 ) ) ;
#20551 = VECTOR ( 'NONE', #22443, 1000.000000000000000 ) ;
#20552 = EDGE_CURVE ( 'NONE', #1020, #1396, #38748, .T. ) ;
#20553 = CARTESIAN_POINT ( 'NONE',  ( 17.99999999999999645, -17.33727698085246871, 110.8498592715972961 ) ) ;
#20554 = ORIENTED_EDGE ( 'NONE', *, *, #7351, .T. ) ;
#20555 = AXIS2_PLACEMENT_3D ( 'NONE', #36046, #32780, #19299 ) ;
#20556 = DIRECTION ( 'NONE',  ( -1.000000000000000000, -0.000000000000000000, 0.000000000000000000 ) ) ;
#20557 = DIRECTION ( 'NONE',  ( -1.000000000000000000, 0.000000000000000000, 0.000000000000000000 ) ) ;
#20558 = ORIENTED_EDGE ( 'NONE', *, *, #19449, .T. ) ;
#20559 = CIRCLE ( 'NONE', #40679, 116.0000000000000000 ) ;
#20560 = DIRECTION ( 'NONE',  ( -1.000000000000000000, -0.000000000000000000, 0.000000000000000000 ) ) ;
#20561 = CARTESIAN_POINT ( 'NONE',  ( 17.99999999999999645, -86.84764344323014029, 76.89919913989720612 ) ) ;
#20562 = ORIENTED_EDGE ( 'NONE', *, *, #29362, .T. ) ;
#20563 = DIRECTION ( 'NONE',  ( -1.000000000000000000, 0.000000000000000000, 0.000000000000000000 ) ) ;
#20564 = DIRECTION ( 'NONE',  ( -0.8660254037844373753, 0.5000000000000021094, 0.000000000000000000 ) ) ;
#20565 = EDGE_CURVE ( 'NONE', #39739, #37953, #13902, .T. ) ;
#20567 = DIRECTION ( 'NONE',  ( 0.000000000000000000, 0.000000000000000000, 1.000000000000000000 ) ) ;
#20566 = DIRECTION ( 'NONE',  ( -1.000000000000000000, -0.000000000000000000, 0.000000000000000000 ) ) ;
#20568 = FACE_OUTER_BOUND ( 'NONE', #39477, .T. ) ;
#20569 = VERTEX_POINT ( 'NONE', #22008 ) ;
#20570 = CARTESIAN_POINT ( 'NONE',  ( -4.943662031389838196E-16, 18.00000000000000355, 1.828353205453026285E-14 ) ) ;
#20571 = CARTESIAN_POINT ( 'NONE',  ( 18.00000000000000355, -13.85708833599937861, -45.43276465116677798 ) ) ;
#20572 = CARTESIAN_POINT ( 'NONE',  ( -32.63632984357925437, 31.00000000000000355, -25.02932899672474676 ) ) ;
#20573 = ORIENTED_EDGE ( 'NONE', *, *, #31027, .F. ) ;
#20574 = DIRECTION ( 'NONE',  ( -1.000000000000000000, 0.000000000000000000, -0.000000000000000000 ) ) ;
#20575 = CARTESIAN_POINT ( 'NONE',  ( 17.99999999999999645, 14.84191762912315049, 27.78316904333131276 ) ) ;
#20576 = ORIENTED_EDGE ( 'NONE', *, *, #6280, .T. ) ;
#20577 = DIRECTION ( 'NONE',  ( -1.000000000000000000, -0.000000000000000000, -0.000000000000000000 ) ) ;
#20578 = EDGE_CURVE ( 'NONE', #42589, #13405, #11098, .T. ) ;
#20579 = CARTESIAN_POINT ( 'NONE',  ( 51.69409438402072965, 40.00000000000000000, -17.56033928829605273 ) ) ;
#20580 = CIRCLE ( 'NONE', #31017, 64.99999999999997158 ) ;
#20581 = CARTESIAN_POINT ( 'NONE',  ( 3.148395399070833545, 40.00000000000000000, 49.39975974384547897 ) ) ;
#20582 = CIRCLE ( 'NONE', #42820, 58.99999999999999289 ) ;
#20583 = AXIS2_PLACEMENT_3D ( 'NONE', #28792, #12209, #38568 ) ;
#20584 = ORIENTED_EDGE ( 'NONE', *, *, #17077, .F. ) ;
#20585 = DIRECTION ( 'NONE',  ( 1.000000000000000000, -0.000000000000000000, -0.000000000000000000 ) ) ;
#20586 = VECTOR ( 'NONE', #3699, 1000.000000000000000 ) ;
#20587 = CARTESIAN_POINT ( 'NONE',  ( -10.00000000000000000, 0.000000000000000000, 0.000000000000000000 ) ) ;
#20588 = MECHANICAL_DESIGN_GEOMETRIC_PRESENTATION_REPRESENTATION (  '', ( #18521 ), #35185 ) ;
#20589 = CARTESIAN_POINT ( 'NONE',  ( 18.00000000000000355, 3.840921266749842022, 47.34345070675171030 ) ) ;
#20590 = CIRCLE ( 'NONE', #16403, 59.00000000000000000 ) ;
#20591 = ORIENTED_EDGE ( 'NONE', *, *, #21061, .T. ) ;
#20592 = CARTESIAN_POINT ( 'NONE',  ( -14.11622541012940601, 40.00000000000000000, -16.08312669853564358 ) ) ;
#20593 = EDGE_LOOP ( 'NONE', ( #24924, #9959, #31617, #16557 ) ) ;
#20594 = DIRECTION ( 'NONE',  ( 0.000000000000000000, 0.000000000000000000, 1.000000000000000000 ) ) ;
#20595 = CARTESIAN_POINT ( 'NONE',  ( 8.999999999999998224, 101.1403355683153933, -56.80345518653383152 ) ) ;
#20596 = ORIENTED_EDGE ( 'NONE', *, *, #5303, .T. ) ;
#20597 = DIRECTION ( 'NONE',  ( -1.000000000000000000, -0.000000000000000000, 0.000000000000000000 ) ) ;
#20598 = ADVANCED_FACE ( 'NONE', ( #25709 ), #25279, .F. ) ;
#20599 = CARTESIAN_POINT ( 'NONE',  ( 17.99999999999999645, 0.000000000000000000, 0.000000000000000000 ) ) ;
#20600 = ORIENTED_EDGE ( 'NONE', *, *, #33326, .T. ) ;
#20601 = DIRECTION ( 'NONE',  ( 1.000000000000000000, 0.000000000000000000, 0.000000000000000000 ) ) ;
#20602 = EDGE_LOOP ( 'NONE', ( #37645, #21501, #28321, #1391 ) ) ;
#20603 = CARTESIAN_POINT ( 'NONE',  ( 0.000000000000000000, -87.92975456462855277, -69.68953103478244770 ) ) ;
#20604 = AXIS2_PLACEMENT_3D ( 'NONE', #22997, #22561, #26024 ) ;
#20605 = ORIENTED_EDGE ( 'NONE', *, *, #4244, .F. ) ;
#20607 = EDGE_LOOP ( 'NONE', ( #25508, #8461, #31537, #32490 ) ) ;
#20606 = FACE_OUTER_BOUND ( 'NONE', #36248, .T. ) ;
#20608 = CARTESIAN_POINT ( 'NONE',  ( 57.47007747236072817, 31.00000000000000000, -33.06854485811727784 ) ) ;
#20609 = ORIENTED_EDGE ( 'NONE', *, *, #28713, .T. ) ;
#20610 = CARTESIAN_POINT ( 'NONE',  ( 0.000000000000000000, -41.33768078145568836, 104.3046912715539918 ) ) ;
#20611 = ADVANCED_FACE ( 'NONE', ( #15455 ), #14803, .F. ) ;
#20612 = VECTOR ( 'NONE', #11157, 1000.000000000000000 ) ;
#20613 = VECTOR ( 'NONE', #28619, 1000.000000000000000 ) ;
#20614 = ORIENTED_EDGE ( 'NONE', *, *, #13876, .T. ) ;
#20615 = ADVANCED_FACE ( 'NONE', ( #28750 ), #18959, .F. ) ;
#20616 = CIRCLE ( 'NONE', #31743, 58.99999999999998579 ) ;
#20617 = CARTESIAN_POINT ( 'NONE',  ( 18.00000000000000355, -5.667686777401384823, -46.64153600743609474 ) ) ;
#20618 = ORIENTED_EDGE ( 'NONE', *, *, #8169, .F. ) ;
#20619 = CARTESIAN_POINT ( 'NONE',  ( -56.91377077966711084, 40.00000000000000000, -74.37798324515208037 ) ) ;
#20620 = AXIS2_PLACEMENT_3D ( 'NONE', #33673, #30425, #40426 ) ;
#20621 = EDGE_CURVE ( 'NONE', #16491, #16968, #43105, .T. ) ;
#20623 = CARTESIAN_POINT ( 'NONE',  ( 17.99999999999999645, 0.000000000000000000, 0.000000000000000000 ) ) ;
#20622 = DIRECTION ( 'NONE',  ( 0.000000000000000000, 0.000000000000000000, 1.000000000000000000 ) ) ;
#20624 = AXIS2_PLACEMENT_3D ( 'NONE', #33266, #40639, #36738 ) ;
#20625 = DIRECTION ( 'NONE',  ( -1.000000000000000000, -0.000000000000000000, 0.000000000000000000 ) ) ;
#20626 = ORIENTED_EDGE ( 'NONE', *, *, #588, .T. ) ;
#20627 = CARTESIAN_POINT ( 'NONE',  ( 17.99999999999999645, 10.40101730206529140, -120.0512800434970018 ) ) ;
#20628 = ORIENTED_EDGE ( 'NONE', *, *, #7879, .F. ) ;
#20629 =( LENGTH_UNIT ( ) NAMED_UNIT ( * ) SI_UNIT ( .MILLI., .METRE. ) );
#20630 = AXIS2_PLACEMENT_3D ( 'NONE', #36264, #13396, #16238 ) ;
#20631 = CARTESIAN_POINT ( 'NONE',  ( 18.00000000000000355, 0.000000000000000000, 0.000000000000000000 ) ) ;
#20632 = CARTESIAN_POINT ( 'NONE',  ( 0.000000000000000000, 0.000000000000000000, 0.000000000000000000 ) ) ;
#20633 = CARTESIAN_POINT ( 'NONE',  ( 84.24376206367318787, 31.00000000000000000, -11.10575268747775901 ) ) ;
#20634 = LINE ( 'NONE', #27164, #35296 ) ;
#20635 = ORIENTED_EDGE ( 'NONE', *, *, #27809, .F. ) ;
#20636 = DIRECTION ( 'NONE',  ( 1.000000000000000000, 0.000000000000000000, 0.000000000000000000 ) ) ;
#20637 = EDGE_CURVE ( 'NONE', #35175, #3463, #27828, .T. ) ;
#20638 =( REPRESENTATION_RELATIONSHIP ('NONE','NONE', #330, #13509 ) REPRESENTATION_RELATIONSHIP_WITH_TRANSFORMATION ( #19875 )SHAPE_REPRESENTATION_RELATIONSHIP( ) );
#20639 = VERTEX_POINT ( 'NONE', #42226 ) ;
#20640 = CARTESIAN_POINT ( 'NONE',  ( 3.510273485745307731, 2.827716139362654424, -3.610536846335885564 ) ) ;
#20641 = CARTESIAN_POINT ( 'NONE',  ( 17.99999999999999645, 117.6086855750638165, -26.24286718911983485 ) ) ;
#20643 = DIRECTION ( 'NONE',  ( 0.000000000000000000, 0.1253332335642974305, 0.9921147013144787641 ) ) ;
#20642 = AXIS2_PLACEMENT_3D ( 'NONE', #24994, #1801, #14933 ) ;
#20644 = DIRECTION ( 'NONE',  ( -1.000000000000000000, 0.000000000000000000, 0.000000000000000000 ) ) ;
#20645 = VECTOR ( 'NONE', #4748, 1000.000000000000000 ) ;
#20646 = VECTOR ( 'NONE', #201, 1000.000000000000000 ) ;
#20647 = CIRCLE ( 'NONE', #3166, 130.0000000000000000 ) ;
#20648 = VERTEX_POINT ( 'NONE', #12386 ) ;
#20649 = DIRECTION ( 'NONE',  ( -1.000000000000000000, 0.000000000000000000, 0.000000000000000000 ) ) ;
#20650 = ORIENTED_EDGE ( 'NONE', *, *, #19268, .F. ) ;
#20651 = CARTESIAN_POINT ( 'NONE',  ( 17.99999999999999645, -23.87611429743677505, 20.54551452399611478 ) ) ;
#20652 = STYLED_ITEM ( 'NONE', ( #28872 ), #13589 ) ;
#20653 = AXIS2_PLACEMENT_3D ( 'NONE', #2064, #15623, #11490 ) ;
#20654 = AXIS2_PLACEMENT_3D ( 'NONE', #27827, #37818, #5094 ) ;
#20655 = DIRECTION ( 'NONE',  ( -1.000000000000000000, -0.000000000000000000, 0.000000000000000000 ) ) ;
#20656 = VECTOR ( 'NONE', #30812, 1000.000000000000000 ) ;
#20657 = CARTESIAN_POINT ( 'NONE',  ( 17.99999999999999645, 116.4607004671432406, -30.94182036827089632 ) ) ;
#20658 = EDGE_LOOP ( 'NONE', ( #33256, #22285, #29495, #22404 ) ) ;
#20659 = VERTEX_POINT ( 'NONE', #41367 ) ;
#20660 = DIRECTION ( 'NONE',  ( -1.000000000000000000, 0.000000000000000000, 0.000000000000000000 ) ) ;
#20661 = EDGE_CURVE ( 'NONE', #28909, #16968, #34779, .T. ) ;
#20662 = DIRECTION ( 'NONE',  ( 3.996523416598930318E-16, -2.658563593772947863E-15, -1.000000000000000000 ) ) ;
#20663 = AXIS2_PLACEMENT_3D ( 'NONE', #27340, #7471, #24316 ) ;
#20664 = CARTESIAN_POINT ( 'NONE',  ( 17.99999999999999645, 0.000000000000000000, 0.000000000000000000 ) ) ;
#20666 = ORIENTED_EDGE ( 'NONE', *, *, #14034, .F. ) ;
#20665 = DIRECTION ( 'NONE',  ( 0.000000000000000000, 0.000000000000000000, 1.000000000000000000 ) ) ;
#20667 = CARTESIAN_POINT ( 'NONE',  ( -23.27229071023271700, 31.00000000000000355, 20.35677778009614869 ) ) ;
#20668 = FACE_OUTER_BOUND ( 'NONE', #12094, .T. ) ;
#20669 = EDGE_CURVE ( 'NONE', #18884, #16540, #13182, .T. ) ;
#20671 = VERTEX_POINT ( 'NONE', #15022 ) ;
#20670 = CARTESIAN_POINT ( 'NONE',  ( 0.000000000000000000, -115.0622509503831452, -14.72000021165260897 ) ) ;
#20672 = EDGE_LOOP ( 'NONE', ( #5446, #35733, #33638, #19086 ) ) ;
#20673 = DIRECTION ( 'NONE',  ( -1.000000000000000000, 0.000000000000000000, 0.000000000000000000 ) ) ;
#20674 = CARTESIAN_POINT ( 'NONE',  ( 3.148395399070833545, 40.00000000000000000, 49.39975974384547897 ) ) ;
#20675 = CIRCLE ( 'NONE', #31110, 59.00000000000000711 ) ;
#20676 = DIRECTION ( 'NONE',  ( 0.000000000000000000, 0.000000000000000000, 1.000000000000000000 ) ) ;
#20677 = AXIS2_PLACEMENT_3D ( 'NONE', #18126, #21614, #41171 ) ;
#20678 = DIRECTION ( 'NONE',  ( -1.000000000000000000, 0.000000000000000000, 0.000000000000000000 ) ) ;
#20680 = VERTEX_POINT ( 'NONE', #41598 ) ;
#20679 = AXIS2_PLACEMENT_3D ( 'NONE', #31383, #14607, #23995 ) ;
#20681 = FACE_OUTER_BOUND ( 'NONE', #459, .T. ) ;
#20682 = VECTOR ( 'NONE', #12573, 1000.000000000000000 ) ;
#20683 = VERTEX_POINT ( 'NONE', #21804 ) ;
#20684 = CARTESIAN_POINT ( 'NONE',  ( 9.000000000000001776, -6.854627147199504833, 115.7972974066013307 ) ) ;
#20685 = CARTESIAN_POINT ( 'NONE',  ( 17.99999999999999645, -91.51415974874549875, -64.91094698989387268 ) ) ;
#20686 = CIRCLE ( 'NONE', #27645, 120.5010000000000332 ) ;
#20687 = CARTESIAN_POINT ( 'NONE',  ( 37.24516168167158270, 31.00000000000000355, 42.45166511289891531 ) ) ;
#20688 = DIRECTION ( 'NONE',  ( 0.000000000000000000, -0.9822872507286865007, -0.1873813145857356199 ) ) ;
#20690 = VERTEX_POINT ( 'NONE', #25080 ) ;
#20689 = CIRCLE ( 'NONE', #1831, 120.5010000000000190 ) ;
#20692 = VECTOR ( 'NONE', #590, 1000.000000000000000 ) ;
#20691 = LINE ( 'NONE', #33316, #36510 ) ;
#20693 = ORIENTED_EDGE ( 'NONE', *, *, #18836, .T. ) ;
#20694 = CARTESIAN_POINT ( 'NONE',  ( 12.74197863150380883, 31.00000000000000355, 96.66318596537892915 ) ) ;
#20695 = EDGE_CURVE ( 'NONE', #14972, #23617, #40329, .T. ) ;
#20696 = ORIENTED_EDGE ( 'NONE', *, *, #5265, .T. ) ;
#20697 = CARTESIAN_POINT ( 'NONE',  ( -10.00000000000000000, 0.000000000000000000, 0.000000000000000000 ) ) ;
#20698 = EDGE_CURVE ( 'NONE', #5055, #16388, #4076, .T. ) ;
#20699 = CARTESIAN_POINT ( 'NONE',  ( 17.99999999999999645, -71.21168426767167148, 86.70160608319299911 ) ) ;
#20700 = CARTESIAN_POINT ( 'NONE',  ( -65.32047834223114080, 31.00000000000000711, -32.32491738443057017 ) ) ;
#20701 = CARTESIAN_POINT ( 'NONE',  ( -23.73339997550686675, 40.00000000000000000, -70.23208777907456124 ) ) ;
#20702 = VECTOR ( 'NONE', #33032, 1000.000000000000000 ) ;
#20703 = DIRECTION ( 'NONE',  ( 0.000000000000000000, 0.000000000000000000, 1.000000000000000000 ) ) ;
#20704 = VERTEX_POINT ( 'NONE', #23077 ) ;
#20705 = DIRECTION ( 'NONE',  ( 0.000000000000000000, 0.000000000000000000, 1.000000000000000000 ) ) ;
#20706 = ORIENTED_EDGE ( 'NONE', *, *, #25631, .T. ) ;
#20707 = DIRECTION ( 'NONE',  ( -1.000000000000000000, 0.000000000000000000, 0.000000000000000000 ) ) ;
#20708 = DIRECTION ( 'NONE',  ( -1.000000000000000000, -0.000000000000000000, -0.000000000000000000 ) ) ;
#20709 = AXIS2_PLACEMENT_3D ( 'NONE', #27438, #36810, #15015 ) ;
#20711 = ORIENTED_EDGE ( 'NONE', *, *, #5906, .T. ) ;
#20710 = LINE ( 'NONE', #33754, #23503 ) ;
#20712 = FACE_OUTER_BOUND ( 'NONE', #4919, .T. ) ;
#20713 = ORIENTED_EDGE ( 'NONE', *, *, #904, .F. ) ;
#20714 = CARTESIAN_POINT ( 'NONE',  ( 17.99999999999999645, 0.000000000000000000, 0.000000000000000000 ) ) ;
#20715 = ADVANCED_FACE ( 'NONE', ( #36532 ), #4817, .F. ) ;
#20716 = CARTESIAN_POINT ( 'NONE',  ( -11.47416535668642723, 40.00000000000000000, 87.14428777381637303 ) ) ;
#20717 = DIRECTION ( 'NONE',  ( 0.000000000000000000, 0.000000000000000000, 1.000000000000000000 ) ) ;
#20718 = AXIS2_PLACEMENT_3D ( 'NONE', #5480, #18193, #31889 ) ;
#20719 = ADVANCED_FACE ( 'NONE', ( #40014 ), #6441, .F. ) ;
#20720 = VERTEX_POINT ( 'NONE', #13237 ) ;
#20721 = CYLINDRICAL_SURFACE ( 'NONE', #42933, 20.00000000000000355 ) ;
#20722 = DIRECTION ( 'NONE',  ( -1.000000000000000000, 0.000000000000000000, 0.000000000000000000 ) ) ;
#20723 = CIRCLE ( 'NONE', #3237, 120.5010000000000332 ) ;
#20724 = ORIENTED_EDGE ( 'NONE', *, *, #16992, .T. ) ;
#20725 = AXIS2_PLACEMENT_3D ( 'NONE', #39020, #19219, #15092 ) ;
#20726 = ADVANCED_FACE ( 'NONE', ( #16520 ), #29594, .F. ) ;
#20727 = SURFACE_STYLE_FILL_AREA ( #1019 ) ;
#20728 = ORIENTED_EDGE ( 'NONE', *, *, #5044, .F. ) ;
#20729 = CARTESIAN_POINT ( 'NONE',  ( 0.000000000000000000, 0.000000000000000000, 0.000000000000000000 ) ) ;
#20730 = VERTEX_POINT ( 'NONE', #20231 ) ;
#20731 = CARTESIAN_POINT ( 'NONE',  ( -10.00000000000000000, 0.000000000000000000, 0.000000000000000000 ) ) ;
#20732 = DIRECTION ( 'NONE',  ( -1.000000000000000000, 0.000000000000000000, -0.000000000000000000 ) ) ;
#20733 = AXIS2_PLACEMENT_3D ( 'NONE', #21117, #30685, #759 ) ;
#20734 = EDGE_CURVE ( 'NONE', #12270, #13782, #17379, .T. ) ;
#20735 = CYLINDRICAL_SURFACE ( 'NONE', #15685, 2.799122904894268959 ) ;
#20736 = FACE_OUTER_BOUND ( 'NONE', #1591, .T. ) ;
#20737 = ORIENTED_EDGE ( 'NONE', *, *, #25060, .F. ) ;
#20739 = CARTESIAN_POINT ( 'NONE',  ( 17.99999999999999645, -9.484061862023704492, -30.03730300138991538 ) ) ;
#20738 = DIRECTION ( 'NONE',  ( 1.000000000000000000, 0.000000000000000000, 0.000000000000000000 ) ) ;
#20740 = EDGE_LOOP ( 'NONE', ( #17087, #37472, #28239, #13603 ) ) ;
#20741 = CARTESIAN_POINT ( 'NONE',  ( 4.000000000000000000, 2.309401076758515803, -0.4999999999999995559 ) ) ;
#20742 = CARTESIAN_POINT ( 'NONE',  ( -8.325335757348113930, 31.00000000000000355, -31.05587074991522201 ) ) ;
#20744 = ORIENTED_EDGE ( 'NONE', *, *, #10562, .T. ) ;
#20743 = AXIS2_PLACEMENT_3D ( 'NONE', #39158, #32637, #2712 ) ;
#20745 = CARTESIAN_POINT ( 'NONE',  ( -0.5999999999999996447, -12.75000000000000000, 0.000000000000000000 ) ) ;
#20746 = FACE_BOUND ( 'NONE', #39737, .T. ) ;
#20747 = AXIS2_PLACEMENT_3D ( 'NONE', #37339, #41031, #4378 ) ;
#20748 = ITEM_DEFINED_TRANSFORMATION ( 'NONE', 'NONE', #13548,  #13552 ) ;
#20749 = AXIS2_PLACEMENT_3D ( 'NONE', #29702, #19260, #6770 ) ;
#20750 = CYLINDRICAL_SURFACE ( 'NONE', #6521, 120.5010000000000190 ) ;
#20751 = CARTESIAN_POINT ( 'NONE',  ( -63.57631528421845957, 31.00000000000000711, -31.33741679916209222 ) ) ;
#20752 = CIRCLE ( 'NONE', #31840, 59.00000000000000000 ) ;
#20753 = VECTOR ( 'NONE', #22005, 1000.000000000000000 ) ;
#20754 = EDGE_CURVE ( 'NONE', #28770, #10324, #15874, .T. ) ;
#20755 = EDGE_CURVE ( 'NONE', #31163, #8980, #9673, .T. ) ;
#20756 = ORIENTED_EDGE ( 'NONE', *, *, #10874, .T. ) ;
#20758 = CARTESIAN_POINT ( 'NONE',  ( -32.60815990948594134, 31.00000000000000355, 24.92795611697640368 ) ) ;
#20757 = CIRCLE ( 'NONE', #10241, 52.00000000000000000 ) ;
#20759 = EDGE_CURVE ( 'NONE', #18280, #11061, #26413, .T. ) ;
#20760 = ADVANCED_FACE ( 'NONE', ( #6657 ), #19579, .F. ) ;
#20761 = CIRCLE ( 'NONE', #26306, 116.0000000000000000 ) ;
#20762 = CARTESIAN_POINT ( 'NONE',  ( 72.19657831791809599, 39.99999999999999289, -19.34484491892447622 ) ) ;
#20763 = CARTESIAN_POINT ( 'NONE',  ( -142.5000000000000284, 1.745121688784978386E-14, 6.999999999999998224 ) ) ;
#20764 = VECTOR ( 'NONE', #42767, 1000.000000000000000 ) ;
#20765 = CARTESIAN_POINT ( 'NONE',  ( 8.999999999999998224, -78.18175027177376535, -85.69488855493077040 ) ) ;
#20766 = DIRECTION ( 'NONE',  ( 0.000000000000000000, 0.000000000000000000, 1.000000000000000000 ) ) ;
#20768 = VERTEX_POINT ( 'NONE', #23280 ) ;
#20767 = DIRECTION ( 'NONE',  ( 1.000000000000000000, 0.000000000000000000, 0.000000000000000000 ) ) ;
#20769 = DIRECTION ( 'NONE',  ( 0.000000000000000000, 0.9574220383620042352, 0.2886919473396248881 ) ) ;
#20770 = LINE ( 'NONE', #34029, #23749 ) ;
#20771 = ORIENTED_EDGE ( 'NONE', *, *, #19653, .F. ) ;
#20772 = CARTESIAN_POINT ( 'NONE',  ( -59.40491426035100631, 40.00000000000000711, 7.833300799371349932 ) ) ;
#20773 = CARTESIAN_POINT ( 'NONE',  ( 18.00000000000000355, 0.000000000000000000, 0.000000000000000000 ) ) ;
#20774 = CARTESIAN_POINT ( 'NONE',  ( 0.000000000000000000, -114.1529630473446986, -38.59523323561551678 ) ) ;
#20775 = ORIENTED_EDGE ( 'NONE', *, *, #29769, .T. ) ;
#20776 = AXIS2_PLACEMENT_3D ( 'NONE', #30617, #26268, #39539 ) ;
#20777 = DIRECTION ( 'NONE',  ( 0.000000000000000000, 0.4817536741017163782, -0.8763066800438630288 ) ) ;
#20778 = DIRECTION ( 'NONE',  ( -1.000000000000000000, -0.000000000000000000, 0.000000000000000000 ) ) ;
#20779 = ORIENTED_EDGE ( 'NONE', *, *, #25180, .T. ) ;
#20780 = DIRECTION ( 'NONE',  ( 1.000000000000000000, -0.000000000000000000, 0.000000000000000000 ) ) ;
#20781 = ORIENTED_EDGE ( 'NONE', *, *, #19811, .F. ) ;
#20782 = CIRCLE ( 'NONE', #1915, 59.00000000000000711 ) ;
#20783 = AXIS2_PLACEMENT_3D ( 'NONE', #37086, #13558, #26855 ) ;
#20784 = EDGE_CURVE ( 'NONE', #27172, #18006, #36761, .T. ) ;
#20785 = CARTESIAN_POINT ( 'NONE',  ( -31.75000000000000711, 19.19999999999999574, 0.000000000000000000 ) ) ;
#20786 = ORIENTED_EDGE ( 'NONE', *, *, #4310, .T. ) ;
#20787 = AXIS2_PLACEMENT_3D ( 'NONE', #25475, #38950, #9281 ) ;
#20788 = DIRECTION ( 'NONE',  ( 0.000000000000000000, -0.7980172272802321665, -0.6026346363792660643 ) ) ;
#20789 = CARTESIAN_POINT ( 'NONE',  ( 17.99999999999999645, 54.09091620264722877, 102.6166301549519488 ) ) ;
#20790 = ORIENTED_EDGE ( 'NONE', *, *, #27901, .F. ) ;
#20791 = EDGE_CURVE ( 'NONE', #7422, #42093, #16739, .T. ) ;
#20792 = CARTESIAN_POINT ( 'NONE',  ( 17.99999999999999645, -41.62036691425604573, 113.0850832732712945 ) ) ;
#20793 = DIRECTION ( 'NONE',  ( -1.000000000000000000, 0.000000000000000000, 0.000000000000000000 ) ) ;
#20794 = ORIENTED_EDGE ( 'NONE', *, *, #5673, .F. ) ;
#20795 = FACE_OUTER_BOUND ( 'NONE', #38554, .T. ) ;
#20796 = VECTOR ( 'NONE', #3161, 1000.000000000000000 ) ;
#20797 = DIRECTION ( 'NONE',  ( 0.000000000000000000, 0.000000000000000000, 1.000000000000000000 ) ) ;
#20798 = DIRECTION ( 'NONE',  ( 0.000000000000000000, 0.000000000000000000, 1.000000000000000000 ) ) ;
#20799 = FACE_OUTER_BOUND ( 'NONE', #14940, .T. ) ;
#20800 = EDGE_LOOP ( 'NONE', ( #8755, #20744, #33297, #38854 ) ) ;
#20801 = CARTESIAN_POINT ( 'NONE',  ( 47.33767018637038859, -2.200000000000013056, 69.39124571101469030 ) ) ;
#20802 = CARTESIAN_POINT ( 'NONE',  ( 0.000000000000000000, 79.94368240339547071, -90.16373242487824768 ) ) ;
#20803 = CARTESIAN_POINT ( 'NONE',  ( 5.583751958424166162, 31.00000000000000355, -42.43436172917101601 ) ) ;
#20804 = ORIENTED_EDGE ( 'NONE', *, *, #35729, .T. ) ;
#20806 = CARTESIAN_POINT ( 'NONE',  ( 109.0695705685763244, -106.4195705685744855, 10.00000000000000000 ) ) ;
#20805 = CARTESIAN_POINT ( 'NONE',  ( 17.99999999999999645, 0.000000000000000000, 0.000000000000000000 ) ) ;
#20807 = DIRECTION ( 'NONE',  ( 0.000000000000000000, 0.000000000000000000, 1.000000000000000000 ) ) ;
#20808 = EDGE_CURVE ( 'NONE', #14470, #42813, #16686, .T. ) ;
#20809 = ORIENTED_EDGE ( 'NONE', *, *, #12562, .F. ) ;
#20810 = EDGE_CURVE ( 'NONE', #8390, #13064, #3386, .T. ) ;
#20811 = ADVANCED_FACE ( 'NONE', ( #3372 ), #30032, .F. ) ;
#20812 = DIRECTION ( 'NONE',  ( 0.000000000000000000, -0.7525707698561306946, -0.6585113790650474197 ) ) ;
#20813 = CARTESIAN_POINT ( 'NONE',  ( -24.21661388771557100, 40.00000000000000000, 41.94898165618241137 ) ) ;
#20814 = AXIS2_PLACEMENT_3D ( 'NONE', #39047, #1978, #5683 ) ;
#20815 = CARTESIAN_POINT ( 'NONE',  ( 3.665567271000699012, 40.00000000000000000, -54.59530427606813419 ) ) ;
#20816 = CIRCLE ( 'NONE', #20121, 116.0000000000000000 ) ;
#20817 = EDGE_CURVE ( 'NONE', #16988, #36583, #1345, .T. ) ;
#20818 = AXIS2_PLACEMENT_3D ( 'NONE', #12295, #2011, #39280 ) ;
#20819 = AXIS2_PLACEMENT_3D ( 'NONE', #39590, #20221, #36521 ) ;
#20820 = CARTESIAN_POINT ( 'NONE',  ( 17.99999999999999645, 0.000000000000000000, 0.000000000000000000 ) ) ;
#20821 = DIRECTION ( 'NONE',  ( 1.000000000000000000, 0.000000000000000000, 0.000000000000000000 ) ) ;
#20822 = AXIS2_PLACEMENT_3D ( 'NONE', #3470, #10474, #39687 ) ;
#20823 = ADVANCED_FACE ( 'NONE', ( #26112 ), #37175, .F. ) ;
#20824 = CARTESIAN_POINT ( 'NONE',  ( -10.00000000000000000, 0.000000000000000000, 0.000000000000000000 ) ) ;
#20825 = DIRECTION ( 'NONE',  ( -0.000000000000000000, -0.000000000000000000, -1.000000000000000000 ) ) ;
#20826 = EDGE_LOOP ( 'NONE', ( #9565, #31175, #35307, #24152 ) ) ;
#20827 = CARTESIAN_POINT ( 'NONE',  ( -18.63466726053507472, 40.00000000000000000, -9.179856479542758407 ) ) ;
#20828 = ORIENTED_EDGE ( 'NONE', *, *, #22930, .T. ) ;
#20829 = DIRECTION ( 'NONE',  ( 1.000000000000000000, 0.000000000000000000, 0.000000000000000000 ) ) ;
#20830 = CARTESIAN_POINT ( 'NONE',  ( 0.6448876103708359731, 4.246476118072354922, -0.2256878752776725616 ) ) ;
#20831 = ADVANCED_FACE ( 'NONE', ( #4237 ), #20440, .F. ) ;
#20832 = ORIENTED_EDGE ( 'NONE', *, *, #29109, .F. ) ;
#20833 = FACE_OUTER_BOUND ( 'NONE', #31308, .T. ) ;
#20834 = DIRECTION ( 'NONE',  ( 1.000000000000000000, 0.000000000000000000, 0.000000000000000000 ) ) ;
#20835 = ORIENTED_EDGE ( 'NONE', *, *, #444, .F. ) ;
#20836 = DIRECTION ( 'NONE',  ( 0.000000000000000000, 1.000000000000000000, 0.000000000000000000 ) ) ;
#20837 = ORIENTED_EDGE ( 'NONE', *, *, #2534, .F. ) ;
#20838 = DIRECTION ( 'NONE',  ( 0.000000000000000000, -0.9213119778704165208, 0.3888241754733123834 ) ) ;
#20839 = ORIENTED_EDGE ( 'NONE', *, *, #24981, .T. ) ;
#20841 = ORIENTED_EDGE ( 'NONE', *, *, #9429, .F. ) ;
#20840 = CARTESIAN_POINT ( 'NONE',  ( 0.000000000000000000, 34.78944633786291973, -9.257128253673256424 ) ) ;
#20842 = CARTESIAN_POINT ( 'NONE',  ( -71.72626536482266602, 31.00000000000000711, -9.557116936239163252 ) ) ;
#20843 = EDGE_LOOP ( 'NONE', ( #26612, #36416, #7604, #43038 ) ) ;
#20844 = CARTESIAN_POINT ( 'NONE',  ( -4.000000000000000000, 0.8730739991738342143, -3.223134629628428893 ) ) ;
#20845 = EDGE_CURVE ( 'NONE', #14556, #4975, #17171, .T. ) ;
#20846 = VECTOR ( 'NONE', #15306, 1000.000000000000114 ) ;
#20847 = AXIS2_PLACEMENT_3D ( 'NONE', #28383, #25127, #2342 ) ;
#20848 = EDGE_CURVE ( 'NONE', #18762, #19436, #10589, .T. ) ;
#20849 = CIRCLE ( 'NONE', #20119, 59.00000000000000000 ) ;
#20850 = ORIENTED_EDGE ( 'NONE', *, *, #31178, .T. ) ;
#20851 = CARTESIAN_POINT ( 'NONE',  ( 0.000000000000000000, 30.03615769709792005, -42.44795908868957923 ) ) ;
#20852 = ORIENTED_EDGE ( 'NONE', *, *, #19172, .F. ) ;
#20853 = ADVANCED_BREP_SHAPE_REPRESENTATION ( '', ( #27502, #13552 ), #1623 ) ;
#20854 = CARTESIAN_POINT ( 'NONE',  ( -91.90012763196534706, 40.00000000000000711, 5.898218105444796855 ) ) ;
#20855 = CIRCLE ( 'NONE', #32635, 20.00000000000000711 ) ;
#20857 = CARTESIAN_POINT ( 'NONE',  ( -5.384454397937118664, 6.702023979852544604E-16, -5.000000000000000000 ) ) ;
#20856 = CARTESIAN_POINT ( 'NONE',  ( -6.999999999999999112, 4.546351088565595293E-15, 0.000000000000000000 ) ) ;
#20858 = CARTESIAN_POINT ( 'NONE',  ( -10.00000000000000000, 0.000000000000000000, 0.000000000000000000 ) ) ;
#20859 = CARTESIAN_POINT ( 'NONE',  ( 0.000000000000000000, 6.854627147198713466, 115.7972974066013734 ) ) ;
#20860 = ORIENTED_EDGE ( 'NONE', *, *, #7317, .T. ) ;
#20861 = FACE_OUTER_BOUND ( 'NONE', #3620, .T. ) ;
#20862 = DIRECTION ( 'NONE',  ( 0.000000000000000000, 0.000000000000000000, -1.000000000000000000 ) ) ;
#20863 = CARTESIAN_POINT ( 'NONE',  ( 85.10416666585589951, 31.00000000000000000, 5.563236982362346872 ) ) ;
#20864 = DIRECTION ( 'NONE',  ( -1.000000000000000000, -0.000000000000000000, -0.000000000000000000 ) ) ;
#20865 = ORIENTED_EDGE ( 'NONE', *, *, #34848, .F. ) ;
#20866 = EDGE_CURVE ( 'NONE', #39191, #14740, #23922, .T. ) ;
#20867 = CARTESIAN_POINT ( 'NONE',  ( 24.91045342551595354, 40.00000000000000000, 12.31387362277309272 ) ) ;
#20868 = EDGE_LOOP ( 'NONE', ( #34557, #32111, #6980, #39013 ) ) ;
#20869 = ORIENTED_EDGE ( 'NONE', *, *, #40437, .F. ) ;
#20870 = CARTESIAN_POINT ( 'NONE',  ( 3.861362476283255685, 2.629030857715988656, -3.671615880910370500 ) ) ;
#20871 = CARTESIAN_POINT ( 'NONE',  ( 153.1499999999986414, 1.392576523351516607E-12, 9.999999999999960920 ) ) ;
#20872 = AXIS2_PLACEMENT_3D ( 'NONE', #28503, #2045, #34574 ) ;
#20873 = DIRECTION ( 'NONE',  ( 0.000000000000000000, 0.000000000000000000, 1.000000000000000000 ) ) ;
#20874 = CARTESIAN_POINT ( 'NONE',  ( 17.99999999999999645, -46.12538073176274622, -111.3235835452215952 ) ) ;
#20875 = AXIS2_PLACEMENT_3D ( 'NONE', #12739, #42159, #35202 ) ;
#20876 = ADVANCED_FACE ( 'NONE', ( #26966 ), #40242, .T. ) ;
#20877 = VERTEX_POINT ( 'NONE', #3578 ) ;
#20878 = DIRECTION ( 'NONE',  ( -1.000000000000000000, 0.000000000000000000, 0.000000000000000000 ) ) ;
#20879 = ORIENTED_EDGE ( 'NONE', *, *, #9698, .T. ) ;
#20880 = CARTESIAN_POINT ( 'NONE',  ( -2.841217984690893843E-16, 1.478917074864463474E-14, 1.999999999999980904 ) ) ;
#20881 = DIRECTION ( 'NONE',  ( 0.000000000000000000, 0.000000000000000000, -1.000000000000000000 ) ) ;
#20882 = EDGE_CURVE ( 'NONE', #33446, #2987, #18139, .T. ) ;
#20883 = CARTESIAN_POINT ( 'NONE',  ( 0.000000000000000000, -3.803237743092135581, 31.26855263151013276 ) ) ;
#20884 = EDGE_CURVE ( 'NONE', #17388, #30173, #42450, .T. ) ;
#20885 = DIRECTION ( 'NONE',  ( 0.000000000000000000, 0.000000000000000000, 1.000000000000000000 ) ) ;
#20886 = ORIENTED_EDGE ( 'NONE', *, *, #21505, .T. ) ;
#20887 = ORIENTED_EDGE ( 'NONE', *, *, #27096, .F. ) ;
#20888 = LINE ( 'NONE', #5108, #35628 ) ;
#20889 = CARTESIAN_POINT ( 'NONE',  ( -12.69999999999999929, 0.000000000000000000, 0.000000000000000000 ) ) ;
#20890 = CARTESIAN_POINT ( 'NONE',  ( 4.000000000000000888, -0.8578082829538523635, -3.433262215449808696 ) ) ;
#20891 = EDGE_LOOP ( 'NONE', ( #321, #43, #16311, #12568 ) ) ;
#20893 = ORIENTED_EDGE ( 'NONE', *, *, #24865, .F. ) ;
#20892 = DIRECTION ( 'NONE',  ( -1.000000000000000000, -0.000000000000000000, -0.000000000000000000 ) ) ;
#20894 = CARTESIAN_POINT ( 'NONE',  ( -17.88900094061790469, 31.00000000000000355, 36.12696699725170646 ) ) ;
#20895 = DIRECTION ( 'NONE',  ( -1.000000000000000000, -0.000000000000000000, -0.000000000000000000 ) ) ;
#20897 = ORIENTED_EDGE ( 'NONE', *, *, #15428, .T. ) ;
#20896 = CARTESIAN_POINT ( 'NONE',  ( 17.99999999999999645, 11.58753559615485251, 29.77419532459266449 ) ) ;
#20898 = ORIENTED_EDGE ( 'NONE', *, *, #15849, .F. ) ;
#20899 = CARTESIAN_POINT ( 'NONE',  ( 4.329677741076332964, 40.00000000000000000, -64.59417075179260337 ) ) ;
#20900 = VECTOR ( 'NONE', #25332, 1000.000000000000000 ) ;
#20901 = AXIS2_PLACEMENT_3D ( 'NONE', #26669, #2855, #12941 ) ;
#20902 = CARTESIAN_POINT ( 'NONE',  ( 0.000000000000000000, 57.40245293794667703, 96.40140491896650587 ) ) ;
#20903 = UNCERTAINTY_MEASURE_WITH_UNIT (LENGTH_MEASURE( 1.000000000000000082E-05 ), #36294, 'distance_accuracy_value', 'NONE');
#20904 = DIRECTION ( 'NONE',  ( -1.000000000000000000, -0.000000000000000000, 0.000000000000000000 ) ) ;
#20905 = VERTEX_POINT ( 'NONE', #11043 ) ;
#20906 = AXIS2_PLACEMENT_3D ( 'NONE', #7234, #36470, #20594 ) ;
#20907 = CARTESIAN_POINT ( 'NONE',  ( 17.99999999999999645, 31.17727234463848163, -111.7317219465816862 ) ) ;
#20908 = ORIENTED_EDGE ( 'NONE', *, *, #7153, .T. ) ;
#20909 =( REPRESENTATION_RELATIONSHIP ('NONE','NONE', #330, #10434 ) REPRESENTATION_RELATIONSHIP_WITH_TRANSFORMATION ( #3453 )SHAPE_REPRESENTATION_RELATIONSHIP( ) );
#20910 = CARTESIAN_POINT ( 'NONE',  ( 0.000000000000000000, -47.00885577955406802, -6.806061952192774989 ) ) ;
#20911 = DIRECTION ( 'NONE',  ( 0.000000000000000000, 0.000000000000000000, 1.000000000000000000 ) ) ;
#20912 = CARTESIAN_POINT ( 'NONE',  ( -44.33513214241411760, 31.00000000000000355, 38.89722855811361768 ) ) ;
#20913 = DIRECTION ( 'NONE',  ( 0.000000000000000000, 0.000000000000000000, 1.000000000000000000 ) ) ;
#20914 = VERTEX_POINT ( 'NONE', #27185 ) ;
#20915 = EDGE_CURVE ( 'NONE', #27491, #23539, #22298, .T. ) ;
#20916 = DIRECTION ( 'NONE',  ( -3.009274222672345096E-17, -1.000000000000000000, 2.455023325076454960E-18 ) ) ;
#20917 = EDGE_LOOP ( 'NONE', ( #352, #33079, #38012, #14524 ) ) ;
#20918 = CARTESIAN_POINT ( 'NONE',  ( -3.620280825866593055, 40.00000000000000000, 27.53105304817175636 ) ) ;
#20919 = ORIENTED_EDGE ( 'NONE', *, *, #34960, .T. ) ;
#20920 = DIRECTION ( 'NONE',  ( 0.000000000000000000, -0.8747630845319560589, -0.4845508703326597000 ) ) ;
#20921 = CARTESIAN_POINT ( 'NONE',  ( 6.600000000000001421, 7.044548050363292547E-15, 0.000000000000000000 ) ) ;
#20922 = CARTESIAN_POINT ( 'NONE',  ( 4.991138515316659863, 31.00000000000000355, -74.59332054773635434 ) ) ;
#20923 = CARTESIAN_POINT ( 'NONE',  ( -19.10382689932985656, 40.00000000000000000, -71.73905014343321795 ) ) ;
#20924 = FACE_OUTER_BOUND ( 'NONE', #36061, .T. ) ;
#20925 = EDGE_CURVE ( 'NONE', #34186, #36059, #30668, .T. ) ;
#20926 = VERTEX_POINT ( 'NONE', #14308 ) ;
#20927 = DIRECTION ( 'NONE',  ( 0.000000000000000000, 0.000000000000000000, -1.000000000000000000 ) ) ;
#20928 = ORIENTED_EDGE ( 'NONE', *, *, #23914, .F. ) ;
#20929 = AXIS2_PLACEMENT_3D ( 'NONE', #12316, #2658, #38679 ) ;
#20930 = PRESENTATION_STYLE_ASSIGNMENT (( #7571 ) ) ;
#20931 = EDGE_CURVE ( 'NONE', #31507, #12750, #40888, .T. ) ;
#20932 = DIRECTION ( 'NONE',  ( -0.5000000000000016653, 0.8660254037844378194, 0.000000000000000000 ) ) ;
#20934 = VERTEX_POINT ( 'NONE', #30233 ) ;
#20933 = DIRECTION ( 'NONE',  ( 1.000000000000000000, 0.000000000000000000, 0.000000000000000000 ) ) ;
#20935 = DIRECTION ( 'NONE',  ( 0.000000000000000000, -0.9510565162951565288, 0.3090169943749383474 ) ) ;
#20936 = EDGE_LOOP ( 'NONE', ( #34356, #26376, #38163, #984 ) ) ;
#20937 = DIRECTION ( 'NONE',  ( 0.000000000000000000, -0.8443279255020087470, -0.5358267949790064266 ) ) ;
#20938 = CARTESIAN_POINT ( 'NONE',  ( 43.43872713698582544, 40.00000000000000000, 75.20828420317944563 ) ) ;
#20939 = CARTESIAN_POINT ( 'NONE',  ( -31.37281731866679024, 31.00000000000001776, 27.62913683693880174 ) ) ;
#20940 = EDGE_LOOP ( 'NONE', ( #30465, #12273 ) ) ;
#20941 = DIRECTION ( 'NONE',  ( -1.000000000000000000, 0.000000000000000000, 0.000000000000000000 ) ) ;
#20942 = CARTESIAN_POINT ( 'NONE',  ( 18.00000000000000355, -9.744342220503709129, 46.48873837489794880 ) ) ;
#20943 = ORIENTED_EDGE ( 'NONE', *, *, #41850, .F. ) ;
#20944 = DIRECTION ( 'NONE',  ( 0.000000000000000000, 0.000000000000000000, 1.000000000000000000 ) ) ;
#20945 = ORIENTED_EDGE ( 'NONE', *, *, #30506, .T. ) ;
#20946 = DIRECTION ( 'NONE',  ( -1.000000000000000000, -0.000000000000000000, 0.000000000000000000 ) ) ;
#20948 = ORIENTED_EDGE ( 'NONE', *, *, #15000, .F. ) ;
#20947 = EDGE_CURVE ( 'NONE', #39644, #22227, #16717, .T. ) ;
#20949 = CARTESIAN_POINT ( 'NONE',  ( 28.69597684714337049, 40.00000000000000000, 25.25520295781286251 ) ) ;
#20950 = FACE_OUTER_BOUND ( 'NONE', #20607, .T. ) ;
#20951 = EDGE_CURVE ( 'NONE', #23124, #1418, #17405, .T. ) ;
#20952 = DIRECTION ( 'NONE',  ( 0.000000000000000000, -0.2631025642275284238, 0.9647678688145140402 ) ) ;
#20953 = DIRECTION ( 'NONE',  ( 1.000000000000000000, 1.836909530733573776E-16, 0.000000000000000000 ) ) ;
#20954 = ORIENTED_EDGE ( 'NONE', *, *, #23518, .F. ) ;
#20956 = CYLINDRICAL_SURFACE ( 'NONE', #18609, 116.0000000000000000 ) ;
#20955 = CARTESIAN_POINT ( 'NONE',  ( 0.000000000000000000, -31.80866420683992857, 2.997093558041182160 ) ) ;
#20957 = ORIENTED_EDGE ( 'NONE', *, *, #12708, .T. ) ;
#20958 = CIRCLE ( 'NONE', #35533, 10.99999999999999645 ) ;
#20959 = CARTESIAN_POINT ( 'NONE',  ( -10.00000000000000000, 0.000000000000000000, 0.000000000000000000 ) ) ;
#20960 = AXIS2_PLACEMENT_3D ( 'NONE', #28089, #18091, #38513 ) ;
#20962 = CARTESIAN_POINT ( 'NONE',  ( 24.60508655230852781, 31.00000000000000355, 6.583411914924224284 ) ) ;
#20961 = AXIS2_PLACEMENT_3D ( 'NONE', #12491, #29072, #35160 ) ;
#20963 = ORIENTED_EDGE ( 'NONE', *, *, #37999, .F. ) ;
#20964 = CARTESIAN_POINT ( 'NONE',  ( 18.00000000000000355, -29.60891106212812574, 37.14118181634756155 ) ) ;
#20965 = AXIS2_PLACEMENT_3D ( 'NONE', #27279, #20328, #40339 ) ;
#20966 = DIRECTION ( 'NONE',  ( 1.000000000000000000, -0.000000000000000000, -0.000000000000000000 ) ) ;
#20967 = CONTEXT_DEPENDENT_SHAPE_REPRESENTATION ( #10867, #38777 ) ;
#20968 = EDGE_CURVE ( 'NONE', #30836, #20999, #33399, .T. ) ;
#20969 = DIRECTION ( 'NONE',  ( 0.000000000000000000, 0.000000000000000000, 1.000000000000000000 ) ) ;
#20970 = CARTESIAN_POINT ( 'NONE',  ( -34.23962737045593485, 31.00000000000000355, 59.30561363632230609 ) ) ;
#20971 = EDGE_LOOP ( 'NONE', ( #32783, #26974, #40612, #15758 ) ) ;
#20972 = CARTESIAN_POINT ( 'NONE',  ( -19.32876798325804302, 31.00000000000000355, -39.37500834189552279 ) ) ;
#20973 = CARTESIAN_POINT ( 'NONE',  ( 38.42722039544141666, 40.00000000000000000, 66.52996821281629991 ) ) ;
#20974 = EDGE_CURVE ( 'NONE', #12278, #25059, #10421, .T. ) ;
#20975 = CARTESIAN_POINT ( 'NONE',  ( 0.000000000000000000, 0.000000000000000000, 0.000000000000000000 ) ) ;
#20976 = AXIS2_PLACEMENT_3D ( 'NONE', #42518, #38399, #18387 ) ;
#20977 = CARTESIAN_POINT ( 'NONE',  ( 17.99999999999999645, 0.000000000000000000, 0.000000000000000000 ) ) ;
#20978 = EDGE_CURVE ( 'NONE', #34567, #8378, #39640, .T. ) ;
#20979 = CARTESIAN_POINT ( 'NONE',  ( 9.000000000000001776, -113.8630351447204134, -22.16324045874526405 ) ) ;
#20981 = VERTEX_POINT ( 'NONE', #29736 ) ;
#20980 = CARTESIAN_POINT ( 'NONE',  ( -10.00000000000000000, 0.000000000000000000, 0.000000000000000000 ) ) ;
#20982 = DIRECTION ( 'NONE',  ( 0.000000000000000000, 0.6783118362696123338, 0.7347741508630706297 ) ) ;
#20983 = CIRCLE ( 'NONE', #30727, 120.5010000000000474 ) ;
#20984 = CARTESIAN_POINT ( 'NONE',  ( 8.999999999999998224, -28.35267316522767445, -22.18391138608739155 ) ) ;
#20985 = ORIENTED_EDGE ( 'NONE', *, *, #33469, .F. ) ;
#20986 = CARTESIAN_POINT ( 'NONE',  ( -13.51098712749246467, 40.00000000000000000, -50.41620372279128048 ) ) ;
#20987 = DIRECTION ( 'NONE',  ( -1.000000000000000000, -0.000000000000000000, -0.000000000000000000 ) ) ;
#20989 = DIRECTION ( 'NONE',  ( -1.000000000000000000, -0.000000000000000000, 0.000000000000000000 ) ) ;
#20988 = CIRCLE ( 'NONE', #17490, 31.49899999999999878 ) ;
#20990 = B_SPLINE_CURVE_WITH_KNOTS ( 'NONE', 3,
 ( #6469, #19827, #13921, #16555 ),
 .UNSPECIFIED., .F., .F.,
 ( 4, 4 ),
 ( 0.000000000000000000, 0.002452478801916376308 ),
 .UNSPECIFIED. ) ;
#20991 = VECTOR ( 'NONE', #26537, 1000.000000000000000 ) ;
#20992 = VERTEX_POINT ( 'NONE', #43006 ) ;
#20993 = AXIS2_PLACEMENT_3D ( 'NONE', #38386, #28602, #22072 ) ;
#20994 = FACE_OUTER_BOUND ( 'NONE', #1518, .T. ) ;
#20995 = FACE_OUTER_BOUND ( 'NONE', #22594, .T. ) ;
#20996 = VECTOR ( 'NONE', #5159, 1000.000000000000000 ) ;
#20997 = EDGE_LOOP ( 'NONE', ( #9604, #5623, #39024, #9219 ) ) ;
#20998 = CYLINDRICAL_SURFACE ( 'NONE', #13820, 120.5010000000000190 ) ;
#20999 = VERTEX_POINT ( 'NONE', #7012 ) ;
#21000 = CARTESIAN_POINT ( 'NONE',  ( 17.99999999999999645, 0.000000000000000000, 0.000000000000000000 ) ) ;
#21001 = ORIENTED_EDGE ( 'NONE', *, *, #15165, .T. ) ;
#21002 = DIRECTION ( 'NONE',  ( -1.000000000000000000, -0.000000000000000000, 0.000000000000000000 ) ) ;
#21003 = EDGE_CURVE ( 'NONE', #1814, #13510, #40359, .T. ) ;
#21004 = CARTESIAN_POINT ( 'NONE',  ( -32.34013556242301490, 31.00000000000000355, 94.87070470182929682 ) ) ;
#21005 = ORIENTED_EDGE ( 'NONE', *, *, #717, .F. ) ;
#21006 = EDGE_CURVE ( 'NONE', #34092, #37795, #39728, .T. ) ;
#21007 = EDGE_CURVE ( 'NONE', #26154, #29573, #218, .T. ) ;
#21008 = ADVANCED_FACE ( 'NONE', ( #32978 ), #20365, .T. ) ;
#21009 = PLANE ( 'NONE',  #33117 ) ;
#21010 = DIRECTION ( 'NONE',  ( 0.000000000000000000, 0.000000000000000000, -1.000000000000000000 ) ) ;
#21011 = ORIENTED_EDGE ( 'NONE', *, *, #36497, .T. ) ;
#21012 = DIRECTION ( 'NONE',  ( -1.000000000000000000, -0.000000000000000000, 0.000000000000000000 ) ) ;
#21013 = DIRECTION ( 'NONE',  ( 1.000000000000000000, 0.000000000000000000, 0.000000000000000000 ) ) ;
#21014 = DIRECTION ( 'NONE',  ( 0.000000000000000000, 0.000000000000000000, 1.000000000000000000 ) ) ;
#21015 = AXIS2_PLACEMENT_3D ( 'NONE', #14070, #7055, #262 ) ;
#21016 = DIRECTION ( 'NONE',  ( -1.000000000000000000, -0.000000000000000000, -0.000000000000000000 ) ) ;
#21017 = ORIENTED_EDGE ( 'NONE', *, *, #22975, .T. ) ;
#21018 = DIRECTION ( 'NONE',  ( -1.836909530733573776E-16, -1.000000000000000000, 0.000000000000000000 ) ) ;
#21019 = CARTESIAN_POINT ( 'NONE',  ( 0.000000000000000000, 0.000000000000000000, 0.000000000000000000 ) ) ;
#21020 = CARTESIAN_POINT ( 'NONE',  ( 24.02862666965263116, 31.00000000000000355, 27.38392887651082575 ) ) ;
#21021 = AXIS2_PLACEMENT_3D ( 'NONE', #33015, #26490, #29774 ) ;
#21022 = ORIENTED_EDGE ( 'NONE', *, *, #17446, .T. ) ;
#21024 = LINE ( 'NONE', #24947, #35798 ) ;
#21023 = DIRECTION ( 'NONE',  ( -1.000000000000000000, 0.000000000000000000, 0.000000000000000000 ) ) ;
#21025 = AXIS2_PLACEMENT_3D ( 'NONE', #698, #16911, #26918 ) ;
#21026 = DIRECTION ( 'NONE',  ( 0.000000000000000000, 0.000000000000000000, -1.000000000000000000 ) ) ;
#21027 = ORIENTED_EDGE ( 'NONE', *, *, #21810, .T. ) ;
#21028 = CIRCLE ( 'NONE', #12618, 58.99999999999999289 ) ;
#21029 = DIRECTION ( 'NONE',  ( 1.000000000000000000, 0.000000000000000000, 0.000000000000000000 ) ) ;
#21030 = CARTESIAN_POINT ( 'NONE',  ( 26.72236725836960147, 40.00000000000000000, -46.28813965123160301 ) ) ;
#21031 = CARTESIAN_POINT ( 'NONE',  ( -17.30549157494238344, 40.00000000000000000, -51.24895740946764988 ) ) ;
#21032 = EDGE_CURVE ( 'NONE', #2829, #4469, #5533, .T. ) ;
#21033 = DIRECTION ( 'NONE',  ( 0.000000000000000000, 0.000000000000000000, -1.000000000000000000 ) ) ;
#21034 = CARTESIAN_POINT ( 'NONE',  ( 0.000000000000000000, 0.000000000000000000, 0.000000000000000000 ) ) ;
#21035 = EDGE_CURVE ( 'NONE', #33113, #40305, #39516, .T. ) ;
#21036 = VECTOR ( 'NONE', #19078, 1000.000000000000000 ) ;
#21037 = DIRECTION ( 'NONE',  ( 0.000000000000000000, -0.5000000000000009992, -0.8660254037844380415 ) ) ;
#21038 = CARTESIAN_POINT ( 'NONE',  ( 0.000000000000000000, -42.41764978026621691, 20.20639853260276197 ) ) ;
#21039 = ORIENTED_EDGE ( 'NONE', *, *, #15339, .F. ) ;
#21040 = CARTESIAN_POINT ( 'NONE',  ( 13.36968668718156295, 40.00000000000000000, 23.13838826010315941 ) ) ;
#21041 = VERTEX_POINT ( 'NONE', #9655 ) ;
#21042 = CARTESIAN_POINT ( 'NONE',  ( 18.00000000000000355, 47.49120266317495265, 0.8606222198176843863 ) ) ;
#21043 = DIRECTION ( 'NONE',  ( -1.000000000000000000, -0.000000000000000000, -0.000000000000000000 ) ) ;
#21044 = ORIENTED_EDGE ( 'NONE', *, *, #40138, .T. ) ;
#21045 = CARTESIAN_POINT ( 'NONE',  ( 17.99999999999999645, -66.49630760163661591, 90.36876423295966276 ) ) ;
#21046 = CARTESIAN_POINT ( 'NONE',  ( 2.500000000000000000, 2.357898499370431722, -2.818925648462311528E-15 ) ) ;
#21047 = EDGE_LOOP ( 'NONE', ( #29239, #41131, #8798, #11552 ) ) ;
#21048 = CARTESIAN_POINT ( 'NONE',  ( 17.99999999999999645, 45.89132998248186368, -102.3829004574625401 ) ) ;
#21049 = VERTEX_POINT ( 'NONE', #23207 ) ;
#21050 = AXIS2_PLACEMENT_3D ( 'NONE', #10556, #23466, #26711 ) ;
#21051 = VERTEX_POINT ( 'NONE', #19715 ) ;
#21053 = ORIENTED_EDGE ( 'NONE', *, *, #20882, .T. ) ;
#21052 = CARTESIAN_POINT ( 'NONE',  ( 0.000000000000000000, 0.000000000000000000, 0.000000000000000000 ) ) ;
#21054 = AXIS2_PLACEMENT_3D ( 'NONE', #42347, #22754, #22127 ) ;
#21055 = EDGE_CURVE ( 'NONE', #6447, #40171, #32016, .T. ) ;
#21056 = CARTESIAN_POINT ( 'NONE',  ( -72.09351246574976813, 31.00000000000000711, -4.825959690424619808 ) ) ;
#21057 = ORIENTED_EDGE ( 'NONE', *, *, #517, .F. ) ;
#21058 = CYLINDRICAL_SURFACE ( 'NONE', #41165, 59.00000000000000000 ) ;
#21059 = EDGE_CURVE ( 'NONE', #6599, #40723, #3710, .T. ) ;
#21060 = ADVANCED_FACE ( 'NONE', ( #42575 ), #36244, .F. ) ;
#21061 = EDGE_CURVE ( 'NONE', #31789, #4637, #3418, .T. ) ;
#21062 = AXIS2_PLACEMENT_3D ( 'NONE', #28747, #18753, #16082 ) ;
#21063 = ORIENTED_EDGE ( 'NONE', *, *, #2560, .F. ) ;
#21064 = DIRECTION ( 'NONE',  ( 0.000000000000000000, 0.000000000000000000, -1.000000000000000000 ) ) ;
#21065 = ADVANCED_FACE ( 'NONE', ( #6367 ), #9705, .T. ) ;
#21066 = ORIENTED_EDGE ( 'NONE', *, *, #22811, .F. ) ;
#21067 = CARTESIAN_POINT ( 'NONE',  ( -72.38966680857410552, 40.00000000000000711, 55.38960906678870799 ) ) ;
#21068 = VECTOR ( 'NONE', #5978, 1000.000000000000000 ) ;
#21070 = LINE ( 'NONE', #25196, #3970 ) ;
#21069 = CARTESIAN_POINT ( 'NONE',  ( 0.000000000000000000, -41.33768078145432412, -104.3046912715545318 ) ) ;
#21071 = CARTESIAN_POINT ( 'NONE',  ( 0.000000000000000000, 0.000000000000000000, 0.000000000000000000 ) ) ;
#21072 = DIRECTION ( 'NONE',  ( -1.847415842360817484E-16, 1.000000000000000000, 0.000000000000000000 ) ) ;
#21073 = ORIENTED_EDGE ( 'NONE', *, *, #2272, .T. ) ;
#21074 = SURFACE_STYLE_FILL_AREA ( #10777 ) ;
#21075 = FILL_AREA_STYLE_COLOUR ( '', #33127 ) ;
#21076 = DIRECTION ( 'NONE',  ( -1.000000000000000000, -0.000000000000000000, -0.000000000000000000 ) ) ;
#21077 = CARTESIAN_POINT ( 'NONE',  ( -87.52616871875942195, 31.00000000000000711, -23.43677886868077209 ) ) ;
#21078 = DIRECTION ( 'NONE',  ( -0.3211947320043981868, -5.016842274700473727E-16, -0.9470131699890044219 ) ) ;
#21079 = ORIENTED_EDGE ( 'NONE', *, *, #21360, .F. ) ;
#21080 = CARTESIAN_POINT ( 'NONE',  ( -21.37212791037562098, 40.00000000000000000, -7.253704819186252983 ) ) ;
#21081 = AXIS2_PLACEMENT_3D ( 'NONE', #37537, #7645, #24933 ) ;
#21082 = VERTEX_POINT ( 'NONE', #13376 ) ;
#21083 = AXIS2_PLACEMENT_3D ( 'NONE', #22656, #26123, #2523 ) ;
#21084 = EDGE_LOOP ( 'NONE', ( #19948, #17382, #16650, #18038 ) ) ;
#21085 = DIRECTION ( 'NONE',  ( 0.000000000000000000, 0.000000000000000000, 1.000000000000000000 ) ) ;
#21086 = CARTESIAN_POINT ( 'NONE',  ( -8.920000000000003482, 0.000000000000000000, 0.000000000000000000 ) ) ;
#21087 = DIRECTION ( 'NONE',  ( 0.000000000000000000, -0.9968120070307509017, 0.07978610555307326380 ) ) ;
#21088 = CIRCLE ( 'NONE', #2872, 10.99999999999998934 ) ;
#21089 = CARTESIAN_POINT ( 'NONE',  ( 17.99999999999999645, 112.5120133921113563, -43.14554256760899875 ) ) ;
#21090 = VERTEX_POINT ( 'NONE', #3060 ) ;
#21091 = DIRECTION ( 'NONE',  ( -1.000000000000000000, 0.000000000000000000, 0.000000000000000000 ) ) ;
#21092 = ORIENTED_EDGE ( 'NONE', *, *, #27184, .F. ) ;
#21093 = LINE ( 'NONE', #15185, #39618 ) ;
#21094 = TOROIDAL_SURFACE ( 'NONE', #35661, 19.11697999999999809, 0.08401999999999931745 ) ;
#21095 = CARTESIAN_POINT ( 'NONE',  ( -16.41266422346948772, 17.11489954122026447, -1.216702565357022037 ) ) ;
#21096 = CARTESIAN_POINT ( 'NONE',  ( 2.500000000000000000, 2.357898499370431722, -2.818925648462311528E-15 ) ) ;
#21097 = DIRECTION ( 'NONE',  ( 1.000000000000000000, 0.000000000000000000, 0.000000000000000000 ) ) ;
#21098 = ORIENTED_EDGE ( 'NONE', *, *, #1300, .T. ) ;
#21099 = ORIENTED_EDGE ( 'NONE', *, *, #18329, .T. ) ;
#21100 = DIRECTION ( 'NONE',  ( -1.000000000000000000, -0.000000000000000000, -0.000000000000000000 ) ) ;
#21101 = CYLINDRICAL_SURFACE ( 'NONE', #28404, 59.00000000000000000 ) ;
#21102 = CARTESIAN_POINT ( 'NONE',  ( 4.000000000000000000, 1.680228229147133767, -3.316631783032546021 ) ) ;
#21103 = ORIENTED_EDGE ( 'NONE', *, *, #12659, .F. ) ;
#21105 = ORIENTED_EDGE ( 'NONE', *, *, #43055, .T. ) ;
#21104 = CARTESIAN_POINT ( 'NONE',  ( -158.4999999999992042, 2.557839043092172690E-13, 7.000000000000065725 ) ) ;
#21106 = CARTESIAN_POINT ( 'NONE',  ( 21.53706125532763593, 31.00000000000000355, 43.87245753946415761 ) ) ;
#21107 = LINE ( 'NONE', #41321, #36937 ) ;
#21108 = EDGE_CURVE ( 'NONE', #43124, #25635, #12724, .T. ) ;
#21109 = ADVANCED_FACE ( 'NONE', ( #37975 ), #30600, .T. ) ;
#21111 = DIRECTION ( 'NONE',  ( -1.000000000000000000, -0.000000000000000000, -0.000000000000000000 ) ) ;
#21110 = CARTESIAN_POINT ( 'NONE',  ( 18.00000000000000355, 41.20225022064636278, 23.63323037071415911 ) ) ;
#21112 = ADVANCED_FACE ( 'NONE', ( #37115 ), #7223, .F. ) ;
#21113 = ORIENTED_EDGE ( 'NONE', *, *, #20020, .T. ) ;
#21114 = CIRCLE ( 'NONE', #14834, 52.00000000000000000 ) ;
#21115 = CARTESIAN_POINT ( 'NONE',  ( -56.33579487689732446, 40.00000000000000000, -27.88694065509425357 ) ) ;
#21116 = AXIS2_PLACEMENT_3D ( 'NONE', #12950, #29746, #10078 ) ;
#21117 = CARTESIAN_POINT ( 'NONE',  ( 0.000000000000000000, 0.000000000000000000, 0.000000000000000000 ) ) ;
#21118 = CYLINDRICAL_SURFACE ( 'NONE', #22021, 31.49899999999999878 ) ;
#21119 = ORIENTED_EDGE ( 'NONE', *, *, #8506, .T. ) ;
#21120 = CARTESIAN_POINT ( 'NONE',  ( 8.919999999999996376, 0.000000000000000000, 0.000000000000000000 ) ) ;
#21121 = EDGE_CURVE ( 'NONE', #4294, #29681, #35876, .T. ) ;
#21122 = ORIENTED_EDGE ( 'NONE', *, *, #16197, .F. ) ;
#21123 = AXIS2_PLACEMENT_3D ( 'NONE', #25566, #2592, #8952 ) ;
#21124 = CARTESIAN_POINT ( 'NONE',  ( 17.99999999999999645, -105.3681574666261298, -38.54638589714993202 ) ) ;
#21125 = CYLINDRICAL_SURFACE ( 'NONE', #21352, 59.00000000000000000 ) ;
#21126 = EDGE_CURVE ( 'NONE', #10322, #25878, #9417, .T. ) ;
#21127 = CARTESIAN_POINT ( 'NONE',  ( -30.90996028308246224, 31.00000000000000355, -53.51249422725337013 ) ) ;
#21128 = DIRECTION ( 'NONE',  ( 0.000000000000000000, 0.000000000000000000, 1.000000000000000000 ) ) ;
#21129 = ORIENTED_EDGE ( 'NONE', *, *, #6053, .F. ) ;
#21130 = LINE ( 'NONE', #11496, #4498 ) ;
#21131 = VERTEX_POINT ( 'NONE', #1331 ) ;
#21132 = CARTESIAN_POINT ( 'NONE',  ( -26.30698076681265363, 40.00000000000000000, 12.97770382244945253 ) ) ;
#21133 = VERTEX_POINT ( 'NONE', #11387 ) ;
#21134 = DIRECTION ( 'NONE',  ( -1.000000000000000000, -0.000000000000000000, -0.000000000000000000 ) ) ;
#21135 = CARTESIAN_POINT ( 'NONE',  ( 9.000000000000001776, -35.78484819117565507, -110.3423972910436390 ) ) ;
#21136 = CARTESIAN_POINT ( 'NONE',  ( -53.37462671637112521, 31.00000000000000711, 60.68184199296217685 ) ) ;
#21137 = CARTESIAN_POINT ( 'NONE',  ( -86.84058463553202500, 40.00000000000000711, 29.36381822872188607 ) ) ;
#21138 = DIRECTION ( 'NONE',  ( 0.000000000000000000, 0.000000000000000000, 1.000000000000000000 ) ) ;
#21139 = ADVANCED_FACE ( 'NONE', ( #24512 ), #14674, .F. ) ;
#21140 = ORIENTED_EDGE ( 'NONE', *, *, #38912, .T. ) ;
#21141 = DIRECTION ( 'NONE',  ( -1.000000000000000000, 0.000000000000000000, -0.000000000000000000 ) ) ;
#21142 = VERTEX_POINT ( 'NONE', #41244 ) ;
#21143 = DIRECTION ( 'NONE',  ( 0.000000000000000000, 0.8183027759081663577, 0.5747874102144109321 ) ) ;
#21144 = DIRECTION ( 'NONE',  ( -1.000000000000000000, 0.000000000000000000, 0.000000000000000000 ) ) ;
#21145 = AXIS2_PLACEMENT_3D ( 'NONE', #14366, #16798, #27681 ) ;
#21147 = ORIENTED_EDGE ( 'NONE', *, *, #6683, .T. ) ;
#21146 = DIRECTION ( 'NONE',  ( -0.9997917317482359900, -0.02040816326530612776, 0.000000000000000000 ) ) ;
#21148 = DIRECTION ( 'NONE',  ( 1.000000000000000000, 0.000000000000000000, 0.000000000000000000 ) ) ;
#21149 = ORIENTED_EDGE ( 'NONE', *, *, #33951, .T. ) ;
#21150 = CARTESIAN_POINT ( 'NONE',  ( 9.000000000000001776, -13.56094713063606783, 50.20060470671735686 ) ) ;
#21151 = CARTESIAN_POINT ( 'NONE',  ( -43.52407497442469264, 40.00000000000000000, 88.29422169633753015 ) ) ;
#21152 = FACE_OUTER_BOUND ( 'NONE', #28621, .T. ) ;
#21153 = AXIS2_PLACEMENT_3D ( 'NONE', #31396, #7605, #1480 ) ;
#21154 = ORIENTED_EDGE ( 'NONE', *, *, #13893, .T. ) ;
#21155 = CARTESIAN_POINT ( 'NONE',  ( -10.00000000000000000, 0.000000000000000000, 0.000000000000000000 ) ) ;
#21156 = CYLINDRICAL_SURFACE ( 'NONE', #19723, 59.00000000000000000 ) ;
#21157 = EDGE_CURVE ( 'NONE', #18006, #33231, #27572, .T. ) ;
#21159 = CYLINDRICAL_SURFACE ( 'NONE', #42883, 116.0000000000000000 ) ;
#21158 = DIRECTION ( 'NONE',  ( -1.000000000000000000, 1.373900992973641868E-15, 4.405646923115722869E-16 ) ) ;
#21160 = VERTEX_POINT ( 'NONE', #10725 ) ;
#21161 = CARTESIAN_POINT ( 'NONE',  ( 18.00000000000000355, -22.82995208772658557, -41.06517797613689424 ) ) ;
#21162 = ORIENTED_EDGE ( 'NONE', *, *, #23782, .T. ) ;
#21163 = LINE ( 'NONE', #199, #16134 ) ;
#21164 = CARTESIAN_POINT ( 'NONE',  ( 27.04960320298795651, 40.00000000000000000, -23.64836272119224247 ) ) ;
#21165 = DIRECTION ( 'NONE',  ( 1.000000000000000000, 0.000000000000000000, 0.000000000000000000 ) ) ;
#21166 = EDGE_CURVE ( 'NONE', #15350, #2405, #35913, .T. ) ;
#21167 = CARTESIAN_POINT ( 'NONE',  ( -101.6738636939643357, 17.11489954122025736, -5.192942712545352890 ) ) ;
#21168 = CARTESIAN_POINT ( 'NONE',  ( 18.00000000000000355, 39.55064067543064965, 25.36340625197373555 ) ) ;
#21169 = ORIENTED_EDGE ( 'NONE', *, *, #33183, .F. ) ;
#21171 = DIRECTION ( 'NONE',  ( -1.000000000000000000, -0.000000000000000000, -0.000000000000000000 ) ) ;
#21170 = CARTESIAN_POINT ( 'NONE',  ( 17.99999999999999645, -57.69704296431255131, 105.7900857083227777 ) ) ;
#21172 = EDGE_CURVE ( 'NONE', #35521, #25440, #34717, .T. ) ;
#21173 = ORIENTED_EDGE ( 'NONE', *, *, #685, .F. ) ;
#21174 = DIRECTION ( 'NONE',  ( 0.000000000000000000, -0.5528000653612000770, 0.8333139190825106235 ) ) ;
#21175 = EDGE_CURVE ( 'NONE', #27084, #18808, #17088, .T. ) ;
#21176 = CARTESIAN_POINT ( 'NONE',  ( -23.02120395722396395, 31.00000000000000355, 17.66995642160909696 ) ) ;
#21177 = ORIENTED_EDGE ( 'NONE', *, *, #23679, .T. ) ;
#21178 = CARTESIAN_POINT ( 'NONE',  ( 0.000000000000000000, 32.49609705003727100, -15.49205204337240005 ) ) ;
#21179 = DIRECTION ( 'NONE',  ( 0.000000000000000000, -4.441553645588922428E-15, -1.000000000000000000 ) ) ;
#21180 =( GEOMETRIC_REPRESENTATION_CONTEXT ( 3 ) GLOBAL_UNCERTAINTY_ASSIGNED_CONTEXT ( ( #7312 ) ) GLOBAL_UNIT_ASSIGNED_CONTEXT ( ( #38714, #28721, #28518 ) ) REPRESENTATION_CONTEXT ( 'NONE', 'WORKASPACE' ) );
#21181 = DIRECTION ( 'NONE',  ( -1.000000000000000000, 0.000000000000000000, 0.000000000000000000 ) ) ;
#21182 = CARTESIAN_POINT ( 'NONE',  ( 68.07048008643859305, 31.00000000000000000, 33.55317283102968418 ) ) ;
#21183 = AXIS2_PLACEMENT_3D ( 'NONE', #33312, #3397, #30055 ) ;
#21184 = ORIENTED_EDGE ( 'NONE', *, *, #9584, .T. ) ;
#21185 = CARTESIAN_POINT ( 'NONE',  ( 27.84166646522859878, 31.00000000000000355, -36.16032403484085478 ) ) ;
#21186 = CARTESIAN_POINT ( 'NONE',  ( 19.99305134020393382, 40.00000000000000000, 74.61661993947731730 ) ) ;
#21187 = ADVANCED_FACE ( 'NONE', ( #17322 ), #30805, .F. ) ;
#21188 = EDGE_CURVE ( 'NONE', #31882, #2747, #14338, .T. ) ;
#21189 = DIRECTION ( 'NONE',  ( -1.000000000000000000, -0.000000000000000000, -0.000000000000000000 ) ) ;
#21190 = CARTESIAN_POINT ( 'NONE',  ( 17.99999999999999645, 0.000000000000000000, 0.000000000000000000 ) ) ;
#21191 = ADVANCED_FACE ( 'NONE', ( #34490 ), #11176, .T. ) ;
#21192 = DIRECTION ( 'NONE',  ( -1.000000000000000000, 0.000000000000000000, 0.000000000000000000 ) ) ;
#21194 = ORIENTED_EDGE ( 'NONE', *, *, #16618, .T. ) ;
#21193 = CYLINDRICAL_SURFACE ( 'NONE', #31389, 120.5010000000000190 ) ;
#21195 = DIRECTION ( 'NONE',  ( 0.000000000000000000, 0.000000000000000000, 1.000000000000000000 ) ) ;
#21196 = DIRECTION ( 'NONE',  ( 0.000000000000000000, 0.000000000000000000, 1.000000000000000000 ) ) ;
#21197 = VECTOR ( 'NONE', #33587, 1000.000000000000000 ) ;
#21198 = ORIENTED_EDGE ( 'NONE', *, *, #28823, .T. ) ;
#21199 = CARTESIAN_POINT ( 'NONE',  ( 43.85342918759069164, 40.00000000000000000, 49.98553323097543455 ) ) ;
#21200 = DIRECTION ( 'NONE',  ( 0.000000000000000000, 0.000000000000000000, 1.000000000000000000 ) ) ;
#21201 = CYLINDRICAL_SURFACE ( 'NONE', #26300, 120.5010000000000190 ) ;
#21202 = ORIENTED_EDGE ( 'NONE', *, *, #23934, .F. ) ;
#21203 = CARTESIAN_POINT ( 'NONE',  ( 8.999999999999998224, 79.18387647320879807, -84.76976882518680156 ) ) ;
#21204 = FACE_OUTER_BOUND ( 'NONE', #156, .T. ) ;
#21205 = VERTEX_POINT ( 'NONE', #10515 ) ;
#21206 = DIRECTION ( 'NONE',  ( 0.000000000000000000, 0.000000000000000000, -1.000000000000000000 ) ) ;
#21207 = VERTEX_POINT ( 'NONE', #665 ) ;
#21208 = ADVANCED_FACE ( 'NONE', ( #1107 ), #40587, .F. ) ;
#21209 = CARTESIAN_POINT ( 'NONE',  ( 17.99999999999999645, -120.4984140710909202, -0.7894348306996294973 ) ) ;
#21210 = AXIS2_PLACEMENT_3D ( 'NONE', #17635, #27647, #7323 ) ;
#21211 = VERTEX_POINT ( 'NONE', #27537 ) ;
#21212 = CARTESIAN_POINT ( 'NONE',  ( 17.99999999999999645, -31.81777574834308098, 2.898764365605205562 ) ) ;
#21213 = DIRECTION ( 'NONE',  ( 1.000000000000000000, 0.000000000000000000, 0.000000000000000000 ) ) ;
#21214 = ORIENTED_EDGE ( 'NONE', *, *, #5669, .T. ) ;
#21215 = FACE_OUTER_BOUND ( 'NONE', #19001, .T. ) ;
#21216 = CARTESIAN_POINT ( 'NONE',  ( -10.00000000000000000, 0.000000000000000000, 0.000000000000000000 ) ) ;
#21218 = VERTEX_POINT ( 'NONE', #40812 ) ;
#21217 = AXIS2_PLACEMENT_3D ( 'NONE', #43037, #29331, #16693 ) ;
#21219 = DIRECTION ( 'NONE',  ( 0.000000000000000000, -0.8443279255020200713, 0.5358267949789887741 ) ) ;
#21220 = ADVANCED_FACE ( 'NONE', ( #10964 ), #14460, .T. ) ;
#21221 =( REPRESENTATION_RELATIONSHIP ('NONE','NONE', #330, #18009 ) REPRESENTATION_RELATIONSHIP_WITH_TRANSFORMATION ( #10458 )SHAPE_REPRESENTATION_RELATIONSHIP( ) );
#21222 = CARTESIAN_POINT ( 'NONE',  ( 0.000000000000000000, 0.000000000000000000, 0.000000000000000000 ) ) ;
#21223 = CARTESIAN_POINT ( 'NONE',  ( 0.000000000000000000, 64.69195966009891663, 96.28577441832274530 ) ) ;
#21224 = VECTOR ( 'NONE', #29256, 1000.000000000000000 ) ;
#21225 = ADVANCED_FACE ( 'NONE', ( #16322, #1543 ), #38992, .F. ) ;
#21226 = CARTESIAN_POINT ( 'NONE',  ( 17.99999999999999645, -29.36437154451924059, -116.8684075565139295 ) ) ;
#21227 = EDGE_LOOP ( 'NONE', ( #36063, #36824, #35764, #10033 ) ) ;
#21228 = CARTESIAN_POINT ( 'NONE',  ( -83.76341667917206735, 8.999999999999992895, 6.300002081858490754 ) ) ;
#21230 = AXIS2_PLACEMENT_3D ( 'NONE', #5849, #16128, #22054 ) ;
#21229 = DIRECTION ( 'NONE',  ( 0.000000000000000000, 0.000000000000000000, 1.000000000000000000 ) ) ;
#21231 = CARTESIAN_POINT ( 'NONE',  ( -33.94102792873697183, 31.00000000000000355, -38.68473105385043453 ) ) ;
#21232 = ORIENTED_EDGE ( 'NONE', *, *, #33858, .T. ) ;
#21234 = FACE_OUTER_BOUND ( 'NONE', #20740, .T. ) ;
#21233 = FACE_OUTER_BOUND ( 'NONE', #32841, .T. ) ;
#21235 = DIRECTION ( 'NONE',  ( -1.000000000000000000, 0.000000000000000000, -0.000000000000000000 ) ) ;
#21236 = ORIENTED_EDGE ( 'NONE', *, *, #6275, .T. ) ;
#21237 = DIRECTION ( 'NONE',  ( -1.000000000000000000, 0.000000000000000000, -0.000000000000000000 ) ) ;
#21238 = CARTESIAN_POINT ( 'NONE',  ( 30.63689417572177831, 40.00000000000000000, 34.91779699477408627 ) ) ;
#21239 = CARTESIAN_POINT ( 'NONE',  ( 0.000000000000000000, 0.000000000000000000, 0.000000000000000000 ) ) ;
#21240 = CARTESIAN_POINT ( 'NONE',  ( 38.48770111205618605, 40.00000000000000000, 44.02435964457617956 ) ) ;
#21241 = CIRCLE ( 'NONE', #42772, 2.649999999999971934 ) ;
#21242 =( GEOMETRIC_REPRESENTATION_CONTEXT ( 3 ) GLOBAL_UNCERTAINTY_ASSIGNED_CONTEXT ( ( #10384 ) ) GLOBAL_UNIT_ASSIGNED_CONTEXT ( ( #23770, #27241, #4512 ) ) REPRESENTATION_CONTEXT ( 'NONE', 'WORKASPACE' ) );
#21243 = EDGE_CURVE ( 'NONE', #5141, #9900, #25510, .T. ) ;
#21244 = FACE_OUTER_BOUND ( 'NONE', #14360, .T. ) ;
#21245 = CARTESIAN_POINT ( 'NONE',  ( 17.99999999999999645, -111.2721026680461733, 14.38025178762581469 ) ) ;
#21246 = EDGE_CURVE ( 'NONE', #12177, #3549, #37291, .T. ) ;
#21247 = DIRECTION ( 'NONE',  ( 1.000000000000000000, 0.000000000000000000, 0.000000000000000000 ) ) ;
#21248 = AXIS2_PLACEMENT_3D ( 'NONE', #37308, #23824, #7423 ) ;
#21249 = CARTESIAN_POINT ( 'NONE',  ( 17.99999999999999645, -67.32409792376564894, 89.75376489259340929 ) ) ;
#21250 = CIRCLE ( 'NONE', #2362, 100.0000000000000000 ) ;
#21251 = ORIENTED_EDGE ( 'NONE', *, *, #29979, .F. ) ;
#21252 = CARTESIAN_POINT ( 'NONE',  ( -29.89583333557403222, 40.00000000000000000, 1.963495399902740690 ) ) ;
#21253 = ORIENTED_EDGE ( 'NONE', *, *, #737, .F. ) ;
#21254 = DIRECTION ( 'NONE',  ( -1.000000000000000000, 0.000000000000000000, 0.000000000000000000 ) ) ;
#21255 = CARTESIAN_POINT ( 'NONE',  ( 0.000000000000000000, 47.31079789947484926, 105.9135893174952656 ) ) ;
#21256 = CIRCLE ( 'NONE', #12199, 59.00000000000000711 ) ;
#21257 = VERTEX_POINT ( 'NONE', #42681 ) ;
#21258 = EDGE_CURVE ( 'NONE', #27491, #12909, #29207, .T. ) ;
#21259 = FACE_OUTER_BOUND ( 'NONE', #482, .T. ) ;
#21260 = CIRCLE ( 'NONE', #26117, 120.5010000000000332 ) ;
#21261 = PLANE ( 'NONE',  #32455 ) ;
#21262 = ORIENTED_EDGE ( 'NONE', *, *, #26144, .T. ) ;
#21263 = CARTESIAN_POINT ( 'NONE',  ( -104.2750351721725650, 17.11489954122025736, -4.541977405098627685 ) ) ;
#21264 = ORIENTED_EDGE ( 'NONE', *, *, #15961, .T. ) ;
#21265 = EDGE_CURVE ( 'NONE', #3549, #12177, #18548, .T. ) ;
#21266 = AXIS2_PLACEMENT_3D ( 'NONE', #28100, #41362, #20935 ) ;
#21267 = ORIENTED_EDGE ( 'NONE', *, *, #27414, .F. ) ;
#21268 = FACE_OUTER_BOUND ( 'NONE', #24428, .T. ) ;
#21269 = CARTESIAN_POINT ( 'NONE',  ( 37.84579180137232157, 31.00000000000000355, -65.31998993212283722 ) ) ;
#21270 = ORIENTED_EDGE ( 'NONE', *, *, #28352, .T. ) ;
#21271 = DIRECTION ( 'NONE',  ( -3.996523416598930318E-16, 2.658563593772947863E-15, 1.000000000000000000 ) ) ;
#21272 = DIRECTION ( 'NONE',  ( -1.000000000000000000, -0.000000000000000000, 0.000000000000000000 ) ) ;
#21273 = ORIENTED_EDGE ( 'NONE', *, *, #19578, .T. ) ;
#21275 = CIRCLE ( 'NONE', #24758, 20.00000000000000711 ) ;
#21274 = DIRECTION ( 'NONE',  ( 1.000000000000000000, 0.000000000000000000, 0.000000000000000000 ) ) ;
#21276 = EDGE_CURVE ( 'NONE', #5508, #8087, #25935, .T. ) ;
#21277 = VERTEX_POINT ( 'NONE', #35707 ) ;
#21278 = CARTESIAN_POINT ( 'NONE',  ( 87.78546986784174067, 39.99999999999999289, 43.41392487578124815 ) ) ;
#21279 = EDGE_CURVE ( 'NONE', #16491, #16762, #22676, .T. ) ;
#21281 = CARTESIAN_POINT ( 'NONE',  ( 8.999999999999998224, 95.31344542257821217, -66.11616384574354299 ) ) ;
#21280 = FACE_OUTER_BOUND ( 'NONE', #38432, .T. ) ;
#21282 = CARTESIAN_POINT ( 'NONE',  ( 17.99999999999999645, 0.000000000000000000, 0.000000000000000000 ) ) ;
#21283 = CARTESIAN_POINT ( 'NONE',  ( 18.00000000000000355, 40.47821179127715396, 32.64221760512772619 ) ) ;
#21284 = ORIENTED_EDGE ( 'NONE', *, *, #4821, .F. ) ;
#21285 = AXIS2_PLACEMENT_3D ( 'NONE', #19440, #2580, #39872 ) ;
#21286 = FACE_OUTER_BOUND ( 'NONE', #9097, .T. ) ;
#21287 = VERTEX_POINT ( 'NONE', #39414 ) ;
#21288 = AXIS2_PLACEMENT_3D ( 'NONE', #18794, #22270, #32048 ) ;
#21289 = CARTESIAN_POINT ( 'NONE',  ( 18.00000000000000355, 0.000000000000000000, 0.000000000000000000 ) ) ;
#21290 = CARTESIAN_POINT ( 'NONE',  ( 21.49215960483416410, 31.00000000000000355, -80.26604385357094884 ) ) ;
#21291 = AXIS2_PLACEMENT_3D ( 'NONE', #35397, #16206, #35595 ) ;
#21292 = CARTESIAN_POINT ( 'NONE',  ( 0.000000000000000000, 0.000000000000000000, 0.000000000000000000 ) ) ;
#21293 = ORIENTED_EDGE ( 'NONE', *, *, #33430, .F. ) ;
#21294 = PRESENTATION_LAYER_ASSIGNMENT (  '', '', ( #18521 ) ) ;
#21295 = CARTESIAN_POINT ( 'NONE',  ( -31.59164309906362078, 40.00000000000000000, 4.115917706318550806 ) ) ;
#21296 = CIRCLE ( 'NONE', #37960, 13.60000000000000142 ) ;
#21297 = EDGE_LOOP ( 'NONE', ( #20308, #36985, #3073, #10309 ) ) ;
#21298 = EDGE_CURVE ( 'NONE', #25238, #8366, #39362, .T. ) ;
#21299 = VERTEX_POINT ( 'NONE', #9551 ) ;
#21300 = CARTESIAN_POINT ( 'NONE',  ( 8.999999999999998224, 69.72480978690046527, 92.70626138606036193 ) ) ;
#21301 = DIRECTION ( 'NONE',  ( 0.000000000000000000, 0.8443279255020126328, 0.5358267949790005424 ) ) ;
#21302 = EDGE_CURVE ( 'NONE', #10153, #32077, #15043, .T. ) ;
#21303 = CARTESIAN_POINT ( 'NONE',  ( -10.00000000000000178, 0.000000000000000000, 0.000000000000000000 ) ) ;
#21304 = ADVANCED_FACE ( 'NONE', ( #5835 ), #8912, .F. ) ;
#21305 = EDGE_CURVE ( 'NONE', #5822, #23930, #20616, .T. ) ;
#21306 = DIRECTION ( 'NONE',  ( 0.000000000000000000, -0.3681245526846653737, -0.9297764858882564543 ) ) ;
#21307 = CIRCLE ( 'NONE', #24784, 58.99999999999999289 ) ;
#21308 = ORIENTED_EDGE ( 'NONE', *, *, #4301, .T. ) ;
#21309 = CARTESIAN_POINT ( 'NONE',  ( 18.00000000000000355, 35.20873326984126805, -31.88259874183992792 ) ) ;
#21310 = ORIENTED_EDGE ( 'NONE', *, *, #1849, .T. ) ;
#21311 = CARTESIAN_POINT ( 'NONE',  ( -4.211140560182196957, 2.431303136016537803, -3.745885042887433514 ) ) ;
#21312 = LINE ( 'NONE', #34561, #30473 ) ;
#21313 = CYLINDRICAL_SURFACE ( 'NONE', #28424, 59.00000000000000000 ) ;
#21314 = AXIS2_PLACEMENT_3D ( 'NONE', #22982, #200, #2831 ) ;
#21315 = DIRECTION ( 'NONE',  ( 0.000000000000000000, 0.9996456111234524045, 0.02662052143777833904 ) ) ;
#21316 = ORIENTED_EDGE ( 'NONE', *, *, #19807, .F. ) ;
#21317 = VERTEX_POINT ( 'NONE', #19408 ) ;
#21318 = DIRECTION ( 'NONE',  ( -1.000000000000000000, -0.000000000000000000, -0.000000000000000000 ) ) ;
#21319 = CARTESIAN_POINT ( 'NONE',  ( 0.000000000000000000, -150.5000000000000284, 9.999999999999998224 ) ) ;
#21320 = VERTEX_POINT ( 'NONE', #32673 ) ;
#21321 = AXIS2_PLACEMENT_3D ( 'NONE', #13930, #17217, #37458 ) ;
#21323 = ORIENTED_EDGE ( 'NONE', *, *, #42657, .T. ) ;
#21322 = DIRECTION ( 'NONE',  ( 1.000000000000000000, 0.000000000000000000, 0.000000000000000000 ) ) ;
#21324 = CARTESIAN_POINT ( 'NONE',  ( 45.87644943786595064, 31.00000000000000355, 12.37342411884007376 ) ) ;
#21325 = LINE ( 'NONE', #34578, #13308 ) ;
#21326 = AXIS2_PLACEMENT_3D ( 'NONE', #36743, #7282, #20643 ) ;
#21328 =( NAMED_UNIT ( * ) SI_UNIT ( $, .STERADIAN. ) SOLID_ANGLE_UNIT ( ) );
#21327 = DIRECTION ( 'NONE',  ( -1.000000000000000000, -0.000000000000000000, -0.000000000000000000 ) ) ;
#21329 = EDGE_CURVE ( 'NONE', #31963, #17636, #16423, .T. ) ;
#21330 = VERTEX_POINT ( 'NONE', #35511 ) ;
#21331 = DIRECTION ( 'NONE',  ( 0.000000000000000000, 1.000000000000000000, 0.000000000000000000 ) ) ;
#21332 = CARTESIAN_POINT ( 'NONE',  ( 28.99662776679782539, 40.00000000000000000, -58.58186007941694129 ) ) ;
#21333 = EDGE_CURVE ( 'NONE', #31625, #21277, #9757, .T. ) ;
#21334 = CARTESIAN_POINT ( 'NONE',  ( 17.99999999999999645, -26.29521155129837595, -17.34211205339375184 ) ) ;
#21335 = CARTESIAN_POINT ( 'NONE',  ( 17.99999999999999645, -110.3490479609633752, 20.28201389785361641 ) ) ;
#21336 = ORIENTED_EDGE ( 'NONE', *, *, #21991, .F. ) ;
#21337 = CYLINDRICAL_SURFACE ( 'NONE', #13329, 59.00000000000000000 ) ;
#21338 = ORIENTED_EDGE ( 'NONE', *, *, #5000, .F. ) ;
#21339 = AXIS2_PLACEMENT_3D ( 'NONE', #32764, #42368, #9651 ) ;
#21340 = DIRECTION ( 'NONE',  ( 0.000000000000000000, -0.6845471059286792892, -0.7289686274214203232 ) ) ;
#21341 = DIRECTION ( 'NONE',  ( 1.000000000000000000, 0.000000000000000000, -0.000000000000000000 ) ) ;
#21342 = CARTESIAN_POINT ( 'NONE',  ( -25.79802671946675474, 31.00000000000000355, 52.34090327860478453 ) ) ;
#21343 = DIRECTION ( 'NONE',  ( 1.000000000000000000, 0.000000000000000000, 0.000000000000000000 ) ) ;
#21344 = ORIENTED_EDGE ( 'NONE', *, *, #34353, .T. ) ;
#21345 = AXIS2_PLACEMENT_3D ( 'NONE', #39706, #26864, #39499 ) ;
#21346 = LINE ( 'NONE', #27649, #7999 ) ;
#21347 = ORIENTED_EDGE ( 'NONE', *, *, #43055, .F. ) ;
#21348 = CARTESIAN_POINT ( 'NONE',  ( -9.022452542771789652, 40.00000000000000000, 26.59230923919664491 ) ) ;
#21349 = CIRCLE ( 'NONE', #15746, 20.00000000000000711 ) ;
#21350 = VERTEX_POINT ( 'NONE', #36146 ) ;
#21352 = AXIS2_PLACEMENT_3D ( 'NONE', #20685, #30692, #11064 ) ;
#21351 = CARTESIAN_POINT ( 'NONE',  ( 17.99999999999999645, 94.52951811191560694, 67.23221107124935259 ) ) ;
#21353 = DIRECTION ( 'NONE',  ( -1.000000000000000000, -0.000000000000000000, -0.000000000000000000 ) ) ;
#21354 = CARTESIAN_POINT ( 'NONE',  ( -70.49178429274641644, 31.00000000000000711, 40.57739572807859929 ) ) ;
#21355 = CARTESIAN_POINT ( 'NONE',  ( 37.87019299813560025, 40.00000000000000000, -76.55254356380190472 ) ) ;
#21356 = EDGE_CURVE ( 'NONE', #952, #38711, #3816, .T. ) ;
#21357 = EDGE_CURVE ( 'NONE', #34854, #36509, #4555, .T. ) ;
#21358 = AXIS2_PLACEMENT_3D ( 'NONE', #17016, #30301, #374 ) ;
#21359 = LINE ( 'NONE', #8223, #2083 ) ;
#21360 = EDGE_CURVE ( 'NONE', #39420, #21974, #33806, .T. ) ;
#21361 = CIRCLE ( 'NONE', #38024, 36.00000000000000000 ) ;
#21362 = ORIENTED_EDGE ( 'NONE', *, *, #19449, .F. ) ;
#21363 = DIRECTION ( 'NONE',  ( -1.000000000000000000, 0.000000000000000000, -0.000000000000000000 ) ) ;
#21364 = ORIENTED_EDGE ( 'NONE', *, *, #19754, .T. ) ;
#21365 = DIRECTION ( 'NONE',  ( 1.000000000000000000, 0.000000000000000000, 0.000000000000000000 ) ) ;
#21366 = DIRECTION ( 'NONE',  ( -1.000000000000000000, -0.000000000000000000, 0.000000000000000000 ) ) ;
#21368 = ORIENTED_EDGE ( 'NONE', *, *, #38246, .F. ) ;
#21367 = LINE ( 'NONE', #1881, #8832 ) ;
#21369 = CARTESIAN_POINT ( 'NONE',  ( 0.000000000000000000, 0.000000000000000000, 0.000000000000000000 ) ) ;
#21370 = ORIENTED_EDGE ( 'NONE', *, *, #7276, .F. ) ;
#21371 = CARTESIAN_POINT ( 'NONE',  ( 17.99999999999999645, -109.1131968883996848, -26.12628443612003437 ) ) ;
#21372 = CARTESIAN_POINT ( 'NONE',  ( -96.39699453480135105, 40.00000000000000711, 25.82690913164849889 ) ) ;
#21373 = CARTESIAN_POINT ( 'NONE',  ( 18.00000000000000355, -5.871425383721165403, -51.66745943012288222 ) ) ;
#21374 = VERTEX_POINT ( 'NONE', #15691 ) ;
#21375 = EDGE_CURVE ( 'NONE', #36059, #25122, #15745, .T. ) ;
#21376 = LINE ( 'NONE', #24423, #20005 ) ;
#21377 = DIRECTION ( 'NONE',  ( 0.000000000000000000, 0.000000000000000000, -1.000000000000000000 ) ) ;
#21378 = VECTOR ( 'NONE', #26709, 1000.000000000000114 ) ;
#21379 = CIRCLE ( 'NONE', #15068, 120.5010000000000190 ) ;
#21380 = AXIS2_PLACEMENT_3D ( 'NONE', #32494, #42511, #31867 ) ;
#21381 = VECTOR ( 'NONE', #41349, 1000.000000000000000 ) ;
#21383 = DIRECTION ( 'NONE',  ( 1.000000000000000000, 0.000000000000000000, 0.000000000000000000 ) ) ;
#21382 = DIRECTION ( 'NONE',  ( 1.000000000000000000, 0.000000000000000000, 0.000000000000000000 ) ) ;
#21384 = VERTEX_POINT ( 'NONE', #31667 ) ;
#21385 = CARTESIAN_POINT ( 'NONE',  ( 17.99999999999999645, -92.25992191227339845, -77.51514567967485902 ) ) ;
#21386 = ORIENTED_EDGE ( 'NONE', *, *, #15255, .T. ) ;
#21387 = CYLINDRICAL_SURFACE ( 'NONE', #12672, 2.649999999999971934 ) ;
#21388 = CARTESIAN_POINT ( 'NONE',  ( -16.82630558382439290, 40.00000000000000000, -29.24196894321155682 ) ) ;
#21389 = CIRCLE ( 'NONE', #35240, 120.5010000000000190 ) ;
#21390 = DIRECTION ( 'NONE',  ( 0.000000000000000000, 0.000000000000000000, 1.000000000000000000 ) ) ;
#21391 = VECTOR ( 'NONE', #34592, 1000.000000000000000 ) ;
#21392 = VECTOR ( 'NONE', #32889, 1000.000000000000000 ) ;
#21393 = FACE_OUTER_BOUND ( 'NONE', #7238, .T. ) ;
#21394 = EDGE_CURVE ( 'NONE', #21299, #41436, #13654, .T. ) ;
#21395 = DIRECTION ( 'NONE',  ( 0.000000000000000000, 0.000000000000000000, 1.000000000000000000 ) ) ;
#21396 = ORIENTED_EDGE ( 'NONE', *, *, #32860, .F. ) ;
#21398 = CARTESIAN_POINT ( 'NONE',  ( 4.141042297810615835, -2.227970268150433863, -3.687027686973623819 ) ) ;
#21397 = DIRECTION ( 'NONE',  ( 1.000000000000000000, 0.000000000000000000, 0.000000000000000000 ) ) ;
#21400 = ORIENTED_EDGE ( 'NONE', *, *, #23157, .F. ) ;
#21399 = VECTOR ( 'NONE', #1452, 1000.000000000000000 ) ;
#21401 = DIRECTION ( 'NONE',  ( -3.996523416598930318E-16, 2.658563593772947863E-15, 1.000000000000000000 ) ) ;
#21402 = CARTESIAN_POINT ( 'NONE',  ( 9.000000000000000000, 7.220349212960960550, -35.26849241522656087 ) ) ;
#21403 = CARTESIAN_POINT ( 'NONE',  ( 11.68784703496123711, 31.00000000000000355, -20.25319168173327355 ) ) ;
#21404 = ORIENTED_EDGE ( 'NONE', *, *, #17667, .F. ) ;
#21405 = DIRECTION ( 'NONE',  ( 1.000000000000000000, 0.000000000000000000, 0.000000000000000000 ) ) ;
#21406 = CARTESIAN_POINT ( 'NONE',  ( 17.99999999999999645, 53.40478689619876462, -108.0204598100360016 ) ) ;
#21407 = DIRECTION ( 'NONE',  ( 0.000000000000000000, -0.3641605752528101481, -0.9313361774523430947 ) ) ;
#21408 = CARTESIAN_POINT ( 'NONE',  ( -10.16518460146908787, 31.00000000000000355, 77.20874865269769316 ) ) ;
#21409 = ORIENTED_EDGE ( 'NONE', *, *, #12460, .F. ) ;
#21410 = CARTESIAN_POINT ( 'NONE',  ( -3.469229457552013507, 31.00000000000000355, -54.39987425099493379 ) ) ;
#21411 = ADVANCED_FACE ( 'NONE', ( #8324 ), #24957, .T. ) ;
#21412 = AXIS2_PLACEMENT_3D ( 'NONE', #5710, #42560, #12501 ) ;
#21413 = CARTESIAN_POINT ( 'NONE',  ( -89.21153162435624040, 40.00000000000000711, 11.76024306507019901 ) ) ;
#21414 = AXIS2_PLACEMENT_3D ( 'NONE', #28120, #2108, #5819 ) ;
#21415 = AXIS2_PLACEMENT_3D ( 'NONE', #35244, #42428, #25262 ) ;
#21416 = ORIENTED_EDGE ( 'NONE', *, *, #13740, .T. ) ;
#21417 = AXIS2_PLACEMENT_3D ( 'NONE', #29961, #12522, #36461 ) ;
#21418 = DIRECTION ( 'NONE',  ( 0.000000000000000000, 2.587384167558627638E-15, -1.000000000000000000 ) ) ;
#21419 = CARTESIAN_POINT ( 'NONE',  ( -91.96080130434583566, -2.055254544495720648, 14.45886780445738395 ) ) ;
#21420 = CARTESIAN_POINT ( 'NONE',  ( 17.99999999999999645, 46.83041522348496954, 101.9567785075603155 ) ) ;
#21421 = CIRCLE ( 'NONE', #24209, 59.00000000000000711 ) ;
#21423 = ORIENTED_EDGE ( 'NONE', *, *, #42382, .T. ) ;
#21422 = DIRECTION ( 'NONE',  ( 0.000000000000000000, 0.000000000000000000, 1.000000000000000000 ) ) ;
#21424 = CARTESIAN_POINT ( 'NONE',  ( 17.99999999999999645, -29.02167576844178853, 108.3790330702168774 ) ) ;
#21425 = DIRECTION ( 'NONE',  ( 0.000000000000000000, 0.000000000000000000, 1.000000000000000000 ) ) ;
#21426 = EDGE_CURVE ( 'NONE', #17650, #17796, #21683, .T. ) ;
#21427 = ORIENTED_EDGE ( 'NONE', *, *, #1299, .F. ) ;
#21428 = CARTESIAN_POINT ( 'NONE',  ( 29.59587406094124873, 40.00000000000000000, 60.01321678176139329 ) ) ;
#21429 = CARTESIAN_POINT ( 'NONE',  ( 8.999999999999998224, 23.79363200506953291, 27.01597816121656237 ) ) ;
#21430 = VECTOR ( 'NONE', #37634, 1000.000000000000000 ) ;
#21431 = ORIENTED_EDGE ( 'NONE', *, *, #1550, .F. ) ;
#21432 = ADVANCED_FACE ( 'NONE', ( #24727 ), #38009, .T. ) ;
#21433 = DIRECTION ( 'NONE',  ( 1.000000000000000000, -0.000000000000000000, -0.000000000000000000 ) ) ;
#21434 = CARTESIAN_POINT ( 'NONE',  ( 18.00000000000000355, -2.123073309834832667, -47.45152853935337589 ) ) ;
#21435 = AXIS2_PLACEMENT_3D ( 'NONE', #20416, #3348, #10353 ) ;
#21436 = EDGE_LOOP ( 'NONE', ( #16583, #20017, #40046, #32258 ) ) ;
#21437 = DIRECTION ( 'NONE',  ( -1.000000000000000000, 0.000000000000000000, -0.000000000000000000 ) ) ;
#21438 = VERTEX_POINT ( 'NONE', #5263 ) ;
#21439 = CARTESIAN_POINT ( 'NONE',  ( 33.90854556226734218, -40.05525454449572464, -74.83297477053821467 ) ) ;
#21440 = ORIENTED_EDGE ( 'NONE', *, *, #19528, .T. ) ;
#21441 = CARTESIAN_POINT ( 'NONE',  ( 17.99999999999999645, 0.000000000000000000, 0.000000000000000000 ) ) ;
#21442 = DIRECTION ( 'NONE',  ( 1.000000000000000000, 0.000000000000000000, 0.000000000000000000 ) ) ;
#21443 = VERTEX_POINT ( 'NONE', #41034 ) ;
#21444 = AXIS2_PLACEMENT_3D ( 'NONE', #1444, #8000, #41806 ) ;
#21445 = CARTESIAN_POINT ( 'NONE',  ( 0.000000000000000000, 42.60732521687599217, -19.80331771201614544 ) ) ;
#21446 = CARTESIAN_POINT ( 'NONE',  ( 0.000000000000000000, -49.65209126885751800, -15.44894276735603356 ) ) ;
#21447 = ORIENTED_EDGE ( 'NONE', *, *, #29480, .F. ) ;
#21448 = AXIS2_PLACEMENT_3D ( 'NONE', #24781, #41520, #21734 ) ;
#21449 = CYLINDRICAL_SURFACE ( 'NONE', #21081, 20.00000000000000355 ) ;
#21450 = EDGE_CURVE ( 'NONE', #2020, #5449, #42852, .T. ) ;
#21451 = AXIS2_PLACEMENT_3D ( 'NONE', #22313, #22732, #42321 ) ;
#21453 = DIRECTION ( 'NONE',  ( 0.000000000000000000, 0.000000000000000000, 1.000000000000000000 ) ) ;
#21452 = AXIS2_PLACEMENT_3D ( 'NONE', #24471, #14419, #38958 ) ;
#21454 = ORIENTED_EDGE ( 'NONE', *, *, #4766, .T. ) ;
#21455 = LINE ( 'NONE', #31875, #31548 ) ;
#21456 = CIRCLE ( 'NONE', #14478, 2.100000000000000089 ) ;
#21457 = CARTESIAN_POINT ( 'NONE',  ( 17.99999999999999645, -103.5682682299985515, -43.14958040911633219 ) ) ;
#21458 = PRODUCT_CONTEXT ( 'NONE', #40067, 'mechanical' ) ;
#21459 = FACE_OUTER_BOUND ( 'NONE', #6243, .T. ) ;
#21460 = CARTESIAN_POINT ( 'NONE',  ( -42.66459923921424036, 31.00000000000000355, 24.64557685607233140 ) ) ;
#21461 = VERTEX_POINT ( 'NONE', #35143 ) ;
#21463 = LINE ( 'NONE', #29465, #2416 ) ;
#21462 = FACE_OUTER_BOUND ( 'NONE', #17356, .T. ) ;
#21464 = DIRECTION ( 'NONE',  ( 0.000000000000000000, 0.9618256431728199329, -0.2736629900720800590 ) ) ;
#21465 = EDGE_LOOP ( 'NONE', ( #19019, #31555, #1471, #19478 ) ) ;
#21466 = CARTESIAN_POINT ( 'NONE',  ( -6.199999999999997513, 4.693303851024319376E-15, 0.000000000000000000 ) ) ;
#21467 = CARTESIAN_POINT ( 'NONE',  ( 61.18335543008118549, 39.99999999999999289, -20.78249587198964576 ) ) ;
#21468 = EDGE_CURVE ( 'NONE', #42039, #1458, #5258, .T. ) ;
#21469 = CARTESIAN_POINT ( 'NONE',  ( 15.22596115864829969, 40.00000000000000000, 57.21640888977480444 ) ) ;
#21470 = DIRECTION ( 'NONE',  ( 3.009274222672345096E-17, 1.000000000000000000, -2.455023325076454960E-18 ) ) ;
#21471 = CARTESIAN_POINT ( 'NONE',  ( 106.9999999999993321, -2.424707662641754077E-13, -32.00000000000000000 ) ) ;
#21472 = VECTOR ( 'NONE', #34997, 1000.000000000000000 ) ;
#21473 = DIRECTION ( 'NONE',  ( 1.000000000000000000, 0.000000000000000000, 0.000000000000000000 ) ) ;
#21474 = CARTESIAN_POINT ( 'NONE',  ( 0.000000000000000000, 0.000000000000000000, 0.000000000000000000 ) ) ;
#21475 = AXIS2_PLACEMENT_3D ( 'NONE', #42789, #26463, #3716 ) ;
#21476 = EDGE_CURVE ( 'NONE', #12372, #13830, #41469, .T. ) ;
#21477 = CIRCLE ( 'NONE', #12385, 120.5010000000000474 ) ;
#21478 = VERTEX_POINT ( 'NONE', #34729 ) ;
#21479 = CARTESIAN_POINT ( 'NONE',  ( -16.93500259178182432, 40.00000000000000000, 34.36424406943201149 ) ) ;
#21480 = EDGE_LOOP ( 'NONE', ( #1353, #29488, #38525, #40715 ) ) ;
#21481 = FACE_OUTER_BOUND ( 'NONE', #39213, .T. ) ;
#21482 = DIRECTION ( 'NONE',  ( 1.000000000000000000, 0.000000000000000000, 0.000000000000000000 ) ) ;
#21483 = CIRCLE ( 'NONE', #29101, 10.99999999999998934 ) ;
#21484 = AXIS2_PLACEMENT_3D ( 'NONE', #15600, #11691, #31528 ) ;
#21485 = VERTEX_POINT ( 'NONE', #7885 ) ;
#21486 = CIRCLE ( 'NONE', #13108, 59.00000000000000000 ) ;
#21487 = DIRECTION ( 'NONE',  ( 1.000000000000000000, 0.000000000000000000, 0.000000000000000000 ) ) ;
#21488 = LINE ( 'NONE', #13835, #35252 ) ;
#21489 = EDGE_LOOP ( 'NONE', ( #25221, #18081, #8830, #16859 ) ) ;
#21490 = CARTESIAN_POINT ( 'NONE',  ( 17.99999999999999645, 0.000000000000000000, 0.000000000000000000 ) ) ;
#21491 = ORIENTED_EDGE ( 'NONE', *, *, #1300, .F. ) ;
#21492 = ORIENTED_EDGE ( 'NONE', *, *, #11073, .F. ) ;
#21493 = DIRECTION ( 'NONE',  ( 0.000000000000000000, 0.000000000000000000, 1.000000000000000000 ) ) ;
#21494 = VECTOR ( 'NONE', #4252, 1000.000000000000000 ) ;
#21495 = CARTESIAN_POINT ( 'NONE',  ( 8.965261019430212031, 31.00000000000000355, 68.85524230650666766 ) ) ;
#21496 = VERTEX_POINT ( 'NONE', #38414 ) ;
#21497 = CARTESIAN_POINT ( 'NONE',  ( -4.000000000000000000, 1.700094919196744270, -3.320312364301766017 ) ) ;
#21498 = CARTESIAN_POINT ( 'NONE',  ( 8.999999999999998224, 114.1157422997283248, 20.82300072952973480 ) ) ;
#21499 = ORIENTED_EDGE ( 'NONE', *, *, #12439, .F. ) ;
#21500 = FACE_OUTER_BOUND ( 'NONE', #39897, .T. ) ;
#21501 = ORIENTED_EDGE ( 'NONE', *, *, #39545, .T. ) ;
#21502 = CARTESIAN_POINT ( 'NONE',  ( 5.735608225908777946, 40.00000000000000000, 89.40012361736363289 ) ) ;
#21503 = EDGE_CURVE ( 'NONE', #38187, #14447, #9310, .T. ) ;
#21504 = CARTESIAN_POINT ( 'NONE',  ( 18.71272080434062701, 31.00000000000000355, 21.38210947162711406 ) ) ;
#21505 = EDGE_CURVE ( 'NONE', #7227, #30398, #10719, .T. ) ;
#21506 = AXIS2_PLACEMENT_3D ( 'NONE', #22376, #25650, #2665 ) ;
#21508 = FACE_OUTER_BOUND ( 'NONE', #28281, .T. ) ;
#21507 = DIRECTION ( 'NONE',  ( -1.000000000000000000, 0.000000000000000000, 0.000000000000000000 ) ) ;
#21509 = CARTESIAN_POINT ( 'NONE',  ( 17.99999999999999645, 111.1352304691227744, 15.40237066878635730 ) ) ;
#21510 = DIRECTION ( 'NONE',  ( 1.000000000000000000, 0.000000000000000000, -0.000000000000000000 ) ) ;
#21511 = CIRCLE ( 'NONE', #33287, 52.00000000000000000 ) ;
#21512 = ORIENTED_EDGE ( 'NONE', *, *, #36895, .F. ) ;
#21513 = AXIS2_PLACEMENT_3D ( 'NONE', #30345, #3681, #30572 ) ;
#21514 = VECTOR ( 'NONE', #34970, 1000.000000000000000 ) ;
#21515 = DIRECTION ( 'NONE',  ( -1.000000000000000000, 0.000000000000000000, 0.000000000000000000 ) ) ;
#21516 = CIRCLE ( 'NONE', #37456, 20.00000000000000711 ) ;
#21517 = ORIENTED_EDGE ( 'NONE', *, *, #32955, .T. ) ;
#21518 = DIRECTION ( 'NONE',  ( -1.000000000000000000, -0.000000000000000000, -0.000000000000000000 ) ) ;
#21519 = CARTESIAN_POINT ( 'NONE',  ( 94.17930118497612568, 31.00000000000000000, -12.41473344271720691 ) ) ;
#21520 = DIRECTION ( 'NONE',  ( 1.000000000000000000, 0.000000000000000000, 0.000000000000000000 ) ) ;
#21522 = EDGE_LOOP ( 'NONE', ( #380, #40164, #15667, #17930 ) ) ;
#21521 = CIRCLE ( 'NONE', #23582, 14.70000000000000107 ) ;
#21523 = CARTESIAN_POINT ( 'NONE',  ( -27.06829236441420861, 40.00000000000000000, 15.58100167311933149 ) ) ;
#21524 = EDGE_LOOP ( 'NONE', ( #4514, #870, #42287, #20786 ) ) ;
#21525 = EDGE_LOOP ( 'NONE', ( #8676, #38458 ) ) ;
#21526 = CARTESIAN_POINT ( 'NONE',  ( 8.999999999999998224, 0.000000000000000000, 11.08000000000000007 ) ) ;
#21527 = DIRECTION ( 'NONE',  ( -0.000000000000000000, -0.000000000000000000, 1.000000000000000000 ) ) ;
#21528 = CARTESIAN_POINT ( 'NONE',  ( -109.0695705685748607, -106.4195705685759776, 9.999999999999998224 ) ) ;
#21529 = DIRECTION ( 'NONE',  ( 0.000000000000000000, -0.4610925014493326146, 0.8873520750565681015 ) ) ;
#21530 = EDGE_CURVE ( 'NONE', #34259, #1680, #32297, .T. ) ;
#21531 = VERTEX_POINT ( 'NONE', #15337 ) ;
#21532 = FACE_OUTER_BOUND ( 'NONE', #13349, .T. ) ;
#21533 = ORIENTED_EDGE ( 'NONE', *, *, #17547, .T. ) ;
#21534 = CARTESIAN_POINT ( 'NONE',  ( 9.000000000000000000, 35.78425302087543969, -3.935382540232422510 ) ) ;
#21535 = CARTESIAN_POINT ( 'NONE',  ( 0.000000000000000000, 0.000000000000000000, 0.000000000000000000 ) ) ;
#21536 = EDGE_CURVE ( 'NONE', #31395, #21384, #20504, .T. ) ;
#21537 = AXIS2_PLACEMENT_3D ( 'NONE', #28842, #41703, #21895 ) ;
#21538 = DIRECTION ( 'NONE',  ( -1.000000000000000000, 0.000000000000000000, 0.000000000000000000 ) ) ;
#21539 = CYLINDRICAL_SURFACE ( 'NONE', #25456, 120.5010000000000190 ) ;
#21540 = ORIENTED_EDGE ( 'NONE', *, *, #23903, .F. ) ;
#21541 = VERTEX_POINT ( 'NONE', #1551 ) ;
#21542 = DIRECTION ( 'NONE',  ( -1.000000000000000000, -0.000000000000000000, 0.000000000000000000 ) ) ;
#21543 = AXIS2_PLACEMENT_3D ( 'NONE', #22269, #31842, #1710 ) ;
#21544 = CARTESIAN_POINT ( 'NONE',  ( 9.000000000000001776, -112.5220807139885864, 28.19186676675806424 ) ) ;
#21545 = CIRCLE ( 'NONE', #31249, 18.77999999999999403 ) ;
#21546 = AXIS2_PLACEMENT_3D ( 'NONE', #36051, #6170, #16447 ) ;
#21547 = ORIENTED_EDGE ( 'NONE', *, *, #18739, .F. ) ;
#21549 = ORIENTED_EDGE ( 'NONE', *, *, #21797, .T. ) ;
#21548 = DIRECTION ( 'NONE',  ( 0.000000000000000000, 0.000000000000000000, 1.000000000000000000 ) ) ;
#21550 = CARTESIAN_POINT ( 'NONE',  ( 5.076274692534474831, 31.00000000000000355, 39.04542013319161953 ) ) ;
#21551 = CARTESIAN_POINT ( 'NONE',  ( -153.1499999999986414, -2.881448370824816841E-13, 10.00000000000004619 ) ) ;
#21552 = CIRCLE ( 'NONE', #15173, 13.59999999999999964 ) ;
#21554 = CARTESIAN_POINT ( 'NONE',  ( 17.99999999999999645, 0.000000000000000000, 0.000000000000000000 ) ) ;
#21553 = DIRECTION ( 'NONE',  ( -1.000000000000000000, 0.000000000000000000, 0.000000000000000000 ) ) ;
#21555 = ORIENTED_EDGE ( 'NONE', *, *, #4045, .F. ) ;
#21556 = CYLINDRICAL_SURFACE ( 'NONE', #17965, 59.00000000000000000 ) ;
#21557 = CARTESIAN_POINT ( 'NONE',  ( 18.91139405008128804, 40.00000000000000000, 55.99505798892768382 ) ) ;
#21558 = ADVANCED_FACE ( 'NONE', ( #28629 ), #41902, .F. ) ;
#21559 = ADVANCED_FACE ( 'NONE', ( #35363 ), #4608, .T. ) ;
#21560 = CYLINDRICAL_SURFACE ( 'NONE', #33239, 59.00000000000000000 ) ;
#21561 = EDGE_CURVE ( 'NONE', #30653, #42446, #37177, .T. ) ;
#21562 = EDGE_CURVE ( 'NONE', #15819, #17013, #1115, .T. ) ;
#21563 = EDGE_CURVE ( 'NONE', #30041, #27914, #27424, .T. ) ;
#21564 = CARTESIAN_POINT ( 'NONE',  ( 0.000000000000000000, 41.33768078145502756, 104.3046912715542902 ) ) ;
#21565 = ORIENTED_EDGE ( 'NONE', *, *, #27559, .T. ) ;
#21566 = DIRECTION ( 'NONE',  ( 3.009274222672345096E-17, 1.000000000000000000, -2.455023325076454960E-18 ) ) ;
#21567 = ORIENTED_EDGE ( 'NONE', *, *, #34192, .T. ) ;
#21568 = DIRECTION ( 'NONE',  ( -3.996523416598930318E-16, 2.658563593772947863E-15, 1.000000000000000000 ) ) ;
#21569 = CARTESIAN_POINT ( 'NONE',  ( 17.99999999999999645, 31.17727234463695041, 111.7317219465820983 ) ) ;
#21570 = CARTESIAN_POINT ( 'NONE',  ( -4.745113895469965648, 31.00000000000000355, -72.39583333427917466 ) ) ;
#21571 = AXIS2_PLACEMENT_3D ( 'NONE', #26426, #13556, #42973 ) ;
#21572 = DIRECTION ( 'NONE',  ( 1.000000000000000000, 0.000000000000000000, 0.000000000000000000 ) ) ;
#21573 = CIRCLE ( 'NONE', #1974, 59.00000000000000000 ) ;
#21574 = VERTEX_POINT ( 'NONE', #39248 ) ;
#21575 = VECTOR ( 'NONE', #34786, 1000.000000000000000 ) ;
#21576 = DIRECTION ( 'NONE',  ( 1.000000000000000000, -0.000000000000000000, -0.000000000000000000 ) ) ;
#21577 = ORIENTED_EDGE ( 'NONE', *, *, #20546, .T. ) ;
#21578 = CYLINDRICAL_SURFACE ( 'NONE', #43046, 51.99999999999999289 ) ;
#21579 = LINE ( 'NONE', #15233, #33155 ) ;
#21580 = CARTESIAN_POINT ( 'NONE',  ( 77.59064570035201314, 31.00000000000000000, -38.12735739514867817 ) ) ;
#21581 = CARTESIAN_POINT ( 'NONE',  ( -54.99468034528496929, 40.00000000000000000, -62.86974495748533087 ) ) ;
#21582 = CARTESIAN_POINT ( 'NONE',  ( 0.000000000000000000, -1.178949249685214307, 2.042000000000001592 ) ) ;
#21583 = EDGE_CURVE ( 'NONE', #14728, #4296, #29264, .T. ) ;
#21584 = ORIENTED_EDGE ( 'NONE', *, *, #20848, .F. ) ;
#21585 = CARTESIAN_POINT ( 'NONE',  ( 17.99999999999999645, 112.8457601792515419, 26.86697618949414945 ) ) ;
#21586 = ORIENTED_EDGE ( 'NONE', *, *, #17722, .T. ) ;
#21587 = DIRECTION ( 'NONE',  ( 0.9914448613738107152, -0.1305261922200494362, 0.000000000000000000 ) ) ;
#21588 = CARTESIAN_POINT ( 'NONE',  ( -132.0000507999999968, 1.347111479062088405E-15, 11.00000000000000000 ) ) ;
#21590 = ORIENTED_EDGE ( 'NONE', *, *, #39009, .T. ) ;
#21589 = DIRECTION ( 'NONE',  ( 1.000000000000000000, 0.000000000000000000, 0.000000000000000000 ) ) ;
#21591 = CARTESIAN_POINT ( 'NONE',  ( 0.000000000000000000, 0.000000000000000000, 0.000000000000000000 ) ) ;
#21592 = ORIENTED_EDGE ( 'NONE', *, *, #26033, .F. ) ;
#21593 = DIRECTION ( 'NONE',  ( 1.000000000000000000, 0.000000000000000000, 0.000000000000000000 ) ) ;
#21594 = CARTESIAN_POINT ( 'NONE',  ( 6.381360069253262601, 40.00000000000000000, 97.39583333395333398 ) ) ;
#21595 = DIRECTION ( 'NONE',  ( 0.000000000000000000, 0.2631025642275152676, 0.9647678688145175929 ) ) ;
#21596 = ORIENTED_EDGE ( 'NONE', *, *, #30551, .T. ) ;
#21597 = CARTESIAN_POINT ( 'NONE',  ( 18.00000000000000355, 0.000000000000000000, 0.000000000000000000 ) ) ;
#21598 = CIRCLE ( 'NONE', #35455, 120.5010000000000190 ) ;
#21599 = CARTESIAN_POINT ( 'NONE',  ( -8.749793197483592522, 117.9447454555042754, 2.972870684497274762 ) ) ;
#21601 = CARTESIAN_POINT ( 'NONE',  ( 0.000000000000000000, 9.744342220503391161, 46.48873837489801275 ) ) ;
#21600 = CARTESIAN_POINT ( 'NONE',  ( 0.000000000000000000, -110.0562500189201955, 49.07252625220073838 ) ) ;
#21602 = ORIENTED_EDGE ( 'NONE', *, *, #8917, .T. ) ;
#21603 = LINE ( 'NONE', #34853, #38623 ) ;
#21604 = VERTEX_POINT ( 'NONE', #35567 ) ;
#21605 = DIRECTION ( 'NONE',  ( -3.996523416598930318E-16, 2.658563593772947863E-15, 1.000000000000000000 ) ) ;
#21606 = CARTESIAN_POINT ( 'NONE',  ( 4.597210615070504325, 40.00000000000000000, -34.47704375835832025 ) ) ;
#21607 = DIRECTION ( 'NONE',  ( -1.000000000000000000, 0.000000000000000000, 0.000000000000000000 ) ) ;
#21608 = EDGE_CURVE ( 'NONE', #15182, #20449, #22525, .T. ) ;
#21609 = CARTESIAN_POINT ( 'NONE',  ( 18.00000000000000355, -17.08890430202782085, 43.76671000081940122 ) ) ;
#21610 = ADVANCED_FACE ( 'NONE', ( #36412 ), #9174, .F. ) ;
#21611 = EDGE_CURVE ( 'NONE', #1993, #24221, #15541, .T. ) ;
#21612 = CARTESIAN_POINT ( 'NONE',  ( 0.000000000000000000, 0.000000000000000000, 0.000000000000000000 ) ) ;
#21613 = EDGE_LOOP ( 'NONE', ( #6396, #42291, #32081, #3967 ) ) ;
#21614 = DIRECTION ( 'NONE',  ( 1.000000000000000000, 0.000000000000000000, 0.000000000000000000 ) ) ;
#21615 = EDGE_CURVE ( 'NONE', #12218, #5335, #28150, .T. ) ;
#21616 = ORIENTED_EDGE ( 'NONE', *, *, #13001, .F. ) ;
#21617 = DIRECTION ( 'NONE',  ( -3.996523416598930318E-16, 2.658563593772947863E-15, 1.000000000000000000 ) ) ;
#21618 = DIRECTION ( 'NONE',  ( -1.000000000000000000, 0.000000000000000000, -0.000000000000000000 ) ) ;
#21619 = CARTESIAN_POINT ( 'NONE',  ( 1.799870782497353439, 31.00000000000000355, 27.39583333577991908 ) ) ;
#21620 = EDGE_LOOP ( 'NONE', ( #29353, #20234, #16187, #16102 ) ) ;
#21621 = DIRECTION ( 'NONE',  ( -1.000000000000000000, -0.000000000000000000, -0.000000000000000000 ) ) ;
#21622 = EDGE_CURVE ( 'NONE', #4984, #19384, #5823, .T. ) ;
#21623 = CARTESIAN_POINT ( 'NONE',  ( 17.99999999999999645, -8.827181066046698277, 120.1772519049559378 ) ) ;
#21624 = CARTESIAN_POINT ( 'NONE',  ( 50.46169669344906339, 31.00000000000000355, 57.51940134901310131 ) ) ;
#21625 = AXIS2_PLACEMENT_3D ( 'NONE', #4300, #811, #11531 ) ;
#21626 = AXIS2_PLACEMENT_3D ( 'NONE', #40189, #20393, #33653 ) ;
#21627 = ORIENTED_EDGE ( 'NONE', *, *, #21476, .F. ) ;
#21628 = CARTESIAN_POINT ( 'NONE',  ( 36.84045577241590763, 31.00000000000000355, -41.86038302678687018 ) ) ;
#21629 = CARTESIAN_POINT ( 'NONE',  ( 82.68608547523962216, 39.99999999999999289, 22.14036602612658200 ) ) ;
#21630 = CIRCLE ( 'NONE', #12527, 59.00000000000000000 ) ;
#21631 = ORIENTED_EDGE ( 'NONE', *, *, #8859, .T. ) ;
#21632 = DIRECTION ( 'NONE',  ( 0.000000000000000000, 0.000000000000000000, 1.000000000000000000 ) ) ;
#21633 = CARTESIAN_POINT ( 'NONE',  ( 17.99999999999999645, 41.33768078145642022, -104.3046912715537076 ) ) ;
#21634 = DIRECTION ( 'NONE',  ( -1.000000000000000000, 0.000000000000000000, 0.000000000000000000 ) ) ;
#21635 = ADVANCED_FACE ( 'NONE', ( #13123 ), #19039, .F. ) ;
#21637 = ORIENTED_EDGE ( 'NONE', *, *, #29001, .T. ) ;
#21636 = DIRECTION ( 'NONE',  ( -1.000000000000000000, 0.000000000000000000, 0.000000000000000000 ) ) ;
#21638 = CARTESIAN_POINT ( 'NONE',  ( 17.99999999999999645, 23.79363200506953291, 27.01597816121656237 ) ) ;
#21639 = DIRECTION ( 'NONE',  ( -1.000000000000000000, -0.000000000000000000, -0.000000000000000000 ) ) ;
#21640 = ORIENTED_EDGE ( 'NONE', *, *, #8276, .F. ) ;
#21641 = CARTESIAN_POINT ( 'NONE',  ( 8.201713468707295007, 40.00000000000000000, -62.30543997111072940 ) ) ;
#21642 = DIRECTION ( 'NONE',  ( 0.000000000000000000, -0.2631025642275089393, -0.9647678688145192583 ) ) ;
#21643 = ORIENTED_EDGE ( 'NONE', *, *, #43155, .T. ) ;
#21644 = DIRECTION ( 'NONE',  ( 0.000000000000000000, 0.000000000000000000, 1.000000000000000000 ) ) ;
#21645 = DIRECTION ( 'NONE',  ( 0.9247238835424298475, 0.000000000000000000, 0.3806385939525924744 ) ) ;
#21646 = ORIENTED_EDGE ( 'NONE', *, *, #8682, .T. ) ;
#21647 = DIRECTION ( 'NONE',  ( -1.000000000000000000, 0.000000000000000000, -0.000000000000000000 ) ) ;
#21648 = ORIENTED_EDGE ( 'NONE', *, *, #21907, .F. ) ;
#21649 = DIRECTION ( 'NONE',  ( -1.000000000000000000, 0.000000000000000000, 0.000000000000000000 ) ) ;
#21650 = ORIENTED_EDGE ( 'NONE', *, *, #17742, .F. ) ;
#21651 = DIRECTION ( 'NONE',  ( 0.000000000000000000, -0.2631025642275283127, 0.9647678688145140402 ) ) ;
#21652 = AXIS2_PLACEMENT_3D ( 'NONE', #27010, #40282, #40927 ) ;
#21653 = DIRECTION ( 'NONE',  ( -1.000000000000000000, 3.469446951953611724E-17, 0.000000000000000000 ) ) ;
#21654 = CIRCLE ( 'NONE', #18849, 125.9999999999993605 ) ;
#21655 = DIRECTION ( 'NONE',  ( 0.000000000000000000, 0.000000000000000000, 1.000000000000000000 ) ) ;
#21656 = ADVANCED_FACE ( 'NONE', ( #2382 ), #36204, .F. ) ;
#21657 = DIRECTION ( 'NONE',  ( -1.000000000000000000, -0.000000000000000000, -0.000000000000000000 ) ) ;
#21658 = B_SPLINE_CURVE_WITH_KNOTS ( 'NONE', 3,
 ( #36139, #19183, #39622, #19601, #22666, #26355 ),
 .UNSPECIFIED., .F., .F.,
 ( 4, 2, 4 ),
 ( -3.640115492409406142E-06, 0.0002066546034006526487, 0.0004169493222937146744 ),
 .UNSPECIFIED. ) ;
#21659 = VERTEX_POINT ( 'NONE', #15751 ) ;
#21660 = LINE ( 'NONE', #865, #9188 ) ;
#21661 = ADVANCED_FACE ( 'NONE', ( #29056 ), #29690, .F. ) ;
#21662 = DIRECTION ( 'NONE',  ( -3.009274222672345096E-17, -1.000000000000000000, 2.455023325076454960E-18 ) ) ;
#21663 = VERTEX_POINT ( 'NONE', #28836 ) ;
#21664 = DIRECTION ( 'NONE',  ( -1.000000000000000000, 0.000000000000000000, 0.000000000000000000 ) ) ;
#21665 = DIRECTION ( 'NONE',  ( -1.000000000000000000, -0.000000000000000000, -0.000000000000000000 ) ) ;
#21666 = EDGE_CURVE ( 'NONE', #26858, #13842, #35758, .T. ) ;
#21667 = APPLICATION_PROTOCOL_DEFINITION ( 'draft international standard', 'automotive_design', 1998, #41755 ) ;
#21668 = CARTESIAN_POINT ( 'NONE',  ( -21.03271207055027858, 31.00000000000000711, 3.044856699593506910 ) ) ;
#21669 = CARTESIAN_POINT ( 'NONE',  ( -31.39472673864601049, 31.00000000000000355, -40.91112553188754930 ) ) ;
#21670 = EDGE_LOOP ( 'NONE', ( #1771, #42140 ) ) ;
#21672 = DIRECTION ( 'NONE',  ( 1.000000000000000000, 0.000000000000000000, 0.000000000000000000 ) ) ;
#21671 = DIRECTION ( 'NONE',  ( -3.009274222672345096E-17, -1.000000000000000000, 2.455023325076454960E-18 ) ) ;
#21673 = EDGE_CURVE ( 'NONE', #20905, #4984, #42736, .T. ) ;
#21674 = EDGE_LOOP ( 'NONE', ( #23811, #31706, #11074, #11398 ) ) ;
#21675 = CARTESIAN_POINT ( 'NONE',  ( 48.45771864870608425, 40.00000000000000000, 27.97524394371832202 ) ) ;
#21676 = CARTESIAN_POINT ( 'NONE',  ( 17.81483206086863191, 40.00000000000000000, -52.17936214187551514 ) ) ;
#21677 = VECTOR ( 'NONE', #13385, 1000.000000000000000 ) ;
#21678 = AXIS2_PLACEMENT_3D ( 'NONE', #10819, #43093, #36537 ) ;
#21679 = CARTESIAN_POINT ( 'NONE',  ( 17.99999999999999645, -106.6051926090974007, 45.73109345704783379 ) ) ;
#21680 = LINE ( 'NONE', #12050, #27705 ) ;
#21681 = CIRCLE ( 'NONE', #18879, 116.0000000000000000 ) ;
#21682 = CIRCLE ( 'NONE', #36243, 116.0000000000000000 ) ;
#21683 = LINE ( 'NONE', #14466, #2455 ) ;
#21684 = CARTESIAN_POINT ( 'NONE',  ( -1.472621547668719444, 31.00000000000000355, -22.39583333634585571 ) ) ;
#21685 = ORIENTED_EDGE ( 'NONE', *, *, #9863, .F. ) ;
#21686 = CARTESIAN_POINT ( 'NONE',  ( -30.97228021248666607, 40.00000000000000000, 23.76985434021725041 ) ) ;
#21687 = ORIENTED_EDGE ( 'NONE', *, *, #12793, .T. ) ;
#21688 = CARTESIAN_POINT ( 'NONE',  ( 18.00000000000000355, 0.000000000000000000, 0.000000000000000000 ) ) ;
#21689 = DIRECTION ( 'NONE',  ( 0.000000000000000000, -0.7164567402983210709, 0.6976315211349786161 ) ) ;
#21690 = EDGE_LOOP ( 'NONE', ( #17816, #41145, #34526, #7941 ) ) ;
#21691 = DIRECTION ( 'NONE',  ( 0.02040816326530612776, 0.9997917317482359900, 0.000000000000000000 ) ) ;
#21692 = CARTESIAN_POINT ( 'NONE',  ( 0.000000000000000000, -95.31344542257689056, -66.11616384574544725 ) ) ;
#21693 = ORIENTED_EDGE ( 'NONE', *, *, #28876, .T. ) ;
#21694 = DIRECTION ( 'NONE',  ( 0.000000000000000000, 0.8951632913550635617, -0.4457383557765359772 ) ) ;
#21695 = ORIENTED_EDGE ( 'NONE', *, *, #40262, .T. ) ;
#21696 = ORIENTED_EDGE ( 'NONE', *, *, #28357, .T. ) ;
#21697 = LINE ( 'NONE', #24535, #9015 ) ;
#21699 = CIRCLE ( 'NONE', #40433, 25.00000000000000000 ) ;
#21698 = CARTESIAN_POINT ( 'NONE',  ( 53.86549405311983918, 31.00000000000000355, 70.40131829849023859 ) ) ;
#21700 = ORIENTED_EDGE ( 'NONE', *, *, #18466, .F. ) ;
#21701 = CARTESIAN_POINT ( 'NONE',  ( 0.000000000000000000, 0.000000000000000000, 0.000000000000000000 ) ) ;
#21702 = EDGE_CURVE ( 'NONE', #22603, #27398, #17010, .T. ) ;
#21703 = CIRCLE ( 'NONE', #29329, 31.49899999999999878 ) ;
#21704 = CARTESIAN_POINT ( 'NONE',  ( 17.99999999999999645, 0.000000000000000000, 0.000000000000000000 ) ) ;
#21705 = EDGE_CURVE ( 'NONE', #23222, #10037, #42731, .T. ) ;
#21706 = ORIENTED_EDGE ( 'NONE', *, *, #40806, .T. ) ;
#21707 = CARTESIAN_POINT ( 'NONE',  ( -5.384454397937118664, 6.594054843588581554E-16, -4.484454397937119197 ) ) ;
#21708 = ORIENTED_EDGE ( 'NONE', *, *, #41118, .T. ) ;
#21709 = DIRECTION ( 'NONE',  ( 1.000000000000000000, 0.000000000000000000, -0.000000000000000000 ) ) ;
#21710 = CIRCLE ( 'NONE', #23067, 13.59999999999999964 ) ;
#21711 = VECTOR ( 'NONE', #29547, 1000.000000000000000 ) ;
#21712 = CARTESIAN_POINT ( 'NONE',  ( -19.81637295874435978, 31.00000000000000355, -11.44243563873997793 ) ) ;
#21713 = CIRCLE ( 'NONE', #9106, 59.00000000000000000 ) ;
#21715 = CARTESIAN_POINT ( 'NONE',  ( 17.99999999999999645, -62.45178862086279992, 93.20969140437486544 ) ) ;
#21714 = DIRECTION ( 'NONE',  ( 0.000000000000000000, 0.000000000000000000, 1.000000000000000000 ) ) ;
#21716 = LINE ( 'NONE', #34760, #8117 ) ;
#21717 = DIRECTION ( 'NONE',  ( -1.000000000000000000, -0.000000000000000000, -0.000000000000000000 ) ) ;
#21718 = ORIENTED_EDGE ( 'NONE', *, *, #36641, .F. ) ;
#21719 = ADVANCED_FACE ( 'NONE', ( #12892, #22315 ), #16385, .F. ) ;
#21720 = SHAPE_REPRESENTATION_RELATIONSHIP ( 'NONE' , 'NONE' ,  #9026, #4160 ) ;
#21721 = CYLINDRICAL_SURFACE ( 'NONE', #9492, 120.5010000000000190 ) ;
#21722 = AXIS2_PLACEMENT_3D ( 'NONE', #3441, #19650, #23571 ) ;
#21723 = ORIENTED_EDGE ( 'NONE', *, *, #26998, .T. ) ;
#21724 = CARTESIAN_POINT ( 'NONE',  ( 18.00000000000000355, 41.20225022064669673, -23.63323037071358357 ) ) ;
#21725 = EDGE_CURVE ( 'NONE', #30619, #28909, #26056, .T. ) ;
#21726 = CARTESIAN_POINT ( 'NONE',  ( 58.84426737335365232, 31.00000000000000355, 76.69096868241209108 ) ) ;
#21727 = CARTESIAN_POINT ( 'NONE',  ( 0.000000000000000000, -19.47322409167291113, 30.27859877001393230 ) ) ;
#21728 = VERTEX_POINT ( 'NONE', #35761 ) ;
#21729 = EDGE_CURVE ( 'NONE', #11059, #25754, #10024, .T. ) ;
#21730 = CARTESIAN_POINT ( 'NONE',  ( -11.85532105537472880, 40.00000000000000000, -20.54123584193517260 ) ) ;
#21731 = VERTEX_POINT ( 'NONE', #13769 ) ;
#21732 = ORIENTED_EDGE ( 'NONE', *, *, #1366, .T. ) ;
#21733 = CARTESIAN_POINT ( 'NONE',  ( 0.000000000000000000, 48.55277268144470781, -105.3500273609075180 ) ) ;
#21734 = DIRECTION ( 'NONE',  ( 0.000000000000000000, 0.000000000000000000, 1.000000000000000000 ) ) ;
#21735 = CARTESIAN_POINT ( 'NONE',  ( 18.00000000000000355, 0.000000000000000000, 0.000000000000000000 ) ) ;
#21736 = CARTESIAN_POINT ( 'NONE',  ( 17.99999999999999645, 0.000000000000000000, 0.000000000000000000 ) ) ;
#21737 = EDGE_CURVE ( 'NONE', #23636, #14855, #19108, .T. ) ;
#21738 = EDGE_LOOP ( 'NONE', ( #9298, #32847 ) ) ;
#21739 = DIRECTION ( 'NONE',  ( 0.000000000000000000, 0.5528000653611945259, -0.8333139190825142872 ) ) ;
#21740 = ORIENTED_EDGE ( 'NONE', *, *, #11175, .F. ) ;
#21741 = CARTESIAN_POINT ( 'NONE',  ( 18.00000000000000355, 46.21320724403648939, 10.97699764141968970 ) ) ;
#21743 = EDGE_CURVE ( 'NONE', #755, #10605, #6966, .T. ) ;
#21742 = CIRCLE ( 'NONE', #40473, 59.00000000000001421 ) ;
#21744 = CARTESIAN_POINT ( 'NONE',  ( 0.000000000000000000, 0.000000000000000000, 0.000000000000000000 ) ) ;
#21745 = TOROIDAL_SURFACE ( 'NONE', #20322, 2.700000000000000622, 0.2000000000000000111 ) ;
#21746 = EDGE_CURVE ( 'NONE', #34600, #22843, #36861, .T. ) ;
#21747 = CARTESIAN_POINT ( 'NONE',  ( 18.00000000000000355, 17.08890430202814059, -43.76671000081927332 ) ) ;
#21748 = VECTOR ( 'NONE', #7085, 1000.000000000000000 ) ;
#21749 = DIRECTION ( 'NONE',  ( 0.000000000000000000, 0.9822872507286893873, -0.1873813145857213536 ) ) ;
#21750 = EDGE_LOOP ( 'NONE', ( #31202, #25520, #42629, #18315 ) ) ;
#21751 = ORIENTED_EDGE ( 'NONE', *, *, #37208, .F. ) ;
#21752 = DIRECTION ( 'NONE',  ( 0.000000000000000000, 0.000000000000000000, 1.000000000000000000 ) ) ;
#21753 = DIRECTION ( 'NONE',  ( 1.000000000000000000, 0.000000000000000000, 0.000000000000000000 ) ) ;
#21754 = AXIS2_PLACEMENT_3D ( 'NONE', #10770, #27151, #46 ) ;
#21755 = ORIENTED_EDGE ( 'NONE', *, *, #23392, .F. ) ;
#21757 = VERTEX_POINT ( 'NONE', #408 ) ;
#21756 = DIRECTION ( 'NONE',  ( -1.000000000000000000, 0.000000000000000000, 0.000000000000000000 ) ) ;
#21758 = CARTESIAN_POINT ( 'NONE',  ( 47.09643503919448193, 31.00000000000000355, 3.164684800459845349 ) ) ;
#21759 = ORIENTED_EDGE ( 'NONE', *, *, #1645, .F. ) ;
#21760 = CARTESIAN_POINT ( 'NONE',  ( 9.000000000000001776, -47.32430374665947426, 21.55018039121509688 ) ) ;
#21761 = EDGE_CURVE ( 'NONE', #4058, #501, #19888, .T. ) ;
#21762 = CARTESIAN_POINT ( 'NONE',  ( 17.99999999999999645, 0.000000000000000000, 0.000000000000000000 ) ) ;
#21763 = UNCERTAINTY_MEASURE_WITH_UNIT (LENGTH_MEASURE( 1.000000000000000082E-05 ), #33766, 'distance_accuracy_value', 'NONE');
#21764 = EDGE_LOOP ( 'NONE', ( #6633, #17973, #20103, #20153 ) ) ;
#21765 = CYLINDRICAL_SURFACE ( 'NONE', #17237, 116.0000000000000000 ) ;
#21766 = CARTESIAN_POINT ( 'NONE',  ( 52.50410707185378811, 39.99999999999999289, -40.15145572477544533 ) ) ;
#21767 = DIRECTION ( 'NONE',  ( -1.000000000000000000, 0.000000000000000000, 0.000000000000000000 ) ) ;
#21768 = DIRECTION ( 'NONE',  ( 0.000000000000000000, 0.000000000000000000, -1.000000000000000000 ) ) ;
#21769 = EDGE_CURVE ( 'NONE', #33264, #37125, #29541, .T. ) ;
#21770 = ORIENTED_EDGE ( 'NONE', *, *, #31173, .F. ) ;
#21771 = CARTESIAN_POINT ( 'NONE',  ( 17.99999999999999645, 0.000000000000000000, 0.000000000000000000 ) ) ;
#21772 = ORIENTED_EDGE ( 'NONE', *, *, #18329, .F. ) ;
#21773 = ADVANCED_FACE ( 'NONE', ( #17484 ), #27278, .T. ) ;
#21774 = VECTOR ( 'NONE', #1362, 1000.000000000000000 ) ;
#21775 = DIRECTION ( 'NONE',  ( 0.000000000000000000, -0.8183027759081743513, 0.5747874102143993857 ) ) ;
#21776 = CYLINDRICAL_SURFACE ( 'NONE', #31780, 59.00000000000001421 ) ;
#21777 = CIRCLE ( 'NONE', #2870, 59.00000000000000711 ) ;
#21778 = EDGE_CURVE ( 'NONE', #16960, #36435, #10250, .T. ) ;
#21779 = CARTESIAN_POINT ( 'NONE',  ( -69.75709431192164800, 31.00000000000000711, -9.183449035091399537 ) ) ;
#21780 = CARTESIAN_POINT ( 'NONE',  ( 0.000000000000000000, 3.996885678774600326, -120.4346956066681713 ) ) ;
#21781 = ORIENTED_EDGE ( 'NONE', *, *, #7062, .F. ) ;
#21782 = AXIS2_PLACEMENT_3D ( 'NONE', #23175, #33388, #29699 ) ;
#21783 = ADVANCED_FACE ( 'NONE', ( #33379, #20327 ), #3464, .F. ) ;
#21784 = PRESENTATION_STYLE_ASSIGNMENT (( #31346 ) ) ;
#21785 = CIRCLE ( 'NONE', #8491, 59.00000000000000711 ) ;
#21786 = ORIENTED_EDGE ( 'NONE', *, *, #25577, .F. ) ;
#21787 = CARTESIAN_POINT ( 'NONE',  ( 18.00000000000000355, 39.55064067543099071, -25.36340625197318488 ) ) ;
#21788 = CARTESIAN_POINT ( 'NONE',  ( 18.00000000000000355, -44.61570720899084819, -14.73072383765613047 ) ) ;
#21789 = CARTESIAN_POINT ( 'NONE',  ( -26.95034633362163845, 31.00000000000000355, -79.72278128421110921 ) ) ;
#21790 = CARTESIAN_POINT ( 'NONE',  ( -41.82916961767931951, 40.00000000000000000, -72.66191475361131324 ) ) ;
#21791 = CARTESIAN_POINT ( 'NONE',  ( 0.000000000000000000, -62.45178862086154226, -93.20969140437570388 ) ) ;
#21792 = ORIENTED_EDGE ( 'NONE', *, *, #17307, .F. ) ;
#21793 = DIRECTION ( 'NONE',  ( 1.000000000000000000, 0.000000000000000000, 0.000000000000000000 ) ) ;
#21794 = EDGE_LOOP ( 'NONE', ( #8288, #9208, #3931, #26530 ) ) ;
#21795 = DIRECTION ( 'NONE',  ( -1.000000000000000000, 0.000000000000000000, 0.000000000000000000 ) ) ;
#21796 = EDGE_CURVE ( 'NONE', #755, #37085, #38549, .T. ) ;
#21797 = EDGE_CURVE ( 'NONE', #3449, #3154, #3893, .T. ) ;
#21799 = ORIENTED_EDGE ( 'NONE', *, *, #29641, .F. ) ;
#21798 = CARTESIAN_POINT ( 'NONE',  ( 9.000000000000001776, -19.12429268481633571, -114.4126803693781085 ) ) ;
#21800 = CARTESIAN_POINT ( 'NONE',  ( 0.000000000000000000, 78.75547124681492051, -91.20343606296921735 ) ) ;
#21801 = ORIENTED_EDGE ( 'NONE', *, *, #5161, .F. ) ;
#21802 = DIRECTION ( 'NONE',  ( 0.000000000000000000, 0.8747630845319623871, -0.4845508703326482647 ) ) ;
#21803 = AXIS2_PLACEMENT_3D ( 'NONE', #39232, #35968, #19446 ) ;
#21804 = CARTESIAN_POINT ( 'NONE',  ( -147.8499999999987438, -3.037267345283352157E-13, 7.000000000000041744 ) ) ;
#21805 = AXIS2_PLACEMENT_3D ( 'NONE', #3274, #36661, #7203 ) ;
#21806 = VERTEX_POINT ( 'NONE', #3668 ) ;
#21807 = FACE_OUTER_BOUND ( 'NONE', #24906, .T. ) ;
#21808 = DIRECTION ( 'NONE',  ( 0.000000000000000000, 1.000000000000000000, 0.000000000000000000 ) ) ;
#21809 = VECTOR ( 'NONE', #21857, 1000.000000000000000 ) ;
#21810 = EDGE_CURVE ( 'NONE', #11023, #30476, #14193, .T. ) ;
#21812 = DIRECTION ( 'NONE',  ( 1.000000000000000000, 0.000000000000000000, 0.000000000000000000 ) ) ;
#21811 = DIRECTION ( 'NONE',  ( 0.000000000000000000, 0.000000000000000000, 1.000000000000000000 ) ) ;
#21813 = EDGE_LOOP ( 'NONE', ( #16938, #623, #3287, #35467 ) ) ;
#21814 = DIRECTION ( 'NONE',  ( 0.000000000000000000, 0.000000000000000000, 1.000000000000000000 ) ) ;
#21815 = ORIENTED_EDGE ( 'NONE', *, *, #15639, .T. ) ;
#21816 = CARTESIAN_POINT ( 'NONE',  ( 42.80287614962790599, -12.05525454449571932, 69.29271901957253021 ) ) ;
#21818 = CARTESIAN_POINT ( 'NONE',  ( -32.09999204393464822, 40.00000000000000000, -2.147948991655045159 ) ) ;
#21817 = AXIS2_PLACEMENT_3D ( 'NONE', #12078, #15364, #28234 ) ;
#21819 = CARTESIAN_POINT ( 'NONE',  ( 103.7695705685741387, 106.4195705685767166, 10.00000000000000000 ) ) ;
#21820 = DIRECTION ( 'NONE',  ( 0.000000000000000000, -0.5076658003388292428, -0.8615540813938125098 ) ) ;
#21821 = CARTESIAN_POINT ( 'NONE',  ( 17.99999999999999645, -23.21237537461669120, -109.7700237000594541 ) ) ;
#21822 = ORIENTED_EDGE ( 'NONE', *, *, #29509, .T. ) ;
#21823 = CARTESIAN_POINT ( 'NONE',  ( -22.00000000000000000, 31.00000000000000355, 0.000000000000000000 ) ) ;
#21824 = EDGE_LOOP ( 'NONE', ( #13314, #29901, #34539, #30795, #18391 ) ) ;
#21825 = EDGE_CURVE ( 'NONE', #214, #29479, #30903, .T. ) ;
#21826 = CARTESIAN_POINT ( 'NONE',  ( 0.000000000000000000, -12.43843445475394027, 111.5058645182329116 ) ) ;
#21827 = DIRECTION ( 'NONE',  ( -1.000000000000000000, 0.000000000000000000, 0.000000000000000000 ) ) ;
#21828 = CARTESIAN_POINT ( 'NONE',  ( -30.97228021248666607, 31.00000000000000355, 23.76985434021725041 ) ) ;
#21829 = ORIENTED_EDGE ( 'NONE', *, *, #23157, .T. ) ;
#21830 = CARTESIAN_POINT ( 'NONE',  ( 0.000000000000000000, 0.000000000000000000, 0.000000000000000000 ) ) ;
#21831 = CONTEXT_DEPENDENT_SHAPE_REPRESENTATION ( #11718, #19064 ) ;
#21832 = CARTESIAN_POINT ( 'NONE',  ( 9.000000000000001776, 114.1157422997285806, -20.82300072952825332 ) ) ;
#21833 = AXIS2_PLACEMENT_3D ( 'NONE', #29617, #12611, #38980 ) ;
#21834 = CARTESIAN_POINT ( 'NONE',  ( 57.37208743749949491, 31.00000000000000355, 50.31438278193533620 ) ) ;
#21835 = EDGE_CURVE ( 'NONE', #21873, #5856, #12115, .T. ) ;
#21836 = ORIENTED_EDGE ( 'NONE', *, *, #11922, .T. ) ;
#21837 = CARTESIAN_POINT ( 'NONE',  ( -44.44570800417318424, 31.00000000000000355, 25.56477902013656589 ) ) ;
#21838 = AXIS2_PLACEMENT_3D ( 'NONE', #27449, #30519, #23982 ) ;
#21839 = CARTESIAN_POINT ( 'NONE',  ( 5.726861599741335240, 40.00000000000000000, 87.39583333411552246 ) ) ;
#21840 = VERTEX_POINT ( 'NONE', #10685 ) ;
#21841 = VECTOR ( 'NONE', #8516, 1000.000000000000000 ) ;
#21842 = CARTESIAN_POINT ( 'NONE',  ( 17.99999999999999645, 0.000000000000000000, 0.000000000000000000 ) ) ;
#21843 = EDGE_CURVE ( 'NONE', #29479, #27194, #24022, .T. ) ;
#21844 = CYLINDRICAL_SURFACE ( 'NONE', #7524, 20.00000000000000355 ) ;
#21845 = FACE_OUTER_BOUND ( 'NONE', #6883, .T. ) ;
#21846 = ADVANCED_FACE ( 'NONE', ( #10468 ), #23808, .T. ) ;
#21847 = EDGE_CURVE ( 'NONE', #14319, #32706, #10918, .T. ) ;
#21848 = EDGE_CURVE ( 'NONE', #29862, #26320, #37894, .T. ) ;
#21850 = ORIENTED_EDGE ( 'NONE', *, *, #12645, .T. ) ;
#21849 = DIRECTION ( 'NONE',  ( 1.000000000000000000, -0.000000000000000000, 0.000000000000000000 ) ) ;
#21851 = CARTESIAN_POINT ( 'NONE',  ( 0.000000000000000000, -84.62908780824814414, -85.78116633471378805 ) ) ;
#21852 = DIRECTION ( 'NONE',  ( 1.000000000000000000, 0.000000000000000000, 0.000000000000000000 ) ) ;
#21853 = ORIENTED_EDGE ( 'NONE', *, *, #13459, .T. ) ;
#21854 = CARTESIAN_POINT ( 'NONE',  ( -34.23962737045593485, 40.00000000000000000, 59.30561363632230609 ) ) ;
#21855 = CARTESIAN_POINT ( 'NONE',  ( -150.5000000000000284, -5.254679414958916394E-13, 9.999999999999998224 ) ) ;
#21856 = ORIENTED_EDGE ( 'NONE', *, *, #40467, .F. ) ;
#21857 = DIRECTION ( 'NONE',  ( -1.000000000000000000, -0.000000000000000000, 0.000000000000000000 ) ) ;
#21858 = FACE_OUTER_BOUND ( 'NONE', #2191, .T. ) ;
#21859 = DIRECTION ( 'NONE',  ( 0.000000000000000000, 1.000000000000000000, 0.000000000000000000 ) ) ;
#21860 = ORIENTED_EDGE ( 'NONE', *, *, #4345, .F. ) ;
#21861 = VECTOR ( 'NONE', #27412, 1000.000000000000000 ) ;
#21862 = ORIENTED_EDGE ( 'NONE', *, *, #18466, .T. ) ;
#21863 = CARTESIAN_POINT ( 'NONE',  ( 0.000000000000000000, 0.000000000000000000, 0.000000000000000000 ) ) ;
#21864 = ORIENTED_EDGE ( 'NONE', *, *, #28509, .T. ) ;
#21865 = CARTESIAN_POINT ( 'NONE',  ( 17.99999999999999645, 52.19040376560434424, 99.31985817764196156 ) ) ;
#21866 = DIRECTION ( 'NONE',  ( -1.000000000000000000, 0.000000000000000000, 0.000000000000000000 ) ) ;
#21867 = FACE_OUTER_BOUND ( 'NONE', #10046, .T. ) ;
#21868 = CARTESIAN_POINT ( 'NONE',  ( 17.99999999999999645, -92.10690493017105496, 64.06707842432145128 ) ) ;
#21869 = ORIENTED_EDGE ( 'NONE', *, *, #42066, .F. ) ;
#21870 = DIRECTION ( 'NONE',  ( 1.000000000000000000, -3.469446951953615421E-17, 0.000000000000000000 ) ) ;
#21871 = AXIS2_PLACEMENT_3D ( 'NONE', #15051, #34652, #41180 ) ;
#21872 = CARTESIAN_POINT ( 'NONE',  ( 17.99999999999999645, 107.5680526044919674, -31.89649718262133149 ) ) ;
#21873 = VERTEX_POINT ( 'NONE', #27943 ) ;
#21874 = DIRECTION ( 'NONE',  ( 0.000000000000000000, -0.4817536741017036661, -0.8763066800438700232 ) ) ;
#21875 = DIRECTION ( 'NONE',  ( 0.000000000000000000, 0.000000000000000000, 1.000000000000000000 ) ) ;
#21876 = CARTESIAN_POINT ( 'NONE',  ( 17.99999999999999645, -34.74871106919551522, -106.6808302961375148 ) ) ;
#21877 = CARTESIAN_POINT ( 'NONE',  ( -6.851565232941113415, 31.00000000000000355, -51.95325991929587417 ) ) ;
#21878 = ORIENTED_EDGE ( 'NONE', *, *, #5591, .T. ) ;
#21880 = LINE ( 'NONE', #1971, #13623 ) ;
#21879 = DIRECTION ( 'NONE',  ( 0.000000000000000000, 0.000000000000000000, 1.000000000000000000 ) ) ;
#21881 = VERTEX_POINT ( 'NONE', #21851 ) ;
#21882 = AXIS2_PLACEMENT_3D ( 'NONE', #449, #23046, #21229 ) ;
#21883 = CARTESIAN_POINT ( 'NONE',  ( -8.160545988181935328, 40.00000000000000000, -61.88879904071598048 ) ) ;
#21884 = VECTOR ( 'NONE', #18197, 1000.000000000000000 ) ;
#21885 = FACE_OUTER_BOUND ( 'NONE', #34071, .T. ) ;
#21886 = DIRECTION ( 'NONE',  ( 1.000000000000000000, 0.000000000000000000, 0.000000000000000000 ) ) ;
#21887 = EDGE_CURVE ( 'NONE', #36681, #30521, #34237, .T. ) ;
#21888 = EDGE_CURVE ( 'NONE', #21478, #2989, #244, .T. ) ;
#21889 = DIRECTION ( 'NONE',  ( 0.000000000000000000, 0.000000000000000000, 1.000000000000000000 ) ) ;
#21890 = CARTESIAN_POINT ( 'NONE',  ( -19.99999999999999645, 31.00000000000000355, 0.000000000000000000 ) ) ;
#21891 = EDGE_CURVE ( 'NONE', #25432, #14258, #35128, .T. ) ;
#21892 = ORIENTED_EDGE ( 'NONE', *, *, #23805, .F. ) ;
#21893 = CARTESIAN_POINT ( 'NONE',  ( 22.24487986055951083, 40.00000000000000000, 28.98451114863597766 ) ) ;
#21894 = ORIENTED_EDGE ( 'NONE', *, *, #29295, .F. ) ;
#21895 = DIRECTION ( 'NONE',  ( 0.000000000000000000, 0.000000000000000000, 1.000000000000000000 ) ) ;
#21896 = AXIS2_PLACEMENT_3D ( 'NONE', #31828, #36142, #19402 ) ;
#21897 = DIRECTION ( 'NONE',  ( 0.000000000000000000, 0.000000000000000000, 1.000000000000000000 ) ) ;
#21898 = ORIENTED_EDGE ( 'NONE', *, *, #38877, .F. ) ;
#21899 = DIRECTION ( 'NONE',  ( -1.000000000000000000, -0.000000000000000000, 0.000000000000000000 ) ) ;
#21900 = DIRECTION ( 'NONE',  ( 1.000000000000000000, -3.035766082959412415E-17, 0.000000000000000000 ) ) ;
#21901 = VERTEX_POINT ( 'NONE', #21638 ) ;
#21902 = DIRECTION ( 'NONE',  ( 1.000000000000000000, 0.000000000000000000, 0.000000000000000000 ) ) ;
#21903 = VERTEX_POINT ( 'NONE', #41198 ) ;
#21904 = AXIS2_PLACEMENT_3D ( 'NONE', #40609, #30, #691 ) ;
#21905 = EDGE_LOOP ( 'NONE', ( #38949, #16854, #32207, #36469 ) ) ;
#21906 = PLANE ( 'NONE',  #20961 ) ;
#21907 = EDGE_CURVE ( 'NONE', #19127, #12837, #10021, .T. ) ;
#21908 = CARTESIAN_POINT ( 'NONE',  ( -10.54315780145427617, 31.00000000000000355, 79.17709703063970039 ) ) ;
#21909 = AXIS2_PLACEMENT_3D ( 'NONE', #15790, #5930, #32342 ) ;
#21910 = ORIENTED_EDGE ( 'NONE', *, *, #11676, .T. ) ;
#21911 = CARTESIAN_POINT ( 'NONE',  ( 0.000000000000000000, 20.99948489194481738, -42.60488980472760545 ) ) ;
#21912 = VECTOR ( 'NONE', #43169, 1000.000000000000000 ) ;
#21913 = FACE_OUTER_BOUND ( 'NONE', #22545, .T. ) ;
#21914 = EDGE_LOOP ( 'NONE', ( #43158, #29064, #2960, #26520 ) ) ;
#21915 = DIRECTION ( 'NONE',  ( 1.224646799147353207E-16, 1.000000000000000000, 0.000000000000000000 ) ) ;
#21916 = CARTESIAN_POINT ( 'NONE',  ( 0.000000000000000000, 49.25004636492389665, 16.68630974939776834 ) ) ;
#21917 = CARTESIAN_POINT ( 'NONE',  ( -7.718844055051848230, 31.00000000000000355, -22.75659427661714673 ) ) ;
#21919 = DIRECTION ( 'NONE',  ( 3.996523416598930318E-16, -2.658563593772947863E-15, -1.000000000000000000 ) ) ;
#21918 = DIRECTION ( 'NONE',  ( 0.000000000000000000, 0.000000000000000000, 1.000000000000000000 ) ) ;
#21920 = DIRECTION ( 'NONE',  ( -1.000000000000000000, -0.000000000000000000, -0.000000000000000000 ) ) ;
#21921 = LINE ( 'NONE', #42359, #3987 ) ;
#21922 =( GEOMETRIC_REPRESENTATION_CONTEXT ( 3 ) GLOBAL_UNCERTAINTY_ASSIGNED_CONTEXT ( ( #32918 ) ) GLOBAL_UNIT_ASSIGNED_CONTEXT ( ( #29043, #11377, #32286 ) ) REPRESENTATION_CONTEXT ( 'NONE', 'WORKASPACE' ) );
#21923 = ORIENTED_EDGE ( 'NONE', *, *, #12464, .F. ) ;
#21924 = ADVANCED_BREP_SHAPE_REPRESENTATION ( '', ( #28802, #13552 ), #9968 ) ;
#21925 = CARTESIAN_POINT ( 'NONE',  ( 17.99999999999999645, 0.000000000000000000, 0.000000000000000000 ) ) ;
#21926 = CIRCLE ( 'NONE', #27466, 10.99999999999999645 ) ;
#21927 = ORIENTED_EDGE ( 'NONE', *, *, #5658, .T. ) ;
#21928 = DIRECTION ( 'NONE',  ( 0.000000000000000000, 0.000000000000000000, 1.000000000000000000 ) ) ;
#21929 = CARTESIAN_POINT ( 'NONE',  ( 94.59594211465898184, 31.00000000000000000, 12.45590092308117569 ) ) ;
#21930 = DIRECTION ( 'NONE',  ( -1.000000000000000000, 0.000000000000000000, 0.000000000000000000 ) ) ;
#21931 = VERTEX_POINT ( 'NONE', #34675 ) ;
#21932 = CIRCLE ( 'NONE', #30273, 31.49899999999999878 ) ;
#21933 = CARTESIAN_POINT ( 'NONE',  ( 36.56095242094649933, 40.00000000000000000, -4.755136101395176951 ) ) ;
#21934 = ORIENTED_EDGE ( 'NONE', *, *, #11645, .T. ) ;
#21935 = VERTEX_POINT ( 'NONE', #1060 ) ;
#21936 = CARTESIAN_POINT ( 'NONE',  ( 18.00000000000000355, 0.000000000000000000, 0.000000000000000000 ) ) ;
#21937 = CARTESIAN_POINT ( 'NONE',  ( 0.000000000000000000, 88.00363688980546328, 82.31555682352686176 ) ) ;
#21938 = DIRECTION ( 'NONE',  ( -1.000000000000000000, 0.000000000000000000, 0.000000000000000000 ) ) ;
#21939 = AXIS2_PLACEMENT_3D ( 'NONE', #38143, #11992, #5193 ) ;
#21940 = EDGE_CURVE ( 'NONE', #39201, #25078, #16339, .T. ) ;
#21941 = FACE_BOUND ( 'NONE', #33829, .T. ) ;
#21942 = DIRECTION ( 'NONE',  ( 0.000000000000000000, 0.000000000000000000, 1.000000000000000000 ) ) ;
#21943 = CIRCLE ( 'NONE', #7976, 20.00000000000000355 ) ;
#21944 = ORIENTED_EDGE ( 'NONE', *, *, #13896, .T. ) ;
#21945 = CARTESIAN_POINT ( 'NONE',  ( 0.000000000000000000, 0.000000000000000000, 0.000000000000000000 ) ) ;
#21946 = ORIENTED_EDGE ( 'NONE', *, *, #23556, .F. ) ;
#21947 = CARTESIAN_POINT ( 'NONE',  ( -10.00000000000000000, 0.000000000000000000, 0.000000000000000000 ) ) ;
#21948 = CYLINDRICAL_SURFACE ( 'NONE', #17267, 59.00000000000000000 ) ;
#21949 = EDGE_CURVE ( 'NONE', #38496, #3479, #11565, .T. ) ;
#21950 = DIRECTION ( 'NONE',  ( 1.000000000000000000, 0.000000000000000000, 0.000000000000000000 ) ) ;
#21951 = FACE_OUTER_BOUND ( 'NONE', #7255, .T. ) ;
#21952 = VERTEX_POINT ( 'NONE', #31416 ) ;
#21953 = VERTEX_POINT ( 'NONE', #25123 ) ;
#21954 = FACE_OUTER_BOUND ( 'NONE', #7688, .T. ) ;
#21955 = ADVANCED_FACE ( 'NONE', ( #15297 ), #38160, .T. ) ;
#21956 = AXIS2_PLACEMENT_3D ( 'NONE', #34484, #21671, #5037 ) ;
#21957 = ORIENTED_EDGE ( 'NONE', *, *, #19004, .T. ) ;
#21959 = VERTEX_POINT ( 'NONE', #8052 ) ;
#21958 = DIRECTION ( 'NONE',  ( -1.000000000000000000, -0.000000000000000000, -0.000000000000000000 ) ) ;
#21960 = EDGE_CURVE ( 'NONE', #35045, #33779, #34447, .T. ) ;
#21961 = CARTESIAN_POINT ( 'NONE',  ( 48.78760054486801323, 31.00000000000000355, -28.06521077754944926 ) ) ;
#21962 = ORIENTED_EDGE ( 'NONE', *, *, #41200, .F. ) ;
#21963 = CARTESIAN_POINT ( 'NONE',  ( 17.99999999999999645, 116.0452958106480708, 32.46506308663498430 ) ) ;
#21964 = AXIS2_PLACEMENT_3D ( 'NONE', #33768, #10651, #4515 ) ;
#21965 = DIRECTION ( 'NONE',  ( 0.000000000000000000, 0.000000000000000000, 1.000000000000000000 ) ) ;
#21966 = ORIENTED_EDGE ( 'NONE', *, *, #4610, .F. ) ;
#21967 = CARTESIAN_POINT ( 'NONE',  ( -61.81085491475939619, 40.00000000000000711, 35.57109242552864004 ) ) ;
#21968 = AXIS2_PLACEMENT_3D ( 'NONE', #1055, #37509, #36463 ) ;
#21969 = LINE ( 'NONE', #4464, #7445 ) ;
#21970 =( GEOMETRIC_REPRESENTATION_CONTEXT ( 3 ) GLOBAL_UNCERTAINTY_ASSIGNED_CONTEXT ( ( #4249 ) ) GLOBAL_UNIT_ASSIGNED_CONTEXT ( ( #41344, #37649, #24398 ) ) REPRESENTATION_CONTEXT ( 'NONE', 'WORKASPACE' ) );
#21971 = FACE_OUTER_BOUND ( 'NONE', #14669, .T. ) ;
#21972 = ORIENTED_EDGE ( 'NONE', *, *, #37441, .F. ) ;
#21973 = CARTESIAN_POINT ( 'NONE',  ( 0.000000000000000000, 37.07968990261480968, 109.9140418541958724 ) ) ;
#21974 = VERTEX_POINT ( 'NONE', #35097 ) ;
#21975 = AXIS2_PLACEMENT_3D ( 'NONE', #21591, #18524, #40942 ) ;
#21976 = ADVANCED_FACE ( 'NONE', ( #12006 ), #28378, .F. ) ;
#21977 = CARTESIAN_POINT ( 'NONE',  ( 1.039096088315723056E-14, -6.912265343809663812E-14, -26.00000000000000355 ) ) ;
#21978 = DIRECTION ( 'NONE',  ( -1.000000000000000000, 0.000000000000000000, 0.000000000000000000 ) ) ;
#21979 = CARTESIAN_POINT ( 'NONE',  ( 64.89583333437747115, 31.00000000000000000, -4.254240043327834009 ) ) ;
#21980 = CARTESIAN_POINT ( 'NONE',  ( 0.000000000000000000, -106.5605152861907072, 56.26142179985788516 ) ) ;
#21981 = VERTEX_POINT ( 'NONE', #7621 ) ;
#21982 = VECTOR ( 'NONE', #38027, 1000.000000000000000 ) ;
#21983 = DIRECTION ( 'NONE',  ( -1.000000000000000000, -0.000000000000000000, -0.000000000000000000 ) ) ;
#21984 = ORIENTED_EDGE ( 'NONE', *, *, #32220, .F. ) ;
#21985 = FACE_OUTER_BOUND ( 'NONE', #22609, .T. ) ;
#21986 = DIRECTION ( 'NONE',  ( -1.000000000000000000, 0.000000000000000000, 0.000000000000000000 ) ) ;
#21987 = CARTESIAN_POINT ( 'NONE',  ( 39.23423008409712054, 31.00000000000000355, 79.83814995801117220 ) ) ;
#21988 = CARTESIAN_POINT ( 'NONE',  ( -29.11455967534193334, 40.00000000000000000, 85.38284731560057139 ) ) ;
#21989 = DIRECTION ( 'NONE',  ( 0.000000000000000000, 0.000000000000000000, 1.000000000000000000 ) ) ;
#21990 = AXIS2_PLACEMENT_3D ( 'NONE', #8770, #5285, #35785 ) ;
#21991 = EDGE_CURVE ( 'NONE', #17128, #20200, #33723, .T. ) ;
#21992 = VECTOR ( 'NONE', #14606, 1000.000000000000000 ) ;
#21993 = ORIENTED_EDGE ( 'NONE', *, *, #17846, .F. ) ;
#21994 = CARTESIAN_POINT ( 'NONE',  ( 18.00000000000000355, 46.77034588191303044, 22.72740077717245910 ) ) ;
#21995 = ORIENTED_EDGE ( 'NONE', *, *, #7647, .T. ) ;
#21996 =( NAMED_UNIT ( * ) SI_UNIT ( $, .STERADIAN. ) SOLID_ANGLE_UNIT ( ) );
#21997 = AXIS2_PLACEMENT_3D ( 'NONE', #37667, #21144, #37024 ) ;
#21999 = AXIS2_PLACEMENT_3D ( 'NONE', #28127, #35499, #18552 ) ;
#21998 = DIRECTION ( 'NONE',  ( -3.996523416598930318E-16, 2.658563593772947863E-15, 1.000000000000000000 ) ) ;
#22001 = VERTEX_POINT ( 'NONE', #14412 ) ;
#22000 = CARTESIAN_POINT ( 'NONE',  ( 0.000000000000000000, -35.78484819117565507, -110.3423972910436390 ) ) ;
#22002 = DIRECTION ( 'NONE',  ( 0.000000000000000000, 0.000000000000000000, -1.000000000000000000 ) ) ;
#22003 = ORIENTED_EDGE ( 'NONE', *, *, #4702, .F. ) ;
#22004 = DIRECTION ( 'NONE',  ( 0.000000000000000000, 0.000000000000000000, 1.000000000000000000 ) ) ;
#22005 = DIRECTION ( 'NONE',  ( 1.000000000000000000, -0.000000000000000000, -0.000000000000000000 ) ) ;
#22006 = EDGE_CURVE ( 'NONE', #31505, #33113, #17931, .T. ) ;
#22007 = AXIS2_PLACEMENT_3D ( 'NONE', #13663, #20015, #13021 ) ;
#22008 = CARTESIAN_POINT ( 'NONE',  ( 18.00000000000000355, -34.03046037009278280, 33.13733193845793323 ) ) ;
#22009 = ORIENTED_EDGE ( 'NONE', *, *, #36048, .T. ) ;
#22010 = CARTESIAN_POINT ( 'NONE',  ( 15.59370980024835696, 31.00000000000000355, -20.29731371384564653 ) ) ;
#22011 = DIRECTION ( 'NONE',  ( -1.000000000000000000, 0.000000000000000000, 0.000000000000000000 ) ) ;
#22012 = ADVANCED_FACE ( 'NONE', ( #18149 ), #4333, .T. ) ;
#22014 = DIRECTION ( 'NONE',  ( 0.000000000000000000, -0.7865515558026479059, 0.6175246149461850464 ) ) ;
#22013 = CARTESIAN_POINT ( 'NONE',  ( 17.99999999999999645, -31.80866420683992857, 2.997093558041182160 ) ) ;
#22015 = ORIENTED_EDGE ( 'NONE', *, *, #4057, .F. ) ;
#22016 = DIRECTION ( 'NONE',  ( 0.000000000000000000, 0.000000000000000000, 1.000000000000000000 ) ) ;
#22017 = EDGE_LOOP ( 'NONE', ( #946, #35824, #34469, #21316 ) ) ;
#22018 = DIRECTION ( 'NONE',  ( -1.000000000000000000, -0.000000000000000000, -0.000000000000000000 ) ) ;
#22019 = CARTESIAN_POINT ( 'NONE',  ( 36.58905133581346547, 40.00000000000000000, -27.97030060560320308 ) ) ;
#22020 = CYLINDRICAL_SURFACE ( 'NONE', #35564, 120.5010000000000190 ) ;
#22021 = AXIS2_PLACEMENT_3D ( 'NONE', #30251, #10829, #33946 ) ;
#22022 = CYLINDRICAL_SURFACE ( 'NONE', #3309, 120.5010000000000190 ) ;
#22023 = DIRECTION ( 'NONE',  ( -1.000000000000000000, 0.000000000000000000, 0.000000000000000000 ) ) ;
#22024 = B_SPLINE_CURVE_WITH_KNOTS ( 'NONE', 3,
 ( #3645, #23342, #40519, #14164, #33995, #4084, #13516, #40079, #23775, #3214, #10653, #23990, #17455, #16592, #16805, #13306, #30299, #26808, #36603, #27457, #10217, #37045, #40728, #10882, #39868, #13737, #23563, #36831, #6725, #20089, #17014, #6936, #33353, #27039, #30095, #17242, #20508, #20294, #33558, #40308, #33770, #3856, #30525, #41613, #28343, #31167, #4753, #31588, #8456, #24644, #11971, #28116, #37899, #30940, #1463, #1023, #14374, #1682, #27690, #11314, #8020, #17891, #40954, #15033, #38126, #21818, #34414, #11105, #8249, #1257, #11763, #28560, #24430, #37686, #41163, #21388, #34638, #7807, #18120, #17672, #31813, #31380, #21606, #14817, #4969, #41823, #25093, #41381, #18327, #21164, #37478, #24873, #4518, #11530, #34856, #14604, #35062, #27908, #18539, #38333, #5175, #1900, #15267, #7593, #20949, #34204, #4299, #32024, #26124, #39389, #9301, #12397, #12599, #2102, #35279, #42664, #25720, #32862, #42879, #9528, #18970, #8664, #5813, #32227, #28762, #16096, #28970, #32437, #8891, #22657, #22241, #2941, #42026, #22884, #2302, #36127, #6247, #15466, #25296, #29607, #12811, #19590, #12180, #16303, #25498, #38540, #15670, #35692, #2524, #35489, #38759, #22446, #5607, #2733, #22019, #5401, #18765, #42241, #38971, #29189, #9090, #19169, #15888, #42459, #25917, #39179, #35901, #6035, #19387, #32655, #29395, #3157, #30246, #33505, #3383, #40257, #20674, #13253, #548, #39612, #10157, #19802, #13040, #17403, #13900, #37201, #23933, #23088, #13467, #23726, #27197, #33941, #33071, #9739, #7098, #20454, #20244, #16964, #16533, #6887, #40466, #43100, #23510, #30684, #36989, #314, #26544, #4030, #30044, #9944, #29836, #23293, #13679, #33714, #36545, #36774, #26342, #39816, #36335, #6668, #6453, #26756, #20033, #3591, #33301, #16753, #3801, #94, #40028, #26979, #10388, #7310, #17182, #30470, #10600, #4916, #11055, #21557, #757, #24154, #7542, #37633, #8403, #35016, #7753, #10826, #38284, #37421, #34365, #4694, #11263, #14765, #41110, #11480, #5124, #34805, #31107, #24816, #30889, #18486, #31329, #21115, #31540, #24592, #18276, #40673, #1629, #14981, #27854, #1197, #8196, #7967, #18069, #20899, #37844, #28292, #40900, #21332, #34150, #41328, #11707, #14320, #21766, #17833, #24380, #4251, #4461, #1414, #38071, #14550, #34582, #14115, #17621, #969, #27631, #27406, #28067, #41557, #25044, #31976, #39132, #25872, #38490, #5560, #2253, #8606, #12762, #25667, #31757, #19332, #35847, #41977, #9252, #1851, #11918, #21967, #32602, #25446, #39332, #22824, #38708, #35225, #18919, #25244, #26068, #22605, #32175, #5977, #9471, #15214, #5347, #35644, #18717, #38924, #2053, #28917, #16044, #8831, #2683, #12343, #29345, #15417, #36077, #42613, #6195, #28511, #41774, #42183, #9042, #12126, #28711, #22398, #22188, #35444, #15613, #5761, #19118, #32383, #2469, #15830, #29139, #42408, #12551, #3747, #13201, #44, #6840, #43050, #19979, #12984, #257, #9691, #36720, #39975, #9894, #3541, #27150, #19751, #7047, #2888, #16703, #26285, #19540, #23885, #20403, #491, #30418, #29553, #33248, #30197, #33663, #40414, #39560, #16256, #13629, #26924, #13857, #17129, #10550, #26492, #23244, #36936, #3333, #37150, #32809, #42823, #39766, #13413, #20196, #36493, #29990, #23035, #40203, #36285, #33453, #10104, #6614, #16916, #6404, #33018, #3102, #16476, #29777, #26706, #23460, #10339, #23678, #31492, #18223, #17357, #7697, #18015, #21502, #14927, #14064, #3978, #1364, #14711, #14496, #11214, #27358, #4410, #21067, #37374, #17782, #24989, #31281, #24544, #20854, #28232, #24333, #4197, #10769, #17568, #7917, #28017, #30842, #31054, #20619, #24103, #30638, #7258, #41060, #34315, #702, #27808, #40621, #7486, #41277, #34104, #37587, #1146, #916, #1578, #37798, #33891, #38013, #11426, #14268, #24760, #27575, #8140, #41497, #40849, #11002, #21278, #34527, #4638, #34756, #4862, #11647, #32547, #2409, #38651, #42352, #2633, #8350, #1796, #42128, #25190, #32124, #12710, #25612, #38438, #25394, #8774, #2005, #22551, #8557, #19274, #15775, #5918, #29082, #15996 ),
 .UNSPECIFIED., .F., .F.,
 ( 4, 2, 2, 2, 2, 2, 2, 2, 2, 2, 2, 2, 2, 2, 2, 2, 2, 2, 2, 2, 2, 2, 2, 2, 2, 2, 2, 2, 2, 2, 2, 2, 2, 2, 2, 2, 2, 2, 2, 2, 2, 2, 2, 2, 2, 2, 2, 2, 2, 2, 2, 2, 2, 2, 2, 2, 2, 2, 2, 2, 2, 2, 2, 2, 2, 2, 2, 2, 2, 2, 2, 2, 2, 2, 2, 2, 2, 2, 2, 2, 2, 2, 2, 2, 2, 2, 2, 2, 2, 2, 2, 2, 2, 2, 2, 2, 2, 2, 2, 2, 2, 2, 2, 2, 2, 2, 2, 2, 2, 2, 2, 2, 2, 2, 2, 2, 2, 2, 2, 2, 2, 2, 2, 2, 2, 2, 2, 2, 2, 2, 2, 2, 2, 2, 2, 2, 2, 2, 2, 2, 2, 2, 2, 2, 2, 2, 2, 2, 2, 2, 2, 2, 2, 2, 2, 2, 2, 2, 2, 2, 2, 2, 2, 2, 2, 2, 2, 2, 2, 2, 2, 2, 2, 2, 2, 2, 2, 2, 2, 2, 2, 2, 2, 2, 2, 2, 2, 2, 2, 2, 2, 2, 2, 2, 2, 2, 2, 2, 2, 2, 2, 2, 2, 2, 2, 2, 2, 2, 2, 2, 2, 2, 2, 2, 2, 2, 2, 2, 2, 2, 2, 2, 2, 2, 2, 2, 2, 2, 2, 2, 2, 2, 2, 2, 2, 2, 2, 2, 2, 2, 2, 2, 2, 2, 2, 2, 2, 2, 2, 2, 2, 2, 2, 2, 2, 2, 4 ),
 ( 0.000000000000000000, 0.003906250000000000000, 0.007812500000000000000, 0.01171875000000000000, 0.01562500000000000000, 0.01953125000000000000, 0.02343750000000000000, 0.02734375000000000000, 0.03125000000000000000, 0.03515625000000000000, 0.03906250000000000000, 0.04296875000000000000, 0.04687500000000000000, 0.05078125000000000000, 0.05468750000000000000, 0.05859375000000000000, 0.06250000000000000000, 0.06640625000000000000, 0.07031250000000000000, 0.07421875000000000000, 0.07812500000000000000, 0.08203125000000000000, 0.08593750000000000000, 0.08984375000000000000, 0.09375000000000000000, 0.09765625000000000000, 0.1015625000000000000, 0.1054687500000000000, 0.1093750000000000000, 0.1132812500000000000, 0.1171875000000000000, 0.1210937500000000000, 0.1250000000000000000, 0.1289062500000000000, 0.1328125000000000000, 0.1367187500000000000, 0.1406250000000000000, 0.1445312500000000000, 0.1484375000000000000, 0.1523437500000000000, 0.1562500000000000000, 0.1601562500000000000, 0.1640625000000000000, 0.1679687500000000000, 0.1718750000000000000, 0.1757812500000000000, 0.1796875000000000000, 0.1835937500000000000, 0.1875000000000000000, 0.1914062500000000000, 0.1953125000000000000, 0.1992187500000000000, 0.2031250000000000000, 0.2070312500000000000, 0.2109375000000000000, 0.2148437500000000000, 0.2187500000000000000, 0.2226562500000000000, 0.2265625000000000000, 0.2304687500000000000, 0.2343750000000000000, 0.2382812500000000000, 0.2421875000000000000, 0.2460937500000000000, 0.2500000000000000000, 0.2539062500000000000, 0.2578125000000000000, 0.2617187500000000000, 0.2656250000000000000, 0.2695312500000000000, 0.2734375000000000000, 0.2773437500000000000, 0.2812500000000000000, 0.2851562500000000000, 0.2890625000000000000, 0.2929687500000000000, 0.2968750000000000000, 0.3007812500000000000, 0.3046875000000000000, 0.3085937500000000000, 0.3125000000000000000, 0.3164062500000000000, 0.3203125000000000000, 0.3242187500000000000, 0.3281250000000000000, 0.3320312500000000000, 0.3359375000000000000, 0.3398437500000000000, 0.3437500000000000000, 0.3476562500000000000, 0.3515625000000000000, 0.3554687500000000000, 0.3593750000000000000, 0.3632812500000000000, 0.3671875000000000000, 0.3710937500000000000, 0.3750000000000000000, 0.3789062500000000000, 0.3828125000000000000, 0.3867187500000000000, 0.3906250000000000000, 0.3945312500000000000, 0.3984375000000000000, 0.4023437500000000000, 0.4062500000000000000, 0.4101562500000000000, 0.4140625000000000000, 0.4179687500000000000, 0.4218750000000000000, 0.4257812500000000000, 0.4296875000000000000, 0.4335937500000000000, 0.4375000000000000000, 0.4414062500000000000, 0.4453125000000000000, 0.4492187500000000000, 0.4531250000000000000, 0.4570312500000000000, 0.4609375000000000000, 0.4648437500000000000, 0.4687500000000000000, 0.4726562500000000000, 0.4765625000000000000, 0.4804687500000000000, 0.4843750000000000000, 0.4882812500000000000, 0.4921875000000000000, 0.4960937500000000000, 0.5000000000000000000, 0.5039062500000000000, 0.5078125000000000000, 0.5117187500000000000, 0.5156250000000000000, 0.5195312500000000000, 0.5234375000000000000, 0.5273437500000000000, 0.5312500000000000000, 0.5351562500000000000, 0.5390625000000000000, 0.5429687500000000000, 0.5468750000000000000, 0.5507812500000000000, 0.5546875000000000000, 0.5585937500000000000, 0.5625000000000000000, 0.5664062500000000000, 0.5703125000000000000, 0.5742187500000000000, 0.5781250000000000000, 0.5820312500000000000, 0.5859375000000000000, 0.5898437500000000000, 0.5937500000000000000, 0.5976562500000000000, 0.6015625000000000000, 0.6054687500000000000, 0.6093750000000000000, 0.6132812500000000000, 0.6171875000000000000, 0.6210937500000000000, 0.6250000000000000000, 0.6289062500000000000, 0.6328125000000000000, 0.6367187500000000000, 0.6406250000000000000, 0.6445312500000000000, 0.6484375000000000000, 0.6523437500000000000, 0.6562500000000000000, 0.6601562500000000000, 0.6640625000000000000, 0.6679687500000000000, 0.6718750000000000000, 0.6757812500000000000, 0.6796875000000000000, 0.6835937500000000000, 0.6875000000000000000, 0.6914062500000000000, 0.6953125000000000000, 0.6992187500000000000, 0.7031250000000000000, 0.7070312500000000000, 0.7109375000000000000, 0.7148437500000000000, 0.7187500000000000000, 0.7226562500000000000, 0.7265625000000000000, 0.7304687500000000000, 0.7343750000000000000, 0.7382812500000000000, 0.7421875000000000000, 0.7460937500000000000, 0.7500000000000000000, 0.7539062500000000000, 0.7578125000000000000, 0.7617187500000000000, 0.7656250000000000000, 0.7695312500000000000, 0.7734375000000000000, 0.7773437500000000000, 0.7812500000000000000, 0.7851562500000000000, 0.7890625000000000000, 0.7929687500000000000, 0.7968750000000000000, 0.8007812500000000000, 0.8046875000000000000, 0.8085937500000000000, 0.8125000000000000000, 0.8164062500000000000, 0.8203125000000000000, 0.8242187500000000000, 0.8281250000000000000, 0.8320312500000000000, 0.8359375000000000000, 0.8398437500000000000, 0.8437500000000000000, 0.8476562500000000000, 0.8515625000000000000, 0.8554687500000000000, 0.8593750000000000000, 0.8632812500000000000, 0.8671875000000000000, 0.8710937500000000000, 0.8750000000000000000, 0.8789062500000000000, 0.8828125000000000000, 0.8867187500000000000, 0.8906250000000000000, 0.8945312500000000000, 0.8984375000000000000, 0.9023437500000000000, 0.9062500000000000000, 0.9101562500000000000, 0.9140625000000000000, 0.9179687500000000000, 0.9218750000000000000, 0.9257812500000000000, 0.9296875000000000000, 0.9335937500000000000, 0.9375000000000000000, 0.9414062500000000000, 0.9453125000000000000, 0.9492187500000000000, 0.9531250000000000000, 0.9570312500000000000, 0.9609375000000000000, 0.9648437500000000000, 0.9687500000000000000, 0.9726562500000000000, 0.9765625000000000000, 0.9804687500000000000, 0.9843750000000000000, 0.9882812500000000000, 0.9921875000000000000, 0.9960937500000000000, 1.000000000000000000 ),
 .UNSPECIFIED. ) ;
#22026 = EDGE_LOOP ( 'NONE', ( #34943, #20240, #39084, #26183 ) ) ;
#22025 = AXIS2_PLACEMENT_3D ( 'NONE', #19486, #1792, #15149 ) ;
#22027 = CARTESIAN_POINT ( 'NONE',  ( 0.5469614295415388128, -4.303013824935362663, -3.535263753543555598 ) ) ;
#22028 = AXIS2_PLACEMENT_3D ( 'NONE', #26140, #15911, #5627 ) ;
#22029 = EDGE_LOOP ( 'NONE', ( #13708, #13917, #27030, #37733 ) ) ;
#22030 = EDGE_CURVE ( 'NONE', #20054, #14989, #18576, .T. ) ;
#22031 = AXIS2_PLACEMENT_3D ( 'NONE', #27365, #4649, #20412 ) ;
#22032 = DIRECTION ( 'NONE',  ( 0.000000000000000000, 0.000000000000000000, 1.000000000000000000 ) ) ;
#22033 = DIRECTION ( 'NONE',  ( 1.000000000000000000, -0.000000000000000000, -0.000000000000000000 ) ) ;
#22034 = CIRCLE ( 'NONE', #26885, 13.59999999999999964 ) ;
#22036 = EDGE_CURVE ( 'NONE', #27845, #28707, #37210, .T. ) ;
#22035 = CARTESIAN_POINT ( 'NONE',  ( 25.50046184691807483, 31.00000000000000355, -22.37655979312362931 ) ) ;
#22037 = VERTEX_POINT ( 'NONE', #5004 ) ;
#22038 = CYLINDRICAL_SURFACE ( 'NONE', #16990, 51.99999999999999289 ) ;
#22040 = ORIENTED_EDGE ( 'NONE', *, *, #2707, .T. ) ;
#22039 = CIRCLE ( 'NONE', #40747, 120.5010000000000190 ) ;
#22042 = AXIS2_PLACEMENT_3D ( 'NONE', #30873, #950, #27614 ) ;
#22041 = DIRECTION ( 'NONE',  ( 0.000000000000000000, 0.000000000000000000, 1.000000000000000000 ) ) ;
#22043 = CARTESIAN_POINT ( 'NONE',  ( 71.66629920589342362, 31.00000000000000000, 24.32769631419027689 ) ) ;
#22044 = ORIENTED_EDGE ( 'NONE', *, *, #42234, .F. ) ;
#22045 = CARTESIAN_POINT ( 'NONE',  ( -39.97893566998936166, 31.00000000000000355, -35.18630237794885574 ) ) ;
#22046 = CARTESIAN_POINT ( 'NONE',  ( -5.726861599740728614, 40.00000000000000000, 87.60416666588449175 ) ) ;
#22047 = EDGE_LOOP ( 'NONE', ( #35803, #35844 ) ) ;
#22048 = DIRECTION ( 'NONE',  ( 0.000000000000000000, 0.000000000000000000, 1.000000000000000000 ) ) ;
#22049 = CARTESIAN_POINT ( 'NONE',  ( 0.000000000000000000, 13.00789606333630566, -115.2683592318613819 ) ) ;
#22050 = CARTESIAN_POINT ( 'NONE',  ( 0.000000000000000000, -115.9750404417043939, -2.406240749598616446 ) ) ;
#22051 = AXIS2_PLACEMENT_3D ( 'NONE', #4414, #27153, #3751 ) ;
#22053 = ORIENTED_EDGE ( 'NONE', *, *, #1546, .T. ) ;
#22052 = CARTESIAN_POINT ( 'NONE',  ( 0.000000000000000000, 2.123073309835852296, -47.45152853935331905 ) ) ;
#22054 = DIRECTION ( 'NONE',  ( 0.000000000000000000, 0.000000000000000000, 1.000000000000000000 ) ) ;
#22055 = DIRECTION ( 'NONE',  ( -1.000000000000000000, 0.000000000000000000, 0.000000000000000000 ) ) ;
#22056 = CIRCLE ( 'NONE', #8772, 13.40000000000000213 ) ;
#22057 = ADVANCED_FACE ( 'NONE', ( #18359 ), #41647, .T. ) ;
#22058 = ORIENTED_EDGE ( 'NONE', *, *, #34704, .F. ) ;
#22059 = CARTESIAN_POINT ( 'NONE',  ( 31.73387399974884104, 40.00000000000000000, -54.96645564127986461 ) ) ;
#22060 = CARTESIAN_POINT ( 'NONE',  ( 0.000000000000000000, 0.000000000000000000, 0.000000000000000000 ) ) ;
#22061 = ORIENTED_EDGE ( 'NONE', *, *, #174, .F. ) ;
#22062 = ADVANCED_FACE ( 'NONE', ( #8697 ), #9334, .F. ) ;
#22063 = CYLINDRICAL_SURFACE ( 'NONE', #15525, 31.49899999999999878 ) ;
#22064 = CYLINDRICAL_SURFACE ( 'NONE', #30615, 59.00000000000000000 ) ;
#22065 = AXIS2_PLACEMENT_3D ( 'NONE', #19089, #28888, #3241 ) ;
#22066 = CARTESIAN_POINT ( 'NONE',  ( 17.99999999999999645, 110.8621702203453339, -34.14058016547420493 ) ) ;
#22067 = ORIENTED_EDGE ( 'NONE', *, *, #3209, .F. ) ;
#22068 = AXIS2_PLACEMENT_3D ( 'NONE', #10984, #14480, #27789 ) ;
#22069 = ORIENTED_EDGE ( 'NONE', *, *, #10588, .F. ) ;
#22070 = CYLINDRICAL_SURFACE ( 'NONE', #42750, 59.00000000000000000 ) ;
#22071 = VERTEX_POINT ( 'NONE', #19423 ) ;
#22072 = DIRECTION ( 'NONE',  ( 0.000000000000000000, 0.000000000000000000, 1.000000000000000000 ) ) ;
#22073 = DIRECTION ( 'NONE',  ( -3.009274222672345096E-17, -1.000000000000000000, 2.455023325076454960E-18 ) ) ;
#22074 = FACE_OUTER_BOUND ( 'NONE', #26489, .T. ) ;
#22075 = CARTESIAN_POINT ( 'NONE',  ( -5.991980000000000750, 0.000000000000000000, 19.11697999999999809 ) ) ;
#22076 = ORIENTED_EDGE ( 'NONE', *, *, #25580, .F. ) ;
#22077 = DIRECTION ( 'NONE',  ( 0.000000000000000000, 0.9822872507286893873, -0.1873813145857213536 ) ) ;
#22078 = PRODUCT_DEFINITION_CONTEXT ( 'detailed design', #14514, 'design' ) ;
#22079 = VERTEX_POINT ( 'NONE', #25751 ) ;
#22080 = CYLINDRICAL_SURFACE ( 'NONE', #28749, 13.59999999999999787 ) ;
#22081 = EDGE_CURVE ( 'NONE', #17523, #18784, #35722, .T. ) ;
#22082 = ADVANCED_FACE ( 'NONE', ( #8926 ), #42695, .F. ) ;
#22084 = ORIENTED_EDGE ( 'NONE', *, *, #32690, .F. ) ;
#22083 = CIRCLE ( 'NONE', #26938, 2.700000000000000622 ) ;
#22085 = DIRECTION ( 'NONE',  ( 1.000000000000000000, 0.000000000000000000, 0.000000000000000000 ) ) ;
#22086 = EDGE_CURVE ( 'NONE', #10513, #25132, #24711, .T. ) ;
#22087 = EDGE_CURVE ( 'NONE', #11411, #14100, #1676, .T. ) ;
#22088 = ADVANCED_FACE ( 'NONE', ( #42918 ), #32052, .F. ) ;
#22089 = VECTOR ( 'NONE', #14823, 1000.000000000000000 ) ;
#22090 = CARTESIAN_POINT ( 'NONE',  ( 17.99999999999999645, 0.000000000000000000, 0.000000000000000000 ) ) ;
#22091 = AXIS2_PLACEMENT_3D ( 'NONE', #16761, #30047, #19808 ) ;
#22092 = AXIS2_PLACEMENT_3D ( 'NONE', #6859, #3563, #19775 ) ;
#22093 = CARTESIAN_POINT ( 'NONE',  ( 106.4195705685741302, 1.999999999999996669, -106.4195705685767166 ) ) ;
#22094 = DIRECTION ( 'NONE',  ( 0.000000000000000000, 0.000000000000000000, 1.000000000000000000 ) ) ;
#22095 = CARTESIAN_POINT ( 'NONE',  ( -49.89583333467011528, 31.00000000000000355, 3.272492339034415831 ) ) ;
#22096 = EDGE_LOOP ( 'NONE', ( #29208, #11694, #36994, #9010 ) ) ;
#22097 = AXIS2_PLACEMENT_3D ( 'NONE', #2653, #16015, #29312 ) ;
#22098 = DIRECTION ( 'NONE',  ( -1.000000000000000000, 0.000000000000000000, 0.000000000000000000 ) ) ;
#22099 = CIRCLE ( 'NONE', #39437, 2.100000000000000089 ) ;
#22100 = ORIENTED_EDGE ( 'NONE', *, *, #2209, .T. ) ;
#22101 = CARTESIAN_POINT ( 'NONE',  ( 54.89583333452979730, 40.00000000000000000, -3.599741573803383332 ) ) ;
#22102 = VECTOR ( 'NONE', #17664, 1000.000000000000000 ) ;
#22103 = CYLINDRICAL_SURFACE ( 'NONE', #10947, 116.0000000000000000 ) ;
#22104 = CYLINDRICAL_SURFACE ( 'NONE', #28461, 120.5010000000000190 ) ;
#22105 = CARTESIAN_POINT ( 'NONE',  ( 150.5000000000000284, 1.576403824487674918E-12, 9.999999999999998224 ) ) ;
#22106 = DIRECTION ( 'NONE',  ( -1.000000000000000000, -0.000000000000000000, 0.000000000000000000 ) ) ;
#22107 = ADVANCED_FACE ( 'NONE', ( #12634 ), #16336, .T. ) ;
#22108 = ORIENTED_EDGE ( 'NONE', *, *, #8656, .T. ) ;
#22109 = CARTESIAN_POINT ( 'NONE',  ( 24.02862666965263116, 40.00000000000000000, 27.38392887651082575 ) ) ;
#22110 = ORIENTED_EDGE ( 'NONE', *, *, #37465, .F. ) ;
#22111 = CARTESIAN_POINT ( 'NONE',  ( 17.99999999999999645, 89.07460286905850921, 81.15544420874991260 ) ) ;
#22112 = CARTESIAN_POINT ( 'NONE',  ( 0.000000000000000000, 0.000000000000000000, -1.199999999999999956 ) ) ;
#22113 = ORIENTED_EDGE ( 'NONE', *, *, #35560, .F. ) ;
#22114 = EDGE_CURVE ( 'NONE', #16254, #20926, #16312, .T. ) ;
#22115 = AXIS2_PLACEMENT_3D ( 'NONE', #7133, #30074, #13715 ) ;
#22116 = DIRECTION ( 'NONE',  ( -3.996523416598930318E-16, 2.658563593772947863E-15, 1.000000000000000000 ) ) ;
#22117 = VERTEX_POINT ( 'NONE', #22275 ) ;
#22118 = CARTESIAN_POINT ( 'NONE',  ( -8.749793197483596074, -2.055254544495723312, 2.972870684497275207 ) ) ;
#22119 = VERTEX_POINT ( 'NONE', #2564 ) ;
#22120 = AXIS2_PLACEMENT_3D ( 'NONE', #22194, #35447, #35227 ) ;
#22121 = VECTOR ( 'NONE', #9221, 1000.000000000000000 ) ;
#22122 = EDGE_LOOP ( 'NONE', ( #2858, #40024, #24693, #36223 ) ) ;
#22123 = VECTOR ( 'NONE', #8321, 1000.000000000000000 ) ;
#22124 = DIRECTION ( 'NONE',  ( 1.000000000000000000, 0.000000000000000000, 0.000000000000000000 ) ) ;
#22125 = CARTESIAN_POINT ( 'NONE',  ( -62.56443097448101298, 31.00000000000000355, -55.02758207457566897 ) ) ;
#22126 = EDGE_LOOP ( 'NONE', ( #25042, #21892, #3405, #655 ) ) ;
#22127 = DIRECTION ( 'NONE',  ( 0.000000000000000000, 0.000000000000000000, -1.000000000000000000 ) ) ;
#22128 = VECTOR ( 'NONE', #24412, 1000.000000000000000 ) ;
#22129 = LINE ( 'NONE', #8553, #7329 ) ;
#22130 = EDGE_LOOP ( 'NONE', ( #23516, #24043, #42755, #8879 ) ) ;
#22131 = DIRECTION ( 'NONE',  ( -1.000000000000000000, 0.000000000000000000, -0.000000000000000000 ) ) ;
#22132 = AXIS2_PLACEMENT_3D ( 'NONE', #42075, #38179, #29027 ) ;
#22133 = FACE_BOUND ( 'NONE', #38881, .T. ) ;
#22134 = VECTOR ( 'NONE', #11921, 1000.000000000000000 ) ;
#22135 = CARTESIAN_POINT ( 'NONE',  ( -22.06642698273766356, 31.00000000000000355, -2.901557744773885616 ) ) ;
#22136 = EDGE_CURVE ( 'NONE', #16671, #24120, #34409, .T. ) ;
#22138 = DIRECTION ( 'NONE',  ( 0.000000000000000000, 0.9048270524660176894, 0.4257792915650767118 ) ) ;
#22137 = FACE_BOUND ( 'NONE', #19259, .T. ) ;
#22139 = EDGE_CURVE ( 'NONE', #15632, #16730, #15923, .T. ) ;
#22140 = EDGE_CURVE ( 'NONE', #31470, #6447, #29010, .T. ) ;
#22141 = CARTESIAN_POINT ( 'NONE',  ( 18.00000000000000355, 24.47917365149946889, 45.87777302070943364 ) ) ;
#22142 = DIRECTION ( 'NONE',  ( -1.000000000000000000, -0.000000000000000000, -0.000000000000000000 ) ) ;
#22143 = ORIENTED_EDGE ( 'NONE', *, *, #40490, .T. ) ;
#22144 = EDGE_CURVE ( 'NONE', #5524, #41864, #31655, .T. ) ;
#22145 =( NAMED_UNIT ( * ) SI_UNIT ( $, .STERADIAN. ) SOLID_ANGLE_UNIT ( ) );
#22146 = VERTEX_POINT ( 'NONE', #15500 ) ;
#22147 = FACE_OUTER_BOUND ( 'NONE', #39125, .T. ) ;
#22148 = CARTESIAN_POINT ( 'NONE',  ( 31.25450476884064699, 31.00000000000000355, 92.02345382966369414 ) ) ;
#22149 = DIRECTION ( 'NONE',  ( -0.000000000000000000, -0.000000000000000000, 1.000000000000000000 ) ) ;
#22150 = CIRCLE ( 'NONE', #42297, 59.00000000000000000 ) ;
#22151 = ORIENTED_EDGE ( 'NONE', *, *, #496, .T. ) ;
#22152 = CARTESIAN_POINT ( 'NONE',  ( 17.42035916340572399, 40.00000000000000000, 19.85006075799527991 ) ) ;
#22153 = CARTESIAN_POINT ( 'NONE',  ( 28.62564328229377608, 40.00000000000000000, -21.88780996305825965 ) ) ;
#22154 = AXIS2_PLACEMENT_3D ( 'NONE', #1230, #21141, #37873 ) ;
#22155 = ORIENTED_EDGE ( 'NONE', *, *, #7347, .F. ) ;
#22156 = AXIS2_PLACEMENT_3D ( 'NONE', #41761, #38059, #28701 ) ;
#22157 = ADVANCED_FACE ( 'NONE', ( #36164 ), #6278, .T. ) ;
#22158 = ORIENTED_EDGE ( 'NONE', *, *, #23937, .F. ) ;
#22159 = DIRECTION ( 'NONE',  ( -1.000000000000000000, 0.000000000000000000, 0.000000000000000000 ) ) ;
#22160 = DIRECTION ( 'NONE',  ( -1.000000000000000000, 0.000000000000000000, 0.000000000000000000 ) ) ;
#22161 = DIRECTION ( 'NONE',  ( -1.000000000000000000, 0.000000000000000000, -0.000000000000000000 ) ) ;
#22162 = AXIS2_PLACEMENT_3D ( 'NONE', #34132, #7732, #3776 ) ;
#22163 = CARTESIAN_POINT ( 'NONE',  ( -2.344047193898593395, -3.265465875126480455, -1.054683074273691752E-14 ) ) ;
#22164 = CARTESIAN_POINT ( 'NONE',  ( 17.99999999999999645, -23.21237537461820466, 109.7700237000591414 ) ) ;
#22165 = ORIENTED_EDGE ( 'NONE', *, *, #30016, .F. ) ;
#22166 = DIRECTION ( 'NONE',  ( 0.8660254037844379305, 0.5000000000000013323, 0.000000000000000000 ) ) ;
#22167 = ORIENTED_EDGE ( 'NONE', *, *, #14770, .T. ) ;
#22168 = CARTESIAN_POINT ( 'NONE',  ( 17.99999999999999645, 91.65951123222582453, -71.09524597797991419 ) ) ;
#22169 = DIRECTION ( 'NONE',  ( 1.000000000000000000, -0.000000000000000000, 0.000000000000000000 ) ) ;
#22170 = AXIS2_PLACEMENT_3D ( 'NONE', #38442, #24546, #35170 ) ;
#22171 = CARTESIAN_POINT ( 'NONE',  ( 0.000000000000000000, 0.000000000000000000, 0.000000000000000000 ) ) ;
#22172 = CARTESIAN_POINT ( 'NONE',  ( 17.99999999999999645, -94.83915810436360516, -59.94836581341685644 ) ) ;
#22173 = ORIENTED_EDGE ( 'NONE', *, *, #37583, .T. ) ;
#22174 = ADVANCED_FACE ( 'NONE', ( #42278 ), #38575, .T. ) ;
#22175 = VERTEX_POINT ( 'NONE', #5639 ) ;
#22176 = CARTESIAN_POINT ( 'NONE',  ( 17.99999999999999645, 3.996885678774600326, -120.4346956066681713 ) ) ;
#22177 = ORIENTED_EDGE ( 'NONE', *, *, #24012, .F. ) ;
#22179 = ORIENTED_EDGE ( 'NONE', *, *, #24683, .F. ) ;
#22178 = DIRECTION ( 'NONE',  ( -3.009274222672345096E-17, -1.000000000000000000, 2.455023325076454960E-18 ) ) ;
#22180 = CARTESIAN_POINT ( 'NONE',  ( -44.44570800417318424, 31.00000000000000355, 25.56477902013656589 ) ) ;
#22181 = EDGE_LOOP ( 'NONE', ( #3273, #7353, #10751, #12112 ) ) ;
#22182 = CARTESIAN_POINT ( 'NONE',  ( 17.99999999999999645, 0.000000000000000000, 0.000000000000000000 ) ) ;
#22183 = CIRCLE ( 'NONE', #29133, 58.99999999999998579 ) ;
#22184 = CIRCLE ( 'NONE', #13098, 116.0000000000000000 ) ;
#22185 = DIRECTION ( 'NONE',  ( 0.000000000000000000, 0.5264321628773570572, -0.8502171357296134380 ) ) ;
#22186 = VERTEX_POINT ( 'NONE', #42056 ) ;
#22187 = AXIS2_PLACEMENT_3D ( 'NONE', #6149, #15367, #19495 ) ;
#22188 = CARTESIAN_POINT ( 'NONE',  ( 76.90008882636699639, 39.99999999999999289, -4.923574515426283327 ) ) ;
#22189 = ADVANCED_FACE ( 'NONE', ( #19841 ), #583, .F. ) ;
#22190 = VECTOR ( 'NONE', #32787, 1000.000000000000000 ) ;
#22192 = LINE ( 'NONE', #4917, #22134 ) ;
#22191 = DIRECTION ( 'NONE',  ( 0.000000000000000000, -0.8477344278896755680, 0.5304209081197350795 ) ) ;
#22193 = EDGE_CURVE ( 'NONE', #33557, #14757, #30936, .T. ) ;
#22194 = CARTESIAN_POINT ( 'NONE',  ( 2.027755760259328333E-13, -150.5000000000013642, 9.999999999999587885 ) ) ;
#22195 = VERTEX_POINT ( 'NONE', #36813 ) ;
#22196 = DIRECTION ( 'NONE',  ( -3.996523416598930318E-16, 2.658563593772947863E-15, 1.000000000000000000 ) ) ;
#22197 = ORIENTED_EDGE ( 'NONE', *, *, #29497, .T. ) ;
#22198 =( NAMED_UNIT ( * ) SI_UNIT ( $, .STERADIAN. ) SOLID_ANGLE_UNIT ( ) );
#22199 = DIRECTION ( 'NONE',  ( 0.000000000000000000, 0.000000000000000000, 1.000000000000000000 ) ) ;
#22200 = CARTESIAN_POINT ( 'NONE',  ( 0.000000000000000000, 79.18387647320879807, -84.76976882518680156 ) ) ;
#22201 = VECTOR ( 'NONE', #16306, 1000.000000000000000 ) ;
#22202 = CARTESIAN_POINT ( 'NONE',  ( -67.35649507452052376, 31.00000000000000711, 18.04843207638801772 ) ) ;
#22204 = FACE_OUTER_BOUND ( 'NONE', #137, .T. ) ;
#22203 = DIRECTION ( 'NONE',  ( -1.000000000000000000, 0.000000000000000000, -0.000000000000000000 ) ) ;
#22205 = EDGE_LOOP ( 'NONE', ( #16691, #10373, #30989, #33925 ) ) ;
#22206 = ADVANCED_FACE ( 'NONE', ( #20712 ), #20278, .F. ) ;
#22207 = DIRECTION ( 'NONE',  ( 0.000000000000000000, 0.000000000000000000, 1.000000000000000000 ) ) ;
#22208 = EDGE_CURVE ( 'NONE', #25826, #6975, #4436, .T. ) ;
#22209 = ORIENTED_EDGE ( 'NONE', *, *, #15410, .F. ) ;
#22210 = DIRECTION ( 'NONE',  ( -1.000000000000000000, 0.000000000000000000, -0.000000000000000000 ) ) ;
#22211 = DIRECTION ( 'NONE',  ( 0.000000000000000000, 0.000000000000000000, 1.000000000000000000 ) ) ;
#22212 = CIRCLE ( 'NONE', #33997, 20.00000000000000000 ) ;
#22213 = CARTESIAN_POINT ( 'NONE',  ( 6.309545988805660421, 31.00000000000000355, -94.59213238968112591 ) ) ;
#22214 = CARTESIAN_POINT ( 'NONE',  ( 12.87762912549411354, 40.00000000000000000, 98.66289914827740404 ) ) ;
#22215 = ADVANCED_FACE ( 'NONE', ( #16576 ), #29875, .T. ) ;
#22216 = CARTESIAN_POINT ( 'NONE',  ( 17.99999999999999645, 0.000000000000000000, 0.000000000000000000 ) ) ;
#22217 = AXIS2_PLACEMENT_3D ( 'NONE', #5205, #24902, #38156 ) ;
#22218 = CIRCLE ( 'NONE', #38882, 116.0000000000000000 ) ;
#22219 = ORIENTED_EDGE ( 'NONE', *, *, #9446, .T. ) ;
#22220 = DIRECTION ( 'NONE',  ( 0.000000000000000000, 0.3681245526846786964, -0.9297764858882511252 ) ) ;
#22221 = CIRCLE ( 'NONE', #39559, 7.500000000000000000 ) ;
#22222 = VERTEX_POINT ( 'NONE', #136 ) ;
#22223 = CIRCLE ( 'NONE', #10340, 120.5010000000000332 ) ;
#22224 = CARTESIAN_POINT ( 'NONE',  ( 0.000000000000000000, 23.21237537461889389, -109.7700237000589709 ) ) ;
#22225 = AXIS2_PLACEMENT_3D ( 'NONE', #18203, #37992, #21689 ) ;
#22227 = VERTEX_POINT ( 'NONE', #40501 ) ;
#22226 = DIRECTION ( 'NONE',  ( 1.000000000000000000, 0.000000000000000000, 0.000000000000000000 ) ) ;
#22228 = DIRECTION ( 'NONE',  ( 1.000000000000000000, 0.000000000000000000, 0.000000000000000000 ) ) ;
#22229 = EDGE_LOOP ( 'NONE', ( #12442, #4257 ) ) ;
#22230 = DIRECTION ( 'NONE',  ( -1.000000000000000000, 0.000000000000000000, 0.000000000000000000 ) ) ;
#22231 = CARTESIAN_POINT ( 'NONE',  ( 9.000000000000001776, 49.25004636492388244, 16.68630974939776834 ) ) ;
#22232 = LINE ( 'NONE', #34841, #29216 ) ;
#22233 = ORIENTED_EDGE ( 'NONE', *, *, #25492, .T. ) ;
#22234 = CARTESIAN_POINT ( 'NONE',  ( 8.075107282080610460, 31.00000000000000355, -23.73893940452553508 ) ) ;
#22235 = CARTESIAN_POINT ( 'NONE',  ( -8.749793197483592522, 117.9447454555042754, 2.972870684497274762 ) ) ;
#22237 = ORIENTED_EDGE ( 'NONE', *, *, #18450, .T. ) ;
#22236 = CARTESIAN_POINT ( 'NONE',  ( 17.99999999999999645, 0.000000000000000000, 0.000000000000000000 ) ) ;
#22238 = EDGE_LOOP ( 'NONE', ( #33932, #23031, #33470, #4943 ) ) ;
#22239 = CARTESIAN_POINT ( 'NONE',  ( 0.000000000000000000, -7.749090474611723067, 30.53094492177210384 ) ) ;
#22240 = CARTESIAN_POINT ( 'NONE',  ( 18.00000000000000355, -49.25004636492376164, -16.68630974939811651 ) ) ;
#22241 = CARTESIAN_POINT ( 'NONE',  ( -41.92568936861482598, 40.00000000000000000, -5.596851440153165491 ) ) ;
#22242 = CARTESIAN_POINT ( 'NONE',  ( 17.99999999999999645, 35.54274411428057334, 115.1399337407607959 ) ) ;
#22243 = AXIS2_PLACEMENT_3D ( 'NONE', #16850, #9624, #26639 ) ;
#22244 = AXIS2_PLACEMENT_3D ( 'NONE', #17707, #37939, #30977 ) ;
#22245 = DIRECTION ( 'NONE',  ( 1.000000000000000000, 0.000000000000000000, 0.000000000000000000 ) ) ;
#22246 = ADVANCED_FACE ( 'NONE', ( #43138 ), #26791, .F. ) ;
#22247 = DIRECTION ( 'NONE',  ( 1.000000000000000000, -0.000000000000000000, -0.000000000000000000 ) ) ;
#22248 = ORIENTED_EDGE ( 'NONE', *, *, #28900, .T. ) ;
#22249 = CIRCLE ( 'NONE', #8964, 13.40000000000000213 ) ;
#22250 = DIRECTION ( 'NONE',  ( -1.000000000000000000, 0.000000000000000000, 0.000000000000000000 ) ) ;
#22251 = EDGE_CURVE ( 'NONE', #40285, #31747, #26795, .T. ) ;
#22252 = ORIENTED_EDGE ( 'NONE', *, *, #16787, .F. ) ;
#22253 = LINE ( 'NONE', #2315, #4346 ) ;
#22254 = FACE_OUTER_BOUND ( 'NONE', #31120, .T. ) ;
#22255 = CARTESIAN_POINT ( 'NONE',  ( 11.92156526682413720, 31.00000000000000355, 35.08788755311113761 ) ) ;
#22256 = ORIENTED_EDGE ( 'NONE', *, *, #19929, .T. ) ;
#22257 = DIRECTION ( 'NONE',  ( 0.000000000000000000, 0.000000000000000000, 1.000000000000000000 ) ) ;
#22258 = EDGE_LOOP ( 'NONE', ( #12915, #37004, #18918, #34586 ) ) ;
#22259 = EDGE_CURVE ( 'NONE', #36059, #10415, #37242, .T. ) ;
#22260 = CARTESIAN_POINT ( 'NONE',  ( -6.199999999999997513, 4.693303851024319376E-15, 0.000000000000000000 ) ) ;
#22261 = CARTESIAN_POINT ( 'NONE',  ( 68.41617299536980568, 31.00000000000000000, 52.47886963225217016 ) ) ;
#22262 = EDGE_CURVE ( 'NONE', #10364, #19109, #17440, .T. ) ;
#22263 = CARTESIAN_POINT ( 'NONE',  ( 1.600000000000000089, -12.75000000000000000, -1.199999999999999956 ) ) ;
#22264 = EDGE_LOOP ( 'NONE', ( #25201, #29781, #26338, #12876 ) ) ;
#22265 = CARTESIAN_POINT ( 'NONE',  ( 55.55275676652586725, 31.00000000000000355, 14.97830846782891356 ) ) ;
#22266 = CARTESIAN_POINT ( 'NONE',  ( 25.17870271038170316, 40.00000000000000000, 93.97695291299892517 ) ) ;
#22267 = ORIENTED_EDGE ( 'NONE', *, *, #7104, .F. ) ;
#22268 = CARTESIAN_POINT ( 'NONE',  ( 17.99999999999999645, 7.749090474611950441, -30.53094492177204700 ) ) ;
#22269 = CARTESIAN_POINT ( 'NONE',  ( -5.991980000000000750, 0.000000000000000000, 0.000000000000000000 ) ) ;
#22270 = DIRECTION ( 'NONE',  ( -1.000000000000000000, 0.000000000000000000, 0.000000000000000000 ) ) ;
#22271 = VECTOR ( 'NONE', #29334, 1000.000000000000000 ) ;
#22272 = AXIS2_PLACEMENT_3D ( 'NONE', #13026, #16290, #19373 ) ;
#22274 = ORIENTED_EDGE ( 'NONE', *, *, #25485, .F. ) ;
#22273 = CARTESIAN_POINT ( 'NONE',  ( 18.00000000000000355, 50.95304419620838132, -10.38206564895608786 ) ) ;
#22275 = CARTESIAN_POINT ( 'NONE',  ( 142.5000000000000284, 0.000000000000000000, -25.00000000000000000 ) ) ;
#22276 = CARTESIAN_POINT ( 'NONE',  ( 4.211140560182196957, 2.431303136016536470, -3.745885042887433514 ) ) ;
#22277 = ORIENTED_EDGE ( 'NONE', *, *, #8866, .F. ) ;
#22278 = CARTESIAN_POINT ( 'NONE',  ( -34.66105084696506822, 40.00000000000000000, 70.31756248751102589 ) ) ;
#22279 = LINE ( 'NONE', #25756, #16656 ) ;
#22280 = EDGE_CURVE ( 'NONE', #1458, #42747, #10053, .T. ) ;
#22281 = ORIENTED_EDGE ( 'NONE', *, *, #39936, .T. ) ;
#22282 = ADVANCED_FACE ( 'NONE', ( #3838 ), #9772, .T. ) ;
#22283 = CARTESIAN_POINT ( 'NONE',  ( 0.000000000000000000, 41.60679253225906393, -108.2814610871942165 ) ) ;
#22284 = VERTEX_POINT ( 'NONE', #36372 ) ;
#22285 = ORIENTED_EDGE ( 'NONE', *, *, #35665, .T. ) ;
#22286 = CARTESIAN_POINT ( 'NONE',  ( 18.00000000000000355, 46.77034588191335729, -22.72740077717179474 ) ) ;
#22287 = ORIENTED_EDGE ( 'NONE', *, *, #26625, .T. ) ;
#22288 = DIRECTION ( 'NONE',  ( 0.000000000000000000, 0.5528000653611945259, -0.8333139190825142872 ) ) ;
#22289 = LINE ( 'NONE', #41875, #15152 ) ;
#22290 = LINE ( 'NONE', #1520, #42783 ) ;
#22291 = CARTESIAN_POINT ( 'NONE',  ( 18.00000000000000355, 0.000000000000000000, 51.99999999999999289 ) ) ;
#22292 = ORIENTED_EDGE ( 'NONE', *, *, #5575, .T. ) ;
#22293 = FACE_OUTER_BOUND ( 'NONE', #11884, .T. ) ;
#22294 = ORIENTED_EDGE ( 'NONE', *, *, #1017, .F. ) ;
#22295 = DIRECTION ( 'NONE',  ( -1.000000000000000000, -0.000000000000000000, -0.000000000000000000 ) ) ;
#22296 = AXIS2_PLACEMENT_3D ( 'NONE', #12753, #39321, #9459 ) ;
#22297 = ORIENTED_EDGE ( 'NONE', *, *, #42674, .T. ) ;
#22298 = CIRCLE ( 'NONE', #41745, 31.49899999999999878 ) ;
#22299 = CYLINDRICAL_SURFACE ( 'NONE', #35025, 58.99999999999999289 ) ;
#22300 = DIRECTION ( 'NONE',  ( -1.000000000000000000, -0.000000000000000000, -0.000000000000000000 ) ) ;
#22301 = EDGE_CURVE ( 'NONE', #33164, #2232, #353, .T. ) ;
#22302 = CIRCLE ( 'NONE', #27861, 13.59999999999999787 ) ;
#22303 = DIRECTION ( 'NONE',  ( 6.413747168845437910E-31, 1.000000000000000000, 6.123233995736766036E-17 ) ) ;
#22304 = EDGE_CURVE ( 'NONE', #4569, #29068, #41409, .T. ) ;
#22305 = DIRECTION ( 'NONE',  ( 0.000000000000000000, 0.000000000000000000, 1.000000000000000000 ) ) ;
#22306 = CARTESIAN_POINT ( 'NONE',  ( 48.10206620145878276, 31.00000000000000355, -42.20136231105875879 ) ) ;
#22307 = VERTEX_POINT ( 'NONE', #37239 ) ;
#22308 = CYLINDRICAL_SURFACE ( 'NONE', #25505, 20.00000000000000355 ) ;
#22309 = ADVANCED_FACE ( 'NONE', ( #16790 ), #7354, .F. ) ;
#22310 = ORIENTED_EDGE ( 'NONE', *, *, #34108, .T. ) ;
#22311 = EDGE_CURVE ( 'NONE', #40032, #25931, #30076, .T. ) ;
#22312 = CARTESIAN_POINT ( 'NONE',  ( -25.79802671946675474, 40.00000000000000000, 52.34090327860478453 ) ) ;
#22313 = CARTESIAN_POINT ( 'NONE',  ( 0.000000000000000000, 0.000000000000000000, 0.000000000000000000 ) ) ;
#22314 = DIRECTION ( 'NONE',  ( -1.000000000000000000, -0.000000000000000000, -0.000000000000000000 ) ) ;
#22315 = FACE_BOUND ( 'NONE', #3055, .T. ) ;
#22316 = CARTESIAN_POINT ( 'NONE',  ( 18.00000000000000355, 0.000000000000000000, 0.000000000000000000 ) ) ;
#22317 = ORIENTED_EDGE ( 'NONE', *, *, #36013, .F. ) ;
#22318 = CARTESIAN_POINT ( 'NONE',  ( 16.30133787010129254, 40.00000000000000000, 33.04822796959624753 ) ) ;
#22319 = EDGE_LOOP ( 'NONE', ( #21264, #1158, #34575, #13455 ) ) ;
#22320 = DIRECTION ( 'NONE',  ( 1.000000000000000000, 0.000000000000000000, 0.000000000000000000 ) ) ;
#22322 = DIRECTION ( 'NONE',  ( 0.000000000000000000, 0.000000000000000000, 1.000000000000000000 ) ) ;
#22321 = AXIS2_PLACEMENT_3D ( 'NONE', #3158, #16097, #29396 ) ;
#22323 = CIRCLE ( 'NONE', #25797, 126.0000000000000284 ) ;
#22324 = ORIENTED_EDGE ( 'NONE', *, *, #8906, .T. ) ;
#22326 = EDGE_CURVE ( 'NONE', #41828, #21131, #35821, .T. ) ;
#22325 = VECTOR ( 'NONE', #13789, 1000.000000000000114 ) ;
#22327 = CARTESIAN_POINT ( 'NONE',  ( -158.5000000000000284, 2.597717496998778441E-13, 6.999999999999939604 ) ) ;
#22328 = ADVANCED_FACE ( 'NONE', ( #1009 ), #15017, .T. ) ;
#22329 = ORIENTED_EDGE ( 'NONE', *, *, #6756, .F. ) ;
#22330 = CARTESIAN_POINT ( 'NONE',  ( 0.000000000000000000, -19.69434969228056787, -24.58291258574069360 ) ) ;
#22331 = ORIENTED_EDGE ( 'NONE', *, *, #24308, .F. ) ;
#22332 = EDGE_LOOP ( 'NONE', ( #22209, #23064, #15510, #18515 ) ) ;
#22333 = CARTESIAN_POINT ( 'NONE',  ( 0.000000000000000000, 14.84191762912354839, -27.78316904333109960 ) ) ;
#22334 = CARTESIAN_POINT ( 'NONE',  ( -70.49178429274641644, 31.00000000000000711, 40.57739572807859929 ) ) ;
#22335 = ORIENTED_EDGE ( 'NONE', *, *, #3451, .T. ) ;
#22336 = CARTESIAN_POINT ( 'NONE',  ( 0.2142857142857142738, -10.49781318335647917, -1.199999999999999956 ) ) ;
#22337 = CARTESIAN_POINT ( 'NONE',  ( 17.99999999999999645, 0.000000000000000000, 0.000000000000000000 ) ) ;
#22338 = ORIENTED_EDGE ( 'NONE', *, *, #42405, .F. ) ;
#22339 = PLANE ( 'NONE',  #36333 ) ;
#22340 = DIRECTION ( 'NONE',  ( 1.000000000000000000, 0.000000000000000000, 0.000000000000000000 ) ) ;
#22341 = CARTESIAN_POINT ( 'NONE',  ( -22.00000000000000000, 31.00000000000000355, 0.000000000000000000 ) ) ;
#22343 = DIRECTION ( 'NONE',  ( 0.000000000000000000, 1.000000000000000000, -1.287488025362403787E-15 ) ) ;
#22342 = CARTESIAN_POINT ( 'NONE',  ( 2.500000000000000000, 0.000000000000000000, 0.000000000000000000 ) ) ;
#22344 = CARTESIAN_POINT ( 'NONE',  ( -1.472621547668719444, 31.00000000000000355, -22.39583333634585571 ) ) ;
#22345 = DIRECTION ( 'NONE',  ( -1.000000000000000000, 0.000000000000000000, 0.000000000000000000 ) ) ;
#22346 = B_SPLINE_CURVE_WITH_KNOTS ( 'NONE', 3,
 ( #40118, #17702, #30334, #17486, #3894, #23600, #30767, #40549 ),
 .UNSPECIFIED., .F., .F.,
 ( 4, 2, 2, 4 ),
 ( 0.000000000000000000, 0.002450665683189818828, 0.003675998524784728459, 0.004901331366379638524 ),
 .UNSPECIFIED. ) ;
#22347 = ORIENTED_EDGE ( 'NONE', *, *, #23450, .T. ) ;
#22348 = SHAPE_REPRESENTATION_RELATIONSHIP ( 'NONE' , 'NONE' ,  #7878, #10920 ) ;
#22349 = EDGE_CURVE ( 'NONE', #33209, #35721, #25422, .T. ) ;
#22350 = AXIS2_PLACEMENT_3D ( 'NONE', #41414, #25322, #1713 ) ;
#22351 = VERTEX_POINT ( 'NONE', #4737 ) ;
#22352 = DIRECTION ( 'NONE',  ( -1.000000000000000000, 0.000000000000000000, 0.000000000000000000 ) ) ;
#22353 = CIRCLE ( 'NONE', #40416, 20.00000000000000355 ) ;
#22354 = EDGE_CURVE ( 'NONE', #42436, #5524, #30287, .T. ) ;
#22355 = CIRCLE ( 'NONE', #27922, 13.59999999999999964 ) ;
#22356 = FACE_OUTER_BOUND ( 'NONE', #250, .T. ) ;
#22357 = ORIENTED_EDGE ( 'NONE', *, *, #34915, .F. ) ;
#22358 = CIRCLE ( 'NONE', #2785, 15.00000000000000000 ) ;
#22359 = CARTESIAN_POINT ( 'NONE',  ( 13.36968668718156295, 40.00000000000000000, 23.13838826010315941 ) ) ;
#22360 = CARTESIAN_POINT ( 'NONE',  ( -41.52979953745317232, 40.00000000000000000, 5.398177843167591305 ) ) ;
#22361 = VERTEX_POINT ( 'NONE', #31364 ) ;
#22363 = ORIENTED_EDGE ( 'NONE', *, *, #30085, .T. ) ;
#22362 = B_SPLINE_CURVE_WITH_KNOTS ( 'NONE', 3,
 ( #24262, #37942, #1070, #11354, #17287, #34683 ),
 .UNSPECIFIED., .F., .F.,
 ( 4, 2, 4 ),
 ( 0.003358874760055550156, 0.004541967308452096383, 0.005725059856848641743 ),
 .UNSPECIFIED. ) ;
#22364 = DIRECTION ( 'NONE',  ( 0.000000000000000000, 0.000000000000000000, 1.000000000000000000 ) ) ;
#22365 = CARTESIAN_POINT ( 'NONE',  ( 17.99999999999999645, 63.55543939553896848, -97.03971415477259654 ) ) ;
#22366 = CARTESIAN_POINT ( 'NONE',  ( 17.99999999999999645, -27.83061035787034498, 117.2431154827796576 ) ) ;
#22367 = DIRECTION ( 'NONE',  ( 0.000000000000000000, 0.000000000000000000, 1.000000000000000000 ) ) ;
#22368 = VERTEX_POINT ( 'NONE', #41592 ) ;
#22369 = DIRECTION ( 'NONE',  ( 1.000000000000000000, 0.000000000000000000, 0.000000000000000000 ) ) ;
#22370 = ORIENTED_EDGE ( 'NONE', *, *, #15658, .F. ) ;
#22371 = DIRECTION ( 'NONE',  ( -1.000000000000000000, -0.000000000000000000, 0.000000000000000000 ) ) ;
#22372 = CARTESIAN_POINT ( 'NONE',  ( 17.99999999999999645, -89.07460286905904923, 81.15544420874930154 ) ) ;
#22373 = EDGE_CURVE ( 'NONE', #6418, #9950, #26120, .T. ) ;
#22374 = CIRCLE ( 'NONE', #36956, 14.70000000000000107 ) ;
#22375 = EDGE_CURVE ( 'NONE', #10415, #3709, #18493, .T. ) ;
#22376 = CARTESIAN_POINT ( 'NONE',  ( 104.9999999999993321, -2.293336392629658115E-13, -32.00000000000000000 ) ) ;
#22377 = EDGE_CURVE ( 'NONE', #508, #5301, #24748, .T. ) ;
#22378 = EDGE_CURVE ( 'NONE', #32231, #41864, #42797, .T. ) ;
#22379 = CYLINDRICAL_SURFACE ( 'NONE', #26857, 120.5010000000000190 ) ;
#22380 = ORIENTED_EDGE ( 'NONE', *, *, #1131, .F. ) ;
#22381 = CARTESIAN_POINT ( 'NONE',  ( 12.74197863150380883, 40.00000000000000000, 96.66318596537892915 ) ) ;
#22382 = ORIENTED_EDGE ( 'NONE', *, *, #12200, .T. ) ;
#22383 = AXIS2_PLACEMENT_3D ( 'NONE', #34422, #15276, #11982 ) ;
#22384 = FACE_OUTER_BOUND ( 'NONE', #37592, .T. ) ;
#22385 = VECTOR ( 'NONE', #32432, 1000.000000000000000 ) ;
#22386 = ORIENTED_EDGE ( 'NONE', *, *, #14195, .F. ) ;
#22388 = ORIENTED_EDGE ( 'NONE', *, *, #8656, .F. ) ;
#22387 = CYLINDRICAL_SURFACE ( 'NONE', #27163, 64.99999999999997158 ) ;
#22389 = CIRCLE ( 'NONE', #10540, 20.00000000000001066 ) ;
#22390 = CARTESIAN_POINT ( 'NONE',  ( -51.46673616000524021, 31.00000000000000355, 6.691140578787329041 ) ) ;
#22392 = EDGE_LOOP ( 'NONE', ( #27402, #32366, #4129, #41057 ) ) ;
#22391 = AXIS2_PLACEMENT_3D ( 'NONE', #12864, #19645, #32911 ) ;
#22393 = DIRECTION ( 'NONE',  ( 0.000000000000000000, 0.000000000000000000, 1.000000000000000000 ) ) ;
#22394 = CIRCLE ( 'NONE', #27953, 47.49900000000000233 ) ;
#22395 = EDGE_CURVE ( 'NONE', #33958, #4060, #22653, .T. ) ;
#22396 = CARTESIAN_POINT ( 'NONE',  ( -150.4999999999986926, -2.921102061156358310E-13, 10.00000000000004619 ) ) ;
#22397 = ORIENTED_EDGE ( 'NONE', *, *, #6275, .F. ) ;
#22398 = CARTESIAN_POINT ( 'NONE',  ( 76.30724621505197547, 39.99999999999999289, -9.942258256684034734 ) ) ;
#22400 = DIRECTION ( 'NONE',  ( 0.000000000000000000, 0.3140767120219495334, -0.9493976084683810601 ) ) ;
#22399 = CARTESIAN_POINT ( 'NONE',  ( 17.99999999999999645, 103.5682682299982673, 43.14958040911701431 ) ) ;
#22401 = DIRECTION ( 'NONE',  ( -1.000000000000000000, -0.000000000000000000, -0.000000000000000000 ) ) ;
#22402 = ORIENTED_EDGE ( 'NONE', *, *, #40787, .F. ) ;
#22403 = CARTESIAN_POINT ( 'NONE',  ( 0.000000000000000000, 101.8011932243948081, 55.61040422519366189 ) ) ;
#22404 = ORIENTED_EDGE ( 'NONE', *, *, #17600, .T. ) ;
#22405 = CARTESIAN_POINT ( 'NONE',  ( -2.107686228591307694E-13, 150.5000000000013642, 10.00000000000041744 ) ) ;
#22406 = FACE_OUTER_BOUND ( 'NONE', #37098, .T. ) ;
#22407 = CARTESIAN_POINT ( 'NONE',  ( -41.80404827410195168, 31.00000000000000355, 54.50178954758867889 ) ) ;
#22409 = DIRECTION ( 'NONE',  ( 0.000000000000000000, 0.000000000000000000, 1.000000000000000000 ) ) ;
#22408 = CARTESIAN_POINT ( 'NONE',  ( 11.90854556226686789, -40.05525454449572464, -74.83297477053821467 ) ) ;
#22410 = ORIENTED_EDGE ( 'NONE', *, *, #2898, .T. ) ;
#22411 = AXIS2_PLACEMENT_3D ( 'NONE', #24820, #1206, #40906 ) ;
#22412 = VECTOR ( 'NONE', #12916, 1000.000000000000000 ) ;
#22413 = EDGE_LOOP ( 'NONE', ( #2246, #24083 ) ) ;
#22414 = DIRECTION ( 'NONE',  ( 0.000000000000000000, 0.000000000000000000, 1.000000000000000000 ) ) ;
#22415 = DIRECTION ( 'NONE',  ( 1.000000000000000000, 0.000000000000000000, 0.000000000000000000 ) ) ;
#22416 = CARTESIAN_POINT ( 'NONE',  ( 25.57473013255608052, 31.00000000000000355, 95.94174708837350352 ) ) ;
#22417 = CARTESIAN_POINT ( 'NONE',  ( -80.50242771303932443, 40.00000000000000711, -46.62292012066232871 ) ) ;
#22418 = AXIS2_PLACEMENT_3D ( 'NONE', #32640, #2715, #2090 ) ;
#22419 = LINE ( 'NONE', #25472, #33715 ) ;
#22420 = VERTEX_POINT ( 'NONE', #21800 ) ;
#22421 = FACE_OUTER_BOUND ( 'NONE', #24239, .T. ) ;
#22422 = ORIENTED_EDGE ( 'NONE', *, *, #39473, .F. ) ;
#22423 = AXIS2_PLACEMENT_3D ( 'NONE', #40314, #43159, #10448 ) ;
#22424 = DIRECTION ( 'NONE',  ( 1.000000000000000000, 0.000000000000000000, 0.000000000000000000 ) ) ;
#22426 = ORIENTED_EDGE ( 'NONE', *, *, #7710, .F. ) ;
#22425 = DIRECTION ( 'NONE',  ( 1.000000000000000000, -0.000000000000000000, -0.000000000000000000 ) ) ;
#22427 = EDGE_CURVE ( 'NONE', #5856, #35004, #37462, .T. ) ;
#22428 = EDGE_CURVE ( 'NONE', #19624, #3495, #14150, .T. ) ;
#22429 = DIRECTION ( 'NONE',  ( 0.000000000000000000, 0.000000000000000000, 1.000000000000000000 ) ) ;
#22430 = ORIENTED_EDGE ( 'NONE', *, *, #34223, .T. ) ;
#22431 = LINE ( 'NONE', #32210, #6356 ) ;
#22432 = CARTESIAN_POINT ( 'NONE',  ( 0.000000000000000000, 0.000000000000000000, -20.00000000000000000 ) ) ;
#22433 = EDGE_CURVE ( 'NONE', #2044, #22037, #24049, .T. ) ;
#22434 = AXIS2_PLACEMENT_3D ( 'NONE', #12894, #15752, #2812 ) ;
#22435 = DIRECTION ( 'NONE',  ( -1.847415842360817977E-16, 1.000000000000000000, 0.000000000000000000 ) ) ;
#22436 = EDGE_LOOP ( 'NONE', ( #2859, #39689, #24033, #40188 ) ) ;
#22437 = CARTESIAN_POINT ( 'NONE',  ( -6.237032369604345483, 31.00000000000000355, -23.31551866006812190 ) ) ;
#22438 = CARTESIAN_POINT ( 'NONE',  ( 17.99999999999999645, 107.2703412112699368, -32.88383143828351507 ) ) ;
#22439 = EDGE_CURVE ( 'NONE', #21953, #42630, #4952, .T. ) ;
#22441 = VERTEX_POINT ( 'NONE', #35046 ) ;
#22440 = DIRECTION ( 'NONE',  ( 0.000000000000000000, -0.5963673585385078635, 0.8027116379309588989 ) ) ;
#22442 = ORIENTED_EDGE ( 'NONE', *, *, #25834, .F. ) ;
#22443 = DIRECTION ( 'NONE',  ( 3.996523416598930318E-16, -2.658563593772947863E-15, -1.000000000000000000 ) ) ;
#22444 = AXIS2_PLACEMENT_3D ( 'NONE', #33451, #3539, #38437 ) ;
#22445 = CARTESIAN_POINT ( 'NONE',  ( 17.99999999999999645, -119.0898412705475522, 18.38751498043690802 ) ) ;
#22446 = CARTESIAN_POINT ( 'NONE',  ( 27.84166646521873645, 40.00000000000000000, -36.16032403486059366 ) ) ;
#22447 = CYLINDRICAL_SURFACE ( 'NONE', #6262, 116.0000000000000000 ) ;
#22448 = CIRCLE ( 'NONE', #3532, 116.0000000000000000 ) ;
#22449 = ADVANCED_FACE ( 'NONE', ( #24198 ), #38107, .T. ) ;
#22450 = DIRECTION ( 'NONE',  ( -1.000000000000000000, 0.000000000000000000, 0.000000000000000000 ) ) ;
#22451 = VECTOR ( 'NONE', #28271, 1000.000000000000000 ) ;
#22452 = DIRECTION ( 'NONE',  ( -1.000000000000000000, 0.000000000000000000, 0.000000000000000000 ) ) ;
#22453 = VERTEX_POINT ( 'NONE', #1663 ) ;
#22454 = DIRECTION ( 'NONE',  ( -1.000000000000000000, -0.000000000000000000, 0.000000000000000000 ) ) ;
#22455 = ORIENTED_EDGE ( 'NONE', *, *, #35361, .F. ) ;
#22456 = AXIS2_PLACEMENT_3D ( 'NONE', #30199, #37151, #258 ) ;
#22457 = DIRECTION ( 'NONE',  ( 1.000000000000000000, 0.000000000000000000, 0.000000000000000000 ) ) ;
#22458 = DIRECTION ( 'NONE',  ( 0.000000000000000000, 0.000000000000000000, 1.000000000000000000 ) ) ;
#22459 = CARTESIAN_POINT ( 'NONE',  ( -38.45388554590046937, 31.00000000000000355, -13.05014827191142679 ) ) ;
#22460 = ORIENTED_EDGE ( 'NONE', *, *, #6317, .F. ) ;
#22461 = CYLINDRICAL_SURFACE ( 'NONE', #9291, 47.49900000000000233 ) ;
#22462 = ORIENTED_EDGE ( 'NONE', *, *, #12858, .F. ) ;
#22463 = EDGE_CURVE ( 'NONE', #5697, #25155, #3764, .T. ) ;
#22464 = PRODUCT_DEFINITION_SHAPE ( 'NONE', 'NONE',  #43196 ) ;
#22465 = CARTESIAN_POINT ( 'NONE',  ( 9.000000000000001776, 36.06787431788676912, 37.45808914225501951 ) ) ;
#22466 = CARTESIAN_POINT ( 'NONE',  ( 46.76839422403993751, 31.00000000000000000, -81.00140361174831583 ) ) ;
#22467 = CARTESIAN_POINT ( 'NONE',  ( 17.99999999999999645, -29.03409033315573851, -12.21509719675420946 ) ) ;
#22468 = EDGE_LOOP ( 'NONE', ( #17542, #27571, #35109, #32712 ) ) ;
#22469 = CARTESIAN_POINT ( 'NONE',  ( 54.03410584561684260, 31.00000000000000355, 41.58544482236945328 ) ) ;
#22470 = CARTESIAN_POINT ( 'NONE',  ( 52.50410707185378811, 39.99999999999999289, -40.15145572477544533 ) ) ;
#22471 = FACE_OUTER_BOUND ( 'NONE', #7531, .T. ) ;
#22472 = ORIENTED_EDGE ( 'NONE', *, *, #32672, .F. ) ;
#22473 = CIRCLE ( 'NONE', #11301, 2.649999999999985700 ) ;
#22474 = LINE ( 'NONE', #16784, #42931 ) ;
#22475 = VECTOR ( 'NONE', #2940, 1000.000000000000000 ) ;
#22476 = DIRECTION ( 'NONE',  ( 3.996523416598930318E-16, -2.658563593772947863E-15, -1.000000000000000000 ) ) ;
#22477 = CARTESIAN_POINT ( 'NONE',  ( 50.00005079999999680, 0.000000000000000000, 15.00000000000000000 ) ) ;
#22478 = AXIS2_PLACEMENT_3D ( 'NONE', #20544, #17710, #40999 ) ;
#22480 = ORIENTED_EDGE ( 'NONE', *, *, #21835, .F. ) ;
#22479 = DIRECTION ( 'NONE',  ( -1.000000000000000000, -0.000000000000000000, -0.000000000000000000 ) ) ;
#22481 = EDGE_CURVE ( 'NONE', #10354, #6259, #29603, .T. ) ;
#22482 = DIRECTION ( 'NONE',  ( -1.000000000000000000, -0.000000000000000000, 0.000000000000000000 ) ) ;
#22483 = FACE_OUTER_BOUND ( 'NONE', #30614, .T. ) ;
#22484 = EDGE_LOOP ( 'NONE', ( #9658, #2687, #39104, #36002 ) ) ;
#22485 = CARTESIAN_POINT ( 'NONE',  ( -59.40286837855683899, 40.00000000000000711, 52.11376356989983805 ) ) ;
#22486 = FACE_OUTER_BOUND ( 'NONE', #22130, .T. ) ;
#22487 = AXIS2_PLACEMENT_3D ( 'NONE', #9205, #42356, #9641 ) ;
#22488 = EDGE_LOOP ( 'NONE', ( #28847, #4207, #3303, #14859 ) ) ;
#22489 = DIRECTION ( 'NONE',  ( 0.000000000000000000, 0.000000000000000000, 1.000000000000000000 ) ) ;
#22490 = ADVANCED_FACE ( 'NONE', ( #27672 ), #17657, .T. ) ;
#22491 = ORIENTED_EDGE ( 'NONE', *, *, #1469, .T. ) ;
#22492 = EDGE_CURVE ( 'NONE', #3503, #5699, #40684, .T. ) ;
#22493 = VERTEX_POINT ( 'NONE', #28955 ) ;
#22494 = CARTESIAN_POINT ( 'NONE',  ( -8.749793197483594298, -12.05525454449572464, 2.972870684497274762 ) ) ;
#22495 = ORIENTED_EDGE ( 'NONE', *, *, #41687, .T. ) ;
#22496 = CARTESIAN_POINT ( 'NONE',  ( 17.99999999999999645, 116.4607004671428570, 30.94182036827244531 ) ) ;
#22497 = DIRECTION ( 'NONE',  ( 0.000000000000000000, 0.6845471059286899473, -0.7289686274214103312 ) ) ;
#22498 = EDGE_CURVE ( 'NONE', #40092, #21299, #9367, .T. ) ;
#22499 = CARTESIAN_POINT ( 'NONE',  ( 0.000000000000000000, 0.000000000000000000, -4.484454397937119197 ) ) ;
#22500 = DIRECTION ( 'NONE',  ( -1.000000000000000000, -0.000000000000000000, -0.000000000000000000 ) ) ;
#22501 = ORIENTED_EDGE ( 'NONE', *, *, #3326, .F. ) ;
#22502 = DIRECTION ( 'NONE',  ( 1.000000000000000000, 0.000000000000000000, 0.000000000000000000 ) ) ;
#22503 = PRODUCT_DEFINITION_CONTEXT ( 'detailed design', #40910, 'design' ) ;
#22504 = VERTEX_POINT ( 'NONE', #15867 ) ;
#22505 = VECTOR ( 'NONE', #16444, 1000.000000000000000 ) ;
#22506 = CARTESIAN_POINT ( 'NONE',  ( 0.000000000000000000, -74.56001736500675747, 88.86396238369010803 ) ) ;
#22507 = ORIENTED_EDGE ( 'NONE', *, *, #40139, .T. ) ;
#22508 = DIRECTION ( 'NONE',  ( 0.000000000000000000, 0.000000000000000000, 1.000000000000000000 ) ) ;
#22509 = AXIS2_PLACEMENT_3D ( 'NONE', #17665, #23336, #10872 ) ;
#22510 = CARTESIAN_POINT ( 'NONE',  ( 4.197393957002303999, 7.772902908466098641E-14, -3.503767560748929810 ) ) ;
#22511 = EDGE_CURVE ( 'NONE', #23668, #9628, #21943, .T. ) ;
#22512 = ITEM_DEFINED_TRANSFORMATION ( 'NONE', 'NONE', #26770,  #13552 ) ;
#22513 = DIRECTION ( 'NONE',  ( 1.000000000000000000, 0.000000000000000000, 0.000000000000000000 ) ) ;
#22514 = CARTESIAN_POINT ( 'NONE',  ( 31.73387399974884104, 31.00000000000000355, -54.96645564127986461 ) ) ;
#22515 = ADVANCED_FACE ( 'NONE', ( #42643 ), #42221, .F. ) ;
#22516 = AXIS2_PLACEMENT_3D ( 'NONE', #24704, #18386, #24495 ) ;
#22517 = ORIENTED_EDGE ( 'NONE', *, *, #10143, .F. ) ;
#22518 = LINE ( 'NONE', #15958, #5255 ) ;
#22519 = EDGE_CURVE ( 'NONE', #23124, #16711, #23331, .T. ) ;
#22520 = ORIENTED_EDGE ( 'NONE', *, *, #29074, .F. ) ;
#22521 = CARTESIAN_POINT ( 'NONE',  ( 34.63398384099731686, 31.00000000000000355, -11.69655689657770203 ) ) ;
#22522 = CARTESIAN_POINT ( 'NONE',  ( -8.856203846296160975, 40.00000000000000000, 67.27320953167645712 ) ) ;
#22523 = DIRECTION ( 'NONE',  ( -1.000000000000000000, 0.000000000000000000, -0.000000000000000000 ) ) ;
#22524 = CARTESIAN_POINT ( 'NONE',  ( 18.00000000000000355, 22.43957647427161461, 41.27978878573636479 ) ) ;
#22525 = LINE ( 'NONE', #19672, #35072 ) ;
#22526 = DIRECTION ( 'NONE',  ( -1.000000000000000000, 0.000000000000000000, -0.000000000000000000 ) ) ;
#22527 = ADVANCED_FACE ( 'NONE', ( #6229, #15252 ), #32638, .T. ) ;
#22528 = AXIS2_PLACEMENT_3D ( 'NONE', #18778, #25729, #39187 ) ;
#22529 = EDGE_LOOP ( 'NONE', ( #16272, #12706 ) ) ;
#22530 = CARTESIAN_POINT ( 'NONE',  ( 23.39270017067629936, 40.00000000000000000, 40.49502024156475244 ) ) ;
#22531 = DIRECTION ( 'NONE',  ( 0.000000000000000000, 0.2486898871648552389, -0.9685831611286309650 ) ) ;
#22532 = LINE ( 'NONE', #2614, #43052 ) ;
#22533 = ORIENTED_EDGE ( 'NONE', *, *, #22262, .T. ) ;
#22534 = DIRECTION ( 'NONE',  ( 0.000000000000000000, -7.709882115452471264E-16, -1.000000000000000000 ) ) ;
#22535 = DIRECTION ( 'NONE',  ( 0.000000000000000000, 0.000000000000000000, 1.000000000000000000 ) ) ;
#22536 = AXIS2_PLACEMENT_3D ( 'NONE', #2296, #19584, #36328 ) ;
#22537 = ORIENTED_EDGE ( 'NONE', *, *, #9519, .T. ) ;
#22538 = DIRECTION ( 'NONE',  ( -1.000000000000000000, 0.000000000000000000, 0.000000000000000000 ) ) ;
#22539 = VERTEX_POINT ( 'NONE', #25903 ) ;
#22540 = EDGE_CURVE ( 'NONE', #31991, #13177, #977, .T. ) ;
#22541 = VECTOR ( 'NONE', #33364, 1000.000000000000000 ) ;
#22542 = ORIENTED_EDGE ( 'NONE', *, *, #26374, .F. ) ;
#22543 = CYLINDRICAL_SURFACE ( 'NONE', #5562, 116.0000000000000000 ) ;
#22544 = CARTESIAN_POINT ( 'NONE',  ( 82.09539989324809994, 31.00000000000000000, -27.75477508811727390 ) ) ;
#22545 = EDGE_LOOP ( 'NONE', ( #32035, #18104, #39901, #36671 ) ) ;
#22546 = CARTESIAN_POINT ( 'NONE',  ( -4.203934362469166963, -1.640673743454851286, -3.598432614606932756 ) ) ;
#22547 = CARTESIAN_POINT ( 'NONE',  ( -2.649999999999993694, 150.5000000000000284, 9.999999999999998224 ) ) ;
#22548 = CARTESIAN_POINT ( 'NONE',  ( 17.99999999999999645, 0.000000000000000000, 0.000000000000000000 ) ) ;
#22549 = ORIENTED_EDGE ( 'NONE', *, *, #226, .T. ) ;
#22550 = DIRECTION ( 'NONE',  ( -1.000000000000000000, 0.000000000000000000, 0.000000000000000000 ) ) ;
#22551 = CARTESIAN_POINT ( 'NONE',  ( -87.85203729262056527, 40.00000000000000711, 50.59313708112332364 ) ) ;
#22552 = CARTESIAN_POINT ( 'NONE',  ( 17.99999999999999645, -35.78425302087536153, -3.935382540233173465 ) ) ;
#22554 = DIRECTION ( 'NONE',  ( 0.000000000000000000, 0.6783118362696172188, -0.7347741508630661889 ) ) ;
#22553 = DIRECTION ( 'NONE',  ( 0.000000000000000000, 0.000000000000000000, 1.000000000000000000 ) ) ;
#22555 = FACE_OUTER_BOUND ( 'NONE', #12780, .T. ) ;
#22556 = ORIENTED_EDGE ( 'NONE', *, *, #2775, .F. ) ;
#22557 = VECTOR ( 'NONE', #13260, 1000.000000000000000 ) ;
#22558 = CARTESIAN_POINT ( 'NONE',  ( -24.68525358734468611, 31.00000000000000355, -18.92943107747915832 ) ) ;
#22559 = EDGE_CURVE ( 'NONE', #10188, #12185, #28893, .T. ) ;
#22560 = ORIENTED_EDGE ( 'NONE', *, *, #23258, .F. ) ;
#22561 = DIRECTION ( 'NONE',  ( -3.996523416598930318E-16, 2.658563593772947863E-15, 1.000000000000000000 ) ) ;
#22562 = EDGE_CURVE ( 'NONE', #37276, #7995, #13575, .T. ) ;
#22563 = CARTESIAN_POINT ( 'NONE',  ( 18.00000000000000355, 0.000000000000000000, 15.00000000000000000 ) ) ;
#22564 = ORIENTED_EDGE ( 'NONE', *, *, #3083, .T. ) ;
#22565 = CARTESIAN_POINT ( 'NONE',  ( 39.78947517253659072, 40.00000000000000000, -19.62497191778171413 ) ) ;
#22566 = CARTESIAN_POINT ( 'NONE',  ( 36.89914868738106435, 40.00000000000000000, -2.354335741662294978 ) ) ;
#22567 = AXIS2_PLACEMENT_3D ( 'NONE', #6898, #16317, #29620 ) ;
#22568 = ORIENTED_EDGE ( 'NONE', *, *, #2638, .F. ) ;
#22569 = ORIENTED_EDGE ( 'NONE', *, *, #2844, .F. ) ;
#22570 = FILL_AREA_STYLE ('',( #15796 ) ) ;
#22571 = CARTESIAN_POINT ( 'NONE',  ( 17.99999999999999645, -111.2559044912522950, -32.83479428644788811 ) ) ;
#22572 = CARTESIAN_POINT ( 'NONE',  ( 18.00000000000000355, -27.79676263918163315, -37.88001506494799031 ) ) ;
#22573 = EDGE_CURVE ( 'NONE', #3181, #29181, #11516, .T. ) ;
#22574 = DIRECTION ( 'NONE',  ( -1.000000000000000000, 0.000000000000000000, 0.000000000000000000 ) ) ;
#22575 = AXIS2_PLACEMENT_3D ( 'NONE', #1076, #855, #10935 ) ;
#22576 = CARTESIAN_POINT ( 'NONE',  ( 9.000000000000000000, -32.49609705003694415, -15.49205204337308217 ) ) ;
#22577 = EDGE_CURVE ( 'NONE', #33525, #16679, #18527, .T. ) ;
#22578 = CARTESIAN_POINT ( 'NONE',  ( 0.000000000000000000, 84.09610293794069946, 74.27057253243037849 ) ) ;
#22579 = ORIENTED_EDGE ( 'NONE', *, *, #17101, .T. ) ;
#22580 = CARTESIAN_POINT ( 'NONE',  ( 18.00000000000000355, -46.21320724403641833, -10.97699764142002188 ) ) ;
#22581 = ORIENTED_EDGE ( 'NONE', *, *, #4307, .T. ) ;
#22582 = CARTESIAN_POINT ( 'NONE',  ( 106.4195705685756792, -106.4195705685758213, 6.999999999999667821 ) ) ;
#22583 = FACE_OUTER_BOUND ( 'NONE', #21522, .T. ) ;
#22584 = AXIS2_PLACEMENT_3D ( 'NONE', #35407, #5723, #28672 ) ;
#22585 = DIRECTION ( 'NONE',  ( 0.000000000000000000, 0.000000000000000000, 1.000000000000000000 ) ) ;
#22586 = AXIS2_PLACEMENT_3D ( 'NONE', #37544, #33027, #17520 ) ;
#22587 = FACE_OUTER_BOUND ( 'NONE', #35341, .T. ) ;
#22588 = ORIENTED_EDGE ( 'NONE', *, *, #42000, .F. ) ;
#22589 = CARTESIAN_POINT ( 'NONE',  ( 48.45023387855729879, 40.00000000000000000, 83.88660019351674180 ) ) ;
#22590 = ORIENTED_EDGE ( 'NONE', *, *, #41748, .F. ) ;
#22591 = DIRECTION ( 'NONE',  ( 1.000000000000000000, 0.000000000000000000, 0.000000000000000000 ) ) ;
#22592 = EDGE_CURVE ( 'NONE', #23588, #23398, #20590, .T. ) ;
#22593 = AXIS2_PLACEMENT_3D ( 'NONE', #6526, #23371, #3244 ) ;
#22594 = EDGE_LOOP ( 'NONE', ( #8585, #9059, #1577, #4613 ) ) ;
#22596 = ORIENTED_EDGE ( 'NONE', *, *, #38011, .F. ) ;
#22595 = DIRECTION ( 'NONE',  ( 3.996523416598930318E-16, -2.658563593772947863E-15, -1.000000000000000000 ) ) ;
#22597 = CARTESIAN_POINT ( 'NONE',  ( -22.33566874673848091, 31.00000000000000355, 45.10700316349001326 ) ) ;
#22598 = ADVANCED_FACE ( 'NONE', ( #28543 ), #2505, .F. ) ;
#22599 = ORIENTED_EDGE ( 'NONE', *, *, #23210, .T. ) ;
#22600 = DIRECTION ( 'NONE',  ( -1.000000000000000000, -0.000000000000000000, -0.000000000000000000 ) ) ;
#22601 = COLOUR_RGB ( '', 0.31764706, 0.68627451, 0.89019608) ;
#22602 = CYLINDRICAL_SURFACE ( 'NONE', #23099, 19.99999999999999645 ) ;
#22603 = VERTEX_POINT ( 'NONE', #9076 ) ;
#22605 = CARTESIAN_POINT ( 'NONE',  ( -65.32047834219908111, 40.00000000000000711, -32.32491738442255524 ) ) ;
#22604 = VECTOR ( 'NONE', #14780, 1000.000000000000000 ) ;
#22607 = DIRECTION ( 'NONE',  ( -1.000000000000000000, 0.000000000000000000, 0.000000000000000000 ) ) ;
#22606 = DIRECTION ( 'NONE',  ( 0.000000000000000000, 0.000000000000000000, -1.000000000000000000 ) ) ;
#22608 = DIRECTION ( 'NONE',  ( -1.000000000000000000, 0.000000000000000000, 0.000000000000000000 ) ) ;
#22609 = EDGE_LOOP ( 'NONE', ( #38916, #21232, #25168, #37530 ) ) ;
#22610 = DIRECTION ( 'NONE',  ( 0.000000000000000000, -0.5877852522924624790, -0.8090169943749551118 ) ) ;
#22611 = VECTOR ( 'NONE', #23441, 1000.000000000000000 ) ;
#22612 = ORIENTED_EDGE ( 'NONE', *, *, #16506, .F. ) ;
#22613 = CARTESIAN_POINT ( 'NONE',  ( 18.00000000000000355, 17.50309955389674954, -43.60271849949345579 ) ) ;
#22614 = VECTOR ( 'NONE', #11027, 1000.000000000000000 ) ;
#22615 = CYLINDRICAL_SURFACE ( 'NONE', #35835, 120.5010000000000190 ) ;
#22616 = ADVANCED_FACE ( 'NONE', ( #32208 ), #16080, .T. ) ;
#22617 = CARTESIAN_POINT ( 'NONE',  ( -51.96644965834242669, 31.00000000000000711, 59.25555446696338890 ) ) ;
#22618 = EDGE_CURVE ( 'NONE', #23414, #39824, #30999, .T. ) ;
#22620 = DIRECTION ( 'NONE',  ( 0.000000000000000000, -0.1837495178165777232, 0.9829730996839003421 ) ) ;
#22619 = DIRECTION ( 'NONE',  ( -1.000000000000000000, 0.000000000000000000, 0.000000000000000000 ) ) ;
#22621 = ORIENTED_EDGE ( 'NONE', *, *, #33981, .F. ) ;
#22622 = EDGE_CURVE ( 'NONE', #12218, #7715, #5384, .T. ) ;
#22623 = EDGE_CURVE ( 'NONE', #39574, #41473, #25274, .T. ) ;
#22624 = CARTESIAN_POINT ( 'NONE',  ( 17.99999999999999645, 0.000000000000000000, 0.000000000000000000 ) ) ;
#22625 = AXIS2_PLACEMENT_3D ( 'NONE', #38795, #22482, #28795 ) ;
#22626 = ORIENTED_EDGE ( 'NONE', *, *, #13717, .F. ) ;
#22627 = CARTESIAN_POINT ( 'NONE',  ( 18.00000000000000355, -49.25004636492399612, 16.68630974939742018 ) ) ;
#22628 = LINE ( 'NONE', #36097, #27638 ) ;
#22629 = CARTESIAN_POINT ( 'NONE',  ( -13.16936484334534008, 31.00000000000000355, 99.04657264463375554 ) ) ;
#22630 = CARTESIAN_POINT ( 'NONE',  ( 43.66223835209735427, 40.00000000000000000, 88.82794485019093145 ) ) ;
#22631 = FACE_OUTER_BOUND ( 'NONE', #19210, .T. ) ;
#22632 = AXIS2_PLACEMENT_3D ( 'NONE', #18829, #5467, #25148 ) ;
#22633 = VERTEX_POINT ( 'NONE', #42008 ) ;
#22634 = DIRECTION ( 'NONE',  ( -1.000000000000000000, -0.000000000000000000, 0.000000000000000000 ) ) ;
#22635 = ORIENTED_EDGE ( 'NONE', *, *, #9342, .T. ) ;
#22636 = LINE ( 'NONE', #6012, #3269 ) ;
#22637 = CARTESIAN_POINT ( 'NONE',  ( 18.00000000000000355, 11.46872990052444408, -45.56340405422433548 ) ) ;
#22638 = CARTESIAN_POINT ( 'NONE',  ( -15.99999999999997691, 31.00000000000000355, 5.571627607371296764E-15 ) ) ;
#22639 = ORIENTED_EDGE ( 'NONE', *, *, #37999, .T. ) ;
#22640 = CARTESIAN_POINT ( 'NONE',  ( 18.00000000000000355, -42.03146605346771025, -22.12489237027361000 ) ) ;
#22641 = CARTESIAN_POINT ( 'NONE',  ( 6.600000000000012079, -19.59999999999998721, 2.400307726328811507E-15 ) ) ;
#22642 = CIRCLE ( 'NONE', #42081, 13.59999999999999787 ) ;
#22643 = EDGE_CURVE ( 'NONE', #8344, #29115, #19197, .T. ) ;
#22644 = CARTESIAN_POINT ( 'NONE',  ( -1.600000000000000089, -12.75000000000000000, -1.199999999999999956 ) ) ;
#22645 = AXIS2_PLACEMENT_3D ( 'NONE', #4546, #7834, #29744 ) ;
#22646 = ORIENTED_EDGE ( 'NONE', *, *, #35990, .T. ) ;
#22647 = CARTESIAN_POINT ( 'NONE',  ( 6.473670811831355287, 31.00000000000000355, -24.11571013580713441 ) ) ;
#22648 = ADVANCED_FACE ( 'NONE', ( #26325 ), #33697, .F. ) ;
#22649 = DIRECTION ( 'NONE',  ( -1.000000000000000000, -0.000000000000000000, -0.000000000000000000 ) ) ;
#22650 = CIRCLE ( 'NONE', #2368, 18.77999999999999403 ) ;
#22652 = EDGE_LOOP ( 'NONE', ( #33480, #15556 ) ) ;
#22651 = CARTESIAN_POINT ( 'NONE',  ( 18.00000000000000355, -39.78933988720098114, -24.98727647985043276 ) ) ;
#22653 = CIRCLE ( 'NONE', #34440, 47.49900000000000233 ) ;
#22654 = VERTEX_POINT ( 'NONE', #9724 ) ;
#22655 = FACE_OUTER_BOUND ( 'NONE', #21674, .T. ) ;
#22656 = CARTESIAN_POINT ( 'NONE',  ( 17.99999999999999645, 0.000000000000000000, 0.000000000000000000 ) ) ;
#22657 = CARTESIAN_POINT ( 'NONE',  ( -42.09738266246711902, 40.00000000000000000, -2.828681863544772135 ) ) ;
#22658 = DIRECTION ( 'NONE',  ( -1.000000000000000000, 0.000000000000000000, 0.000000000000000000 ) ) ;
#22659 = CARTESIAN_POINT ( 'NONE',  ( -4.211140560182196957, 2.431303136016537803, -3.745885042887433514 ) ) ;
#22660 = CARTESIAN_POINT ( 'NONE',  ( -6.259644161404860030E-16, -4.618802153517027165, -3.433295621305388234 ) ) ;
#22661 = VERTEX_POINT ( 'NONE', #20434 ) ;
#22662 = CARTESIAN_POINT ( 'NONE',  ( 17.99999999999999645, 117.6086855750638165, -26.24286718911983485 ) ) ;
#22663 = CIRCLE ( 'NONE', #7982, 120.5010000000000332 ) ;
#22664 = ORIENTED_EDGE ( 'NONE', *, *, #401, .F. ) ;
#22665 = DIRECTION ( 'NONE',  ( 0.000000000000000000, 0.000000000000000000, 1.000000000000000000 ) ) ;
#22666 = CARTESIAN_POINT ( 'NONE',  ( -4.000000000000000888, -2.309401076758512694, -3.504269196027526512 ) ) ;
#22667 = CARTESIAN_POINT ( 'NONE',  ( 34.94781834021004840, 31.00000000000000355, -26.81980329959834108 ) ) ;
#22668 = EDGE_LOOP ( 'NONE', ( #39174, #9416, #23055, #36945 ) ) ;
#22669 = EDGE_CURVE ( 'NONE', #11369, #20569, #30319, .T. ) ;
#22670 = EDGE_CURVE ( 'NONE', #5275, #24485, #36971, .T. ) ;
#22671 = AXIS2_PLACEMENT_3D ( 'NONE', #20031, #43098, #26340 ) ;
#22672 = EDGE_CURVE ( 'NONE', #16283, #26598, #13233, .T. ) ;
#22673 = DIRECTION ( 'NONE',  ( -3.009274222672345096E-17, -1.000000000000000000, 2.455023325076454960E-18 ) ) ;
#22674 = CARTESIAN_POINT ( 'NONE',  ( -54.00384411200708712, 31.00000000000000711, 70.40394205939183792 ) ) ;
#22675 = CIRCLE ( 'NONE', #7299, 31.49899999999999878 ) ;
#22676 = LINE ( 'NONE', #12419, #31051 ) ;
#22677 = ORIENTED_EDGE ( 'NONE', *, *, #14321, .T. ) ;
#22678 = CARTESIAN_POINT ( 'NONE',  ( 32.82854187708761629, 31.00000000000000355, -56.64543409046200395 ) ) ;
#22680 = CIRCLE ( 'NONE', #8688, 20.00000000000000000 ) ;
#22679 = CARTESIAN_POINT ( 'NONE',  ( 8.570044366896553356, 40.00000000000000000, -64.27561742002654910 ) ) ;
#22681 = CARTESIAN_POINT ( 'NONE',  ( 0.000000000000000000, 22.66088087769211157, -21.87856208362532939 ) ) ;
#22682 = VECTOR ( 'NONE', #33050, 1000.000000000000000 ) ;
#22683 = ORIENTED_EDGE ( 'NONE', *, *, #39954, .F. ) ;
#22684 = LINE ( 'NONE', #13072, #21392 ) ;
#22685 = EDGE_CURVE ( 'NONE', #2260, #28849, #10823, .T. ) ;
#22686 = DIRECTION ( 'NONE',  ( -1.000000000000000000, -0.000000000000000000, -0.000000000000000000 ) ) ;
#22687 = PLANE ( 'NONE',  #16392 ) ;
#22689 = ORIENTED_EDGE ( 'NONE', *, *, #5477, .F. ) ;
#22688 = DIRECTION ( 'NONE',  ( 0.000000000000000000, 0.000000000000000000, 1.000000000000000000 ) ) ;
#22690 = CARTESIAN_POINT ( 'NONE',  ( 17.99999999999999645, 0.000000000000000000, 0.000000000000000000 ) ) ;
#22691 = CARTESIAN_POINT ( 'NONE',  ( 17.99999999999999645, -15.21076497709792008, 119.5371223922154797 ) ) ;
#22692 = EDGE_LOOP ( 'NONE', ( #9559, #39968, #2764, #18990 ) ) ;
#22693 = CARTESIAN_POINT ( 'NONE',  ( 71.66629920589342362, 39.99999999999999289, 24.32769631419027689 ) ) ;
#22694 = CARTESIAN_POINT ( 'NONE',  ( 0.000000000000000000, 23.79363200506953291, 27.01597816121656237 ) ) ;
#22695 = VECTOR ( 'NONE', #30597, 1000.000000000000000 ) ;
#22696 = VERTEX_POINT ( 'NONE', #20225 ) ;
#22697 = CARTESIAN_POINT ( 'NONE',  ( 0.000000000000000000, 0.000000000000000000, 0.000000000000000000 ) ) ;
#22698 = CYLINDRICAL_SURFACE ( 'NONE', #40539, 51.99999999999999289 ) ;
#22699 = CIRCLE ( 'NONE', #24794, 120.5010000000000332 ) ;
#22700 = ORIENTED_EDGE ( 'NONE', *, *, #26147, .T. ) ;
#22701 = CIRCLE ( 'NONE', #14337, 59.00000000000000711 ) ;
#22702 = EDGE_CURVE ( 'NONE', #21663, #14485, #29815, .T. ) ;
#22703 = CIRCLE ( 'NONE', #12893, 36.00000000000000000 ) ;
#22704 = VECTOR ( 'NONE', #16116, 1000.000000000000000 ) ;
#22705 = VERTEX_POINT ( 'NONE', #23275 ) ;
#22706 = FACE_OUTER_BOUND ( 'NONE', #33370, .T. ) ;
#22707 = VERTEX_POINT ( 'NONE', #2924 ) ;
#22708 = AXIS2_PLACEMENT_3D ( 'NONE', #41413, #21634, #31614 ) ;
#22709 = CARTESIAN_POINT ( 'NONE',  ( 18.00000000000000355, 0.000000000000000000, 0.000000000000000000 ) ) ;
#22710 = CARTESIAN_POINT ( 'NONE',  ( 130.0000000000000284, 1.638195277402996435E-14, 367.6955262170047263 ) ) ;
#22711 = LINE ( 'NONE', #29237, #36503 ) ;
#22712 = CARTESIAN_POINT ( 'NONE',  ( 0.000000000000000000, 0.000000000000000000, 0.000000000000000000 ) ) ;
#22713 = EDGE_LOOP ( 'NONE', ( #22310, #1292 ) ) ;
#22714 = LINE ( 'NONE', #42714, #29377 ) ;
#22716 = ORIENTED_EDGE ( 'NONE', *, *, #17777, .T. ) ;
#22715 = CIRCLE ( 'NONE', #12235, 58.99999999999998579 ) ;
#22717 = DIRECTION ( 'NONE',  ( 0.000000000000000000, 0.000000000000000000, 1.000000000000000000 ) ) ;
#22718 = VERTEX_POINT ( 'NONE', #16945 ) ;
#22719 = CARTESIAN_POINT ( 'NONE',  ( 65.39325745242679488, -12.05525454449572464, 58.58409293616905700 ) ) ;
#22720 = EDGE_CURVE ( 'NONE', #3516, #21806, #8006, .T. ) ;
#22721 = CARTESIAN_POINT ( 'NONE',  ( 0.000000000000000000, 0.000000000000000000, 0.000000000000000000 ) ) ;
#22722 = PRODUCT_CONTEXT ( 'NONE', #26721, 'mechanical' ) ;
#22723 = DIRECTION ( 'NONE',  ( 0.000000000000000000, -0.000000000000000000, 1.000000000000000000 ) ) ;
#22724 = CARTESIAN_POINT ( 'NONE',  ( -59.89583333444493718, 31.00000000000000711, 3.926990808566372060 ) ) ;
#22725 = DIRECTION ( 'NONE',  ( 1.000000000000000000, 0.000000000000000000, 0.000000000000000000 ) ) ;
#22726 = ORIENTED_EDGE ( 'NONE', *, *, #37157, .F. ) ;
#22727 = CARTESIAN_POINT ( 'NONE',  ( 36.56095242095437925, 31.00000000000000355, -4.755136101395175174 ) ) ;
#22728 = AXIS2_PLACEMENT_3D ( 'NONE', #42094, #12246, #25575 ) ;
#22729 = CARTESIAN_POINT ( 'NONE',  ( 62.17703816010947548, 39.99999999999999289, 21.10553973064489597 ) ) ;
#22730 = EDGE_CURVE ( 'NONE', #5856, #14037, #32393, .T. ) ;
#22731 = AXIS2_PLACEMENT_3D ( 'NONE', #20631, #17577, #24342 ) ;
#22732 = DIRECTION ( 'NONE',  ( 1.000000000000000000, 0.000000000000000000, 0.000000000000000000 ) ) ;
#22733 = ADVANCED_FACE ( 'NONE', ( #23493 ), #27179, .T. ) ;
#22734 = CYLINDRICAL_SURFACE ( 'NONE', #34687, 59.00000000000000000 ) ;
#22735 = EDGE_CURVE ( 'NONE', #25826, #1540, #24076, .T. ) ;
#22736 = DIRECTION ( 'NONE',  ( 0.000000000000000000, 0.000000000000000000, 1.000000000000000000 ) ) ;
#22737 = CARTESIAN_POINT ( 'NONE',  ( 0.000000000000000000, -36.05989434073592292, -30.12041790338656710 ) ) ;
#22738 = CIRCLE ( 'NONE', #28318, 116.0000000000000000 ) ;
#22739 = ORIENTED_EDGE ( 'NONE', *, *, #16943, .T. ) ;
#22740 = CARTESIAN_POINT ( 'NONE',  ( 44.89583333484414140, 40.00000000000000000, -2.945243104263157274 ) ) ;
#22741 = LINE ( 'NONE', #1774, #14627 ) ;
#22742 = DIRECTION ( 'NONE',  ( 0.000000000000000000, 0.000000000000000000, 1.000000000000000000 ) ) ;
#22743 = ORIENTED_EDGE ( 'NONE', *, *, #14195, .T. ) ;
#22744 = LINE ( 'NONE', #32738, #36339 ) ;
#22745 = FACE_OUTER_BOUND ( 'NONE', #12317, .T. ) ;
#22746 = EDGE_LOOP ( 'NONE', ( #39217, #32736, #41243, #27231 ) ) ;
#22747 = DIRECTION ( 'NONE',  ( 1.000000000000000000, 0.000000000000000000, 0.000000000000000000 ) ) ;
#22748 = ORIENTED_EDGE ( 'NONE', *, *, #963, .F. ) ;
#22749 = EDGE_CURVE ( 'NONE', #34617, #39340, #7082, .T. ) ;
#22750 = ORIENTED_EDGE ( 'NONE', *, *, #32769, .T. ) ;
#22751 = DIRECTION ( 'NONE',  ( 1.000000000000000000, 0.000000000000000000, 0.000000000000000000 ) ) ;
#22752 = CARTESIAN_POINT ( 'NONE',  ( 83.51212062385671686, 31.00000000000000000, -48.08891344041042970 ) ) ;
#22753 = ORIENTED_EDGE ( 'NONE', *, *, #24247, .T. ) ;
#22754 = DIRECTION ( 'NONE',  ( -1.000000000000000000, -0.000000000000000000, -0.000000000000000000 ) ) ;
#22755 = AXIS2_PLACEMENT_3D ( 'NONE', #16607, #3656, #33362 ) ;
#22756 = DIRECTION ( 'NONE',  ( 0.000000000000000000, 0.000000000000000000, 1.000000000000000000 ) ) ;
#22757 = VECTOR ( 'NONE', #36839, 1000.000000000000000 ) ;
#22759 = DIRECTION ( 'NONE',  ( 1.000000000000000000, 0.000000000000000000, 0.000000000000000000 ) ) ;
#22758 = AXIS2_PLACEMENT_3D ( 'NONE', #16814, #23144, #20094 ) ;
#22760 = ORIENTED_EDGE ( 'NONE', *, *, #34824, .T. ) ;
#22761 = VECTOR ( 'NONE', #9494, 1000.000000000000000 ) ;
#22762 = CARTESIAN_POINT ( 'NONE',  ( 18.00000000000000355, 0.000000000000000000, 0.000000000000000000 ) ) ;
#22763 = CARTESIAN_POINT ( 'NONE',  ( 0.000000000000000000, -30.01658535635337444, 108.1077105353196970 ) ) ;
#22764 = CIRCLE ( 'NONE', #3888, 20.00000000000000711 ) ;
#22765 = DIRECTION ( 'NONE',  ( 0.000000000000000000, 0.3641605752528229711, -0.9313361774523382097 ) ) ;
#22767 = DIRECTION ( 'NONE',  ( 0.000000000000000000, 0.000000000000000000, 1.000000000000000000 ) ) ;
#22766 = CARTESIAN_POINT ( 'NONE',  ( 0.000000000000000000, 115.5737863835463628, -9.934782381632540904 ) ) ;
#22768 = CIRCLE ( 'NONE', #19974, 13.59999999999999964 ) ;
#22769 = AXIS2_PLACEMENT_3D ( 'NONE', #14661, #7864, #11372 ) ;
#22770 = FACE_OUTER_BOUND ( 'NONE', #21436, .T. ) ;
#22771 = EDGE_CURVE ( 'NONE', #9051, #18562, #27520, .T. ) ;
#22772 = ORIENTED_EDGE ( 'NONE', *, *, #21188, .T. ) ;
#22773 = PRESENTATION_STYLE_ASSIGNMENT (( #26449 ) ) ;
#22774 = AXIS2_PLACEMENT_3D ( 'NONE', #28331, #4509, #24636 ) ;
#22775 = CARTESIAN_POINT ( 'NONE',  ( 26.99674208481366833, 31.00000000000000355, -20.71990538090019029 ) ) ;
#22776 = ORIENTED_EDGE ( 'NONE', *, *, #14431, .F. ) ;
#22777 = DIRECTION ( 'NONE',  ( 0.000000000000000000, -0.9826841245925190815, -0.1852887240871243513 ) ) ;
#22778 = DIRECTION ( 'NONE',  ( 0.000000000000000000, 0.000000000000000000, 1.000000000000000000 ) ) ;
#22779 = EDGE_LOOP ( 'NONE', ( #34377, #26482, #20279, #5097 ) ) ;
#22780 = AXIS2_PLACEMENT_3D ( 'NONE', #26083, #39573, #16058 ) ;
#22781 = DIRECTION ( 'NONE',  ( -1.000000000000000000, -0.000000000000000000, -0.000000000000000000 ) ) ;
#22782 = CARTESIAN_POINT ( 'NONE',  ( -19.20510714644778361, 40.00000000000000000, 33.27066566623395261 ) ) ;
#22783 = CARTESIAN_POINT ( 'NONE',  ( 5.076274692535532651, 40.00000000000000000, 39.04542013319162663 ) ) ;
#22784 = EDGE_CURVE ( 'NONE', #17146, #39595, #42864, .T. ) ;
#22785 = VERTEX_POINT ( 'NONE', #23916 ) ;
#22786 = VERTEX_POINT ( 'NONE', #40235 ) ;
#22787 = CARTESIAN_POINT ( 'NONE',  ( 17.99999999999999645, 7.220349212960452512, 35.26849241522666745 ) ) ;
#22788 = EDGE_CURVE ( 'NONE', #40762, #16567, #39594, .T. ) ;
#22789 = DIRECTION ( 'NONE',  ( 0.000000000000000000, 1.000000000000000000, 0.000000000000000000 ) ) ;
#22790 = VECTOR ( 'NONE', #16285, 1000.000000000000000 ) ;
#22791 = CARTESIAN_POINT ( 'NONE',  ( -3.679171394226034675, -2.494631558665844739, -0.3503314178412558211 ) ) ;
#22792 = CIRCLE ( 'NONE', #11631, 120.5010000000000190 ) ;
#22793 = CIRCLE ( 'NONE', #39459, 116.0000000000000000 ) ;
#22794 = CARTESIAN_POINT ( 'NONE',  ( 106.4195705685734623, 106.4195705685780524, 10.00000000000025224 ) ) ;
#22795 = CIRCLE ( 'NONE', #11634, 116.0000000000000000 ) ;
#22796 = DIRECTION ( 'NONE',  ( 0.000000000000000000, 0.05322217484217877520, -0.9985826956767620555 ) ) ;
#22797 = EDGE_LOOP ( 'NONE', ( #12649, #6287, #32, #8645 ) ) ;
#22798 = DIRECTION ( 'NONE',  ( -3.996523416598930318E-16, 2.658563593772947863E-15, 1.000000000000000000 ) ) ;
#22799 = EDGE_LOOP ( 'NONE', ( #41984, #34612, #22151, #40779 ) ) ;
#22800 = CYLINDRICAL_SURFACE ( 'NONE', #24329, 120.5010000000000190 ) ;
#22801 = CARTESIAN_POINT ( 'NONE',  ( 106.4195705685734623, 106.4195705685780524, 10.00000000000025224 ) ) ;
#22802 = CIRCLE ( 'NONE', #10205, 31.49899999999999878 ) ;
#22803 = AXIS2_PLACEMENT_3D ( 'NONE', #27436, #20707, #17216 ) ;
#22804 = DIRECTION ( 'NONE',  ( -1.000000000000000000, 0.000000000000000000, -0.000000000000000000 ) ) ;
#22805 = CARTESIAN_POINT ( 'NONE',  ( 8.919999999999994600, 0.000000000000000000, 0.000000000000000000 ) ) ;
#22806 = VERTEX_POINT ( 'NONE', #19574 ) ;
#22807 = DIRECTION ( 'NONE',  ( -1.000000000000000000, 0.000000000000000000, 0.000000000000000000 ) ) ;
#22808 = ORIENTED_EDGE ( 'NONE', *, *, #23628, .F. ) ;
#22809 = DIRECTION ( 'NONE',  ( 1.000000000000000000, 0.000000000000000000, 0.000000000000000000 ) ) ;
#22810 = AXIS2_PLACEMENT_3D ( 'NONE', #29663, #12865, #23565 ) ;
#22811 = EDGE_CURVE ( 'NONE', #41456, #38270, #8690, .T. ) ;
#22812 = VERTEX_POINT ( 'NONE', #23072 ) ;
#22814 = ORIENTED_EDGE ( 'NONE', *, *, #18885, .T. ) ;
#22813 = CYLINDRICAL_SURFACE ( 'NONE', #24381, 120.5010000000000190 ) ;
#22815 = CIRCLE ( 'NONE', #18664, 116.0000000000000000 ) ;
#22816 = CARTESIAN_POINT ( 'NONE',  ( 56.89991739620084132, 31.00000000000000355, -3.630084216720528278 ) ) ;
#22818 = EDGE_CURVE ( 'NONE', #18138, #37185, #6436, .T. ) ;
#22817 = VERTEX_POINT ( 'NONE', #36318 ) ;
#22819 = CARTESIAN_POINT ( 'NONE',  ( 17.99999999999999645, 0.000000000000000000, 0.000000000000000000 ) ) ;
#22820 = ORIENTED_EDGE ( 'NONE', *, *, #21059, .T. ) ;
#22821 = CARTESIAN_POINT ( 'NONE',  ( 18.00000000000000355, 43.55304910509445904, -28.41006711799937889 ) ) ;
#22822 = PRODUCT_DEFINITION_SHAPE ( 'NONE', 'NONE',  #43193 ) ;
#22823 = ORIENTED_EDGE ( 'NONE', *, *, #3683, .T. ) ;
#22824 = CARTESIAN_POINT ( 'NONE',  ( -71.33925323115938966, 40.00000000000000711, 9.290813765102964084 ) ) ;
#22825 = AXIS2_PLACEMENT_3D ( 'NONE', #23492, #23707, #37401 ) ;
#22827 = CARTESIAN_POINT ( 'NONE',  ( 17.99999999999999645, 59.07817985939002625, 105.0250430397510968 ) ) ;
#22826 = DIRECTION ( 'NONE',  ( 1.000000000000000000, 0.000000000000000000, 0.000000000000000000 ) ) ;
#22828 = DIRECTION ( 'NONE',  ( 0.000000000000000000, 0.000000000000000000, 1.000000000000000000 ) ) ;
#22829 = ORIENTED_EDGE ( 'NONE', *, *, #6008, .T. ) ;
#22830 = DIRECTION ( 'NONE',  ( 1.000000000000000000, 0.000000000000000000, 0.000000000000000000 ) ) ;
#22831 = CIRCLE ( 'NONE', #14438, 1.399999999999998579 ) ;
#22832 = EDGE_CURVE ( 'NONE', #10211, #17650, #35190, .T. ) ;
#22833 = ORIENTED_EDGE ( 'NONE', *, *, #23993, .F. ) ;
#22834 = CIRCLE ( 'NONE', #3949, 13.59999999999999964 ) ;
#22835 = VECTOR ( 'NONE', #20585, 1000.000000000000000 ) ;
#22836 = CARTESIAN_POINT ( 'NONE',  ( 0.000000000000000000, 111.1352304691227744, 15.40237066878635730 ) ) ;
#22837 = CYLINDRICAL_SURFACE ( 'NONE', #31006, 51.99999999999999289 ) ;
#22838 = VECTOR ( 'NONE', #27842, 1000.000000000000000 ) ;
#22839 = CARTESIAN_POINT ( 'NONE',  ( 10.12401712103624263, 31.00000000000000355, 76.79210772277129138 ) ) ;
#22841 = CARTESIAN_POINT ( 'NONE',  ( 0.000000000000000000, 0.000000000000000000, 0.000000000000000000 ) ) ;
#22840 = DIRECTION ( 'NONE',  ( 0.000000000000000000, 0.000000000000000000, 1.000000000000000000 ) ) ;
#22843 = VERTEX_POINT ( 'NONE', #18260 ) ;
#22842 = CIRCLE ( 'NONE', #37424, 31.49899999999999878 ) ;
#22845 = CIRCLE ( 'NONE', #3966, 100.0000000000000000 ) ;
#22844 = CYLINDRICAL_SURFACE ( 'NONE', #5932, 51.99999999999999289 ) ;
#22846 = EDGE_CURVE ( 'NONE', #25771, #40772, #14099, .T. ) ;
#22847 = CIRCLE ( 'NONE', #6075, 20.00000000000000711 ) ;
#22848 = ORIENTED_EDGE ( 'NONE', *, *, #3376, .T. ) ;
#22849 = DIRECTION ( 'NONE',  ( 0.000000000000000000, 0.5877852522924685852, 0.8090169943749506709 ) ) ;
#22850 = EDGE_CURVE ( 'NONE', #24053, #10364, #33067, .T. ) ;
#22851 = LINE ( 'NONE', #39150, #41565 ) ;
#22852 = CARTESIAN_POINT ( 'NONE',  ( 77.87745995352098305, 31.00000000000000000, 59.89653754214596404 ) ) ;
#22853 = CARTESIAN_POINT ( 'NONE',  ( 47.87658044100083288, 39.99999999999999289, -82.67148682534872250 ) ) ;
#22854 = CARTESIAN_POINT ( 'NONE',  ( 5.657435538624008755E-15, 4.615443851143735910E-16, -20.00000000000001776 ) ) ;
#22855 = FACE_BOUND ( 'NONE', #36917, .T. ) ;
#22856 = ORIENTED_EDGE ( 'NONE', *, *, #8804, .F. ) ;
#22857 = CARTESIAN_POINT ( 'NONE',  ( 18.00000000000000355, -22.82995208772658557, -41.06517797613689424 ) ) ;
#22858 = ORIENTED_EDGE ( 'NONE', *, *, #10678, .F. ) ;
#22859 = CARTESIAN_POINT ( 'NONE',  ( 17.99999999999999645, 0.000000000000000000, 0.000000000000000000 ) ) ;
#22860 = VECTOR ( 'NONE', #20597, 1000.000000000000000 ) ;
#22861 = CARTESIAN_POINT ( 'NONE',  ( 17.99999999999999645, -5.822172717930484964, 31.41458249383138934 ) ) ;
#22862 = DIRECTION ( 'NONE',  ( -1.000000000000000000, -0.000000000000000000, 0.000000000000000000 ) ) ;
#22863 = ORIENTED_EDGE ( 'NONE', *, *, #27106, .F. ) ;
#22864 = FACE_BOUND ( 'NONE', #24798, .T. ) ;
#22865 = VECTOR ( 'NONE', #24517, 1000.000000000000000 ) ;
#22866 = DIRECTION ( 'NONE',  ( 0.000000000000000000, 0.000000000000000000, 1.000000000000000000 ) ) ;
#22867 = CARTESIAN_POINT ( 'NONE',  ( 4.000000000000000000, -2.471525695159793035, -3.686886880705770864 ) ) ;
#22868 = CIRCLE ( 'NONE', #28434, 20.00000000000000711 ) ;
#22869 = VECTOR ( 'NONE', #24581, 1000.000000000000000 ) ;
#22871 = ORIENTED_EDGE ( 'NONE', *, *, #37739, .F. ) ;
#22870 = LINE ( 'NONE', #19580, #20846 ) ;
#22872 = EDGE_CURVE ( 'NONE', #32977, #14493, #31717, .T. ) ;
#22873 = CARTESIAN_POINT ( 'NONE',  ( -18.31940394017777507, 31.00000000000000355, -14.05611420671224288 ) ) ;
#22874 = ADVANCED_FACE ( 'NONE', ( #33924 ), #21539, .F. ) ;
#22875 = FACE_OUTER_BOUND ( 'NONE', #37164, .T. ) ;
#22876 = VECTOR ( 'NONE', #32994, 1000.000000000000000 ) ;
#22877 = EDGE_CURVE ( 'NONE', #9735, #14673, #5907, .T. ) ;
#22878 = ADVANCED_FACE ( 'NONE', ( #41091 ), #38055, .F. ) ;
#22880 = ORIENTED_EDGE ( 'NONE', *, *, #34366, .F. ) ;
#22879 = CARTESIAN_POINT ( 'NONE',  ( -10.00000000000000000, 0.000000000000000000, 0.000000000000000000 ) ) ;
#22881 = ORIENTED_EDGE ( 'NONE', *, *, #8850, .T. ) ;
#22882 = DIRECTION ( 'NONE',  ( 0.000000000000000000, 0.2486898871648552389, -0.9685831611286309650 ) ) ;
#22883 = CARTESIAN_POINT ( 'NONE',  ( 0.000000000000000000, -37.07968990261553444, 109.9140418541956308 ) ) ;
#22884 = CARTESIAN_POINT ( 'NONE',  ( -38.37160831358556123, 40.00000000000000000, -19.00137192356237392 ) ) ;
#22885 = DIRECTION ( 'NONE',  ( 0.000000000000000000, -4.539683130352864453E-14, -1.000000000000000000 ) ) ;
#22886 = APPLICATION_CONTEXT ( 'automotive_design' ) ;
#22887 = CIRCLE ( 'NONE', #33985, 59.00000000000000000 ) ;
#22888 = CARTESIAN_POINT ( 'NONE',  ( 18.00000000000000355, 0.000000000000000000, 0.000000000000000000 ) ) ;
#22889 = CARTESIAN_POINT ( 'NONE',  ( 0.000000000000000000, -40.13512380274045199, 113.6206972269520179 ) ) ;
#22890 = EDGE_LOOP ( 'NONE', ( #15648, #28589, #31133, #31809 ) ) ;
#22891 = DIRECTION ( 'NONE',  ( 0.000000000000000000, -0.5877852522924802425, 0.8090169943749421222 ) ) ;
#22892 = VERTEX_POINT ( 'NONE', #34789 ) ;
#22893 = CARTESIAN_POINT ( 'NONE',  ( 17.99999999999999645, 99.97660604679964536, 67.26937820704921478 ) ) ;
#22894 = CYLINDRICAL_SURFACE ( 'NONE', #11573, 116.0000000000000000 ) ;
#22895 = CARTESIAN_POINT ( 'NONE',  ( -16.75480014238754478, 31.00000000000000355, -49.32177912249007790 ) ) ;
#22896 = CIRCLE ( 'NONE', #4010, 13.59999999999999964 ) ;
#22897 = DIRECTION ( 'NONE',  ( -1.000000000000000000, -0.000000000000000000, -0.000000000000000000 ) ) ;
#22898 = ORIENTED_EDGE ( 'NONE', *, *, #2741, .F. ) ;
#22899 = VECTOR ( 'NONE', #33376, 1000.000000000000000 ) ;
#22900 = AXIS2_PLACEMENT_3D ( 'NONE', #779, #993, #34382 ) ;
#22901 = CARTESIAN_POINT ( 'NONE',  ( 47.55521504368574881, -2.055254544495723756, -70.64469547305695585 ) ) ;
#22902 = EDGE_CURVE ( 'NONE', #24319, #30609, #28927, .T. ) ;
#22903 = CARTESIAN_POINT ( 'NONE',  ( 91.55691129138550366, 31.00000000000000000, -24.53049628908797430 ) ) ;
#22904 = AXIS2_PLACEMENT_3D ( 'NONE', #18234, #8355, #37379 ) ;
#22905 = ADVANCED_FACE ( 'NONE', ( #14962 ), #34134, .T. ) ;
#22906 = CARTESIAN_POINT ( 'NONE',  ( 0.000000000000000000, 103.1672962317657323, -44.09967643725766351 ) ) ;
#22907 = ORIENTED_EDGE ( 'NONE', *, *, #8209, .F. ) ;
#22909 = CARTESIAN_POINT ( 'NONE',  ( 66.37122006405570573, 31.00000000000000000, -8.639838683444628131 ) ) ;
#22908 = CIRCLE ( 'NONE', #27778, 116.0000000000000000 ) ;
#22910 = CARTESIAN_POINT ( 'NONE',  ( 57.47007747233163144, 39.99999999999999289, -33.06854485814638878 ) ) ;
#22911 = CYLINDRICAL_SURFACE ( 'NONE', #27367, 2.649999999999993694 ) ;
#22912 = ORIENTED_EDGE ( 'NONE', *, *, #33642, .F. ) ;
#22913 = LINE ( 'NONE', #16569, #13010 ) ;
#22914 = DIRECTION ( 'NONE',  ( -1.847415842360817484E-16, 1.000000000000000000, 0.000000000000000000 ) ) ;
#22915 = CARTESIAN_POINT ( 'NONE',  ( 17.99999999999999645, 13.22719389141978930, 28.58720592780601066 ) ) ;
#22916 = AXIS2_PLACEMENT_3D ( 'NONE', #29348, #5764, #32812 ) ;
#22918 = EDGE_LOOP ( 'NONE', ( #20957, #2498, #1303, #24937 ) ) ;
#22917 = CARTESIAN_POINT ( 'NONE',  ( 17.99999999999999645, 16.86122981692017930, 27.13802899033298388 ) ) ;
#22919 = DIRECTION ( 'NONE',  ( 0.000000000000000000, 0.8183027759081701324, -0.5747874102144052699 ) ) ;
#22920 = DIRECTION ( 'NONE',  ( 1.000000000000000000, -0.000000000000000000, 0.000000000000000000 ) ) ;
#22921 = CARTESIAN_POINT ( 'NONE',  ( 38.42722039544141666, 40.00000000000000000, 66.52996821281629991 ) ) ;
#22922 = DIRECTION ( 'NONE',  ( 1.000000000000000000, 0.000000000000000000, 0.000000000000000000 ) ) ;
#22923 = VERTEX_POINT ( 'NONE', #11687 ) ;
#22924 = EDGE_CURVE ( 'NONE', #7516, #34509, #10804, .T. ) ;
#22925 = CARTESIAN_POINT ( 'NONE',  ( 17.99999999999999645, 0.000000000000000000, 0.000000000000000000 ) ) ;
#22927 = EDGE_CURVE ( 'NONE', #21211, #10833, #40655, .T. ) ;
#22926 = AXIS2_PLACEMENT_3D ( 'NONE', #38856, #6126, #35376 ) ;
#22928 = CARTESIAN_POINT ( 'NONE',  ( 18.00000000000000355, -42.60732521687585006, 19.80331771201644031 ) ) ;
#22929 = AXIS2_PLACEMENT_3D ( 'NONE', #42285, #12011, #28799 ) ;
#22930 = EDGE_CURVE ( 'NONE', #12909, #33094, #21296, .T. ) ;
#22931 = ADVANCED_FACE ( 'NONE', ( #7520 ), #14301, .T. ) ;
#22932 = ORIENTED_EDGE ( 'NONE', *, *, #20444, .T. ) ;
#22933 = CIRCLE ( 'NONE', #6150, 52.00000000000000000 ) ;
#22934 = ADVANCED_FACE ( 'NONE', ( #11035 ), #17604, .F. ) ;
#22935 = ORIENTED_EDGE ( 'NONE', *, *, #2094, .F. ) ;
#22936 = DIRECTION ( 'NONE',  ( -1.000000000000000000, -0.000000000000000000, 0.000000000000000000 ) ) ;
#22937 = ORIENTED_EDGE ( 'NONE', *, *, #9278, .T. ) ;
#22938 = AXIS2_PLACEMENT_3D ( 'NONE', #36468, #3074, #42588 ) ;
#22939 = CARTESIAN_POINT ( 'NONE',  ( 0.000000000000000000, 109.3506818544115617, -38.70953859160899668 ) ) ;
#22940 = CARTESIAN_POINT ( 'NONE',  ( 2.499999999999999556, 0.000000000000000000, 3.469446951953614189E-15 ) ) ;
#22941 = DIRECTION ( 'NONE',  ( -1.000000000000000000, 0.000000000000000000, -0.000000000000000000 ) ) ;
#22942 = CARTESIAN_POINT ( 'NONE',  ( 6.004904395537136175, 2.351321854362917684E-15, -19.19999999999999574 ) ) ;
#22943 = ORIENTED_EDGE ( 'NONE', *, *, #12667, .F. ) ;
#22944 = DIRECTION ( 'NONE',  ( 1.000000000000000000, 1.836909530733573776E-16, 0.000000000000000000 ) ) ;
#22945 = VERTEX_POINT ( 'NONE', #24363 ) ;
#22946 = FACE_OUTER_BOUND ( 'NONE', #11139, .T. ) ;
#22947 = ORIENTED_EDGE ( 'NONE', *, *, #21279, .T. ) ;
#22948 = DIRECTION ( 'NONE',  ( -1.000000000000000000, -0.000000000000000000, -0.000000000000000000 ) ) ;
#22949 = CARTESIAN_POINT ( 'NONE',  ( 0.000000000000000000, -92.25992191227442163, 77.51514567967366531 ) ) ;
#22950 = CONTEXT_DEPENDENT_SHAPE_REPRESENTATION ( #13113, #33590 ) ;
#22951 = CARTESIAN_POINT ( 'NONE',  ( 0.000000000000000000, 34.45183346761150034, -10.44371441202619621 ) ) ;
#22952 = CARTESIAN_POINT ( 'NONE',  ( -18.68892229297488683, 31.00000000000000355, 55.06009237583231197 ) ) ;
#22953 = VECTOR ( 'NONE', #29926, 1000.000000000000000 ) ;
#22954 = EDGE_LOOP ( 'NONE', ( #12976, #30114, #16910, #4015 ) ) ;
#22955 = AXIS2_PLACEMENT_3D ( 'NONE', #5801, #5597, #41812 ) ;
#22956 = CARTESIAN_POINT ( 'NONE',  ( -2.197745971918068530, 31.00000000000000355, -34.39891587002171036 ) ) ;
#22957 = CARTESIAN_POINT ( 'NONE',  ( 49.83821931962687302, 40.00000000000000000, 43.70611527624207326 ) ) ;
#22958 = AXIS2_PLACEMENT_3D ( 'NONE', #26046, #35423, #2037 ) ;
#22959 = DIRECTION ( 'NONE',  ( 1.000000000000000000, 0.000000000000000000, 0.000000000000000000 ) ) ;
#22960 = DIRECTION ( 'NONE',  ( -1.000000000000000000, 0.000000000000000000, -0.000000000000000000 ) ) ;
#22961 = DIRECTION ( 'NONE',  ( -1.000000000000000000, 0.000000000000000000, 0.000000000000000000 ) ) ;
#22962 = DIRECTION ( 'NONE',  ( -1.000000000000000000, -0.000000000000000000, -0.000000000000000000 ) ) ;
#22963 = ORIENTED_EDGE ( 'NONE', *, *, #20968, .T. ) ;
#22964 = CARTESIAN_POINT ( 'NONE',  ( 12.21457428495364006, 40.00000000000000000, 45.57612047952555656 ) ) ;
#22965 = DIRECTION ( 'NONE',  ( 0.000000000000000000, 3.528251137579946599E-15, -1.000000000000000000 ) ) ;
#22966 = DIRECTION ( 'NONE',  ( -3.996523416598930318E-16, 2.658563593772947863E-15, 1.000000000000000000 ) ) ;
#22967 = ORIENTED_EDGE ( 'NONE', *, *, #42552, .F. ) ;
#22968 = CARTESIAN_POINT ( 'NONE',  ( 17.99999999999999645, 31.81777574834305966, 10.70123563439457293 ) ) ;
#22969 = CARTESIAN_POINT ( 'NONE',  ( 18.00000000000000355, 47.22458491092827160, -5.098390039073737334 ) ) ;
#22970 = EDGE_CURVE ( 'NONE', #42093, #3574, #17139, .T. ) ;
#22971 = EDGE_CURVE ( 'NONE', #36509, #19787, #31314, .T. ) ;
#22972 = ORIENTED_EDGE ( 'NONE', *, *, #33267, .F. ) ;
#22973 = CARTESIAN_POINT ( 'NONE',  ( 42.80287614962790599, -40.05525454449572464, 69.29271901957253021 ) ) ;
#22974 = VERTEX_POINT ( 'NONE', #34348 ) ;
#22975 = EDGE_CURVE ( 'NONE', #4068, #42073, #3830, .T. ) ;
#22976 = EDGE_LOOP ( 'NONE', ( #22397, #36092, #9216, #27574 ) ) ;
#22977 = LINE ( 'NONE', #6341, #23719 ) ;
#22978 = CARTESIAN_POINT ( 'NONE',  ( 77.87745995352098305, 31.00000000000000000, 59.89653754214596404 ) ) ;
#22979 = ORIENTED_EDGE ( 'NONE', *, *, #41900, .T. ) ;
#22980 = LINE ( 'NONE', #36879, #22412 ) ;
#22981 = AXIS2_PLACEMENT_3D ( 'NONE', #19937, #22781, #3505 ) ;
#22982 = CARTESIAN_POINT ( 'NONE',  ( 106.4195705685741302, 106.4195705685767166, 9.999999999999998224 ) ) ;
#22983 = DIRECTION ( 'NONE',  ( 0.000000000000000000, 0.000000000000000000, 1.000000000000000000 ) ) ;
#22984 = VECTOR ( 'NONE', #31032, 1000.000000000000000 ) ;
#22985 = ORIENTED_EDGE ( 'NONE', *, *, #27032, .F. ) ;
#22986 = EDGE_CURVE ( 'NONE', #19747, #36818, #12944, .T. ) ;
#22987 = DIRECTION ( 'NONE',  ( -1.000000000000000000, -0.000000000000000000, -0.000000000000000000 ) ) ;
#22988 = DIRECTION ( 'NONE',  ( 1.000000000000000000, 0.000000000000000000, 0.000000000000000000 ) ) ;
#22989 = EDGE_CURVE ( 'NONE', #170, #17173, #23385, .T. ) ;
#22991 = CARTESIAN_POINT ( 'NONE',  ( 17.99999999999999645, -78.18175027177375114, -85.69488855493077040 ) ) ;
#22990 = CARTESIAN_POINT ( 'NONE',  ( 8.999999999999998224, -68.63002662989811142, 93.51962064069482494 ) ) ;
#22992 = CARTESIAN_POINT ( 'NONE',  ( 17.99999999999999645, 3.803237743091921974, 31.26855263151016828 ) ) ;
#22993 = ORIENTED_EDGE ( 'NONE', *, *, #29593, .F. ) ;
#22994 = AXIS2_PLACEMENT_3D ( 'NONE', #3118, #12997, #22409 ) ;
#22995 = CARTESIAN_POINT ( 'NONE',  ( 16.69935377588158332, 31.00000000000000355, -28.93150767131472989 ) ) ;
#22996 = ORIENTED_EDGE ( 'NONE', *, *, #3461, .F. ) ;
#22997 = CARTESIAN_POINT ( 'NONE',  ( 150.4999999999986926, 1.396217360982896810E-12, 9.999999999999960920 ) ) ;
#22998 = DIRECTION ( 'NONE',  ( 0.000000000000000000, 0.000000000000000000, -1.000000000000000000 ) ) ;
#22999 = VERTEX_POINT ( 'NONE', #28495 ) ;
#23000 = DIRECTION ( 'NONE',  ( -1.000000000000000000, -0.000000000000000000, -0.000000000000000000 ) ) ;
#23001 = CARTESIAN_POINT ( 'NONE',  ( 24.02862666965263116, 40.00000000000000000, 27.38392887651082575 ) ) ;
#23002 = CARTESIAN_POINT ( 'NONE',  ( -38.37160831358556123, 40.00000000000000000, -19.00137192356237392 ) ) ;
#23003 = VECTOR ( 'NONE', #18691, 1000.000000000000000 ) ;
#23004 = EDGE_LOOP ( 'NONE', ( #38211, #22501, #41740, #424 ) ) ;
#23005 = EDGE_LOOP ( 'NONE', ( #36962, #24531, #33491, #21122 ) ) ;
#23006 = CARTESIAN_POINT ( 'NONE',  ( 17.99999999999999645, 0.000000000000000000, 0.000000000000000000 ) ) ;
#23007 = CARTESIAN_POINT ( 'NONE',  ( 18.00000000000000355, 22.43957647427161461, 41.27978878573636479 ) ) ;
#23008 = CIRCLE ( 'NONE', #13211, 2.649999999999957723 ) ;
#23009 = CARTESIAN_POINT ( 'NONE',  ( 17.99999999999999645, 0.000000000000000000, 0.000000000000000000 ) ) ;
#23010 = LINE ( 'NONE', #19515, #16190 ) ;
#23011 = FACE_OUTER_BOUND ( 'NONE', #32452, .T. ) ;
#23012 = ORIENTED_EDGE ( 'NONE', *, *, #8070, .F. ) ;
#23013 = CARTESIAN_POINT ( 'NONE',  ( 18.00000000000000355, 0.000000000000000000, 0.000000000000000000 ) ) ;
#23014 = ORIENTED_EDGE ( 'NONE', *, *, #12087, .F. ) ;
#23015 = CARTESIAN_POINT ( 'NONE',  ( 17.99999999999999645, 13.00789606333630566, -115.2683592318613819 ) ) ;
#23016 = DIRECTION ( 'NONE',  ( -3.996523416598930318E-16, 2.658563593772947863E-15, 1.000000000000000000 ) ) ;
#23017 = DIRECTION ( 'NONE',  ( 1.000000000000000000, 0.000000000000000000, 0.000000000000000000 ) ) ;
#23018 = ADVANCED_FACE ( 'NONE', ( #22587 ), #19314, .T. ) ;
#23019 = CARTESIAN_POINT ( 'NONE',  ( 17.99999999999999645, -2.007101075699733173, -31.43498920425971832 ) ) ;
#23020 = VERTEX_POINT ( 'NONE', #2240 ) ;
#23021 = CARTESIAN_POINT ( 'NONE',  ( 0.000000000000000000, 107.1354928292875996, -44.47455650397954230 ) ) ;
#23022 = ORIENTED_EDGE ( 'NONE', *, *, #10929, .T. ) ;
#23023 = EDGE_CURVE ( 'NONE', #36227, #39315, #38909, .T. ) ;
#23024 = DIRECTION ( 'NONE',  ( 0.000000000000000000, 0.000000000000000000, 1.000000000000000000 ) ) ;
#23025 = ORIENTED_EDGE ( 'NONE', *, *, #25762, .T. ) ;
#23027 = ORIENTED_EDGE ( 'NONE', *, *, #20578, .F. ) ;
#23026 = DIRECTION ( 'NONE',  ( 1.000000000000000000, -3.336006684570784581E-17, 0.000000000000000000 ) ) ;
#23028 = CARTESIAN_POINT ( 'NONE',  ( -8.314562429035724733, 31.00000000000000355, -63.88718494334916187 ) ) ;
#23029 = ORIENTED_EDGE ( 'NONE', *, *, #3582, .T. ) ;
#23030 = DIRECTION ( 'NONE',  ( -1.000000000000000000, 0.000000000000000000, 0.000000000000000000 ) ) ;
#23031 = ORIENTED_EDGE ( 'NONE', *, *, #18598, .F. ) ;
#23032 = EDGE_CURVE ( 'NONE', #17179, #26181, #3146, .T. ) ;
#23033 = CARTESIAN_POINT ( 'NONE',  ( 0.000000000000000000, 3.840921266749842022, 47.34345070675171030 ) ) ;
#23034 = ORIENTED_EDGE ( 'NONE', *, *, #26066, .F. ) ;
#23035 = CARTESIAN_POINT ( 'NONE',  ( 74.83201185296370284, 39.99999999999999289, -43.08100868844128684 ) ) ;
#23036 = CIRCLE ( 'NONE', #18877, 52.00000000000000000 ) ;
#23037 = ADVANCED_FACE ( 'NONE', ( #32159, #32584 ), #2040, .T. ) ;
#23038 = CIRCLE ( 'NONE', #33428, 64.99999999999998579 ) ;
#23040 = DIRECTION ( 'NONE',  ( -1.000000000000000000, 0.000000000000000000, 0.000000000000000000 ) ) ;
#23039 = CARTESIAN_POINT ( 'NONE',  ( 17.99999999999999645, 0.000000000000000000, 0.000000000000000000 ) ) ;
#23041 = CARTESIAN_POINT ( 'NONE',  ( 17.99999999999999645, 0.000000000000000000, 0.000000000000000000 ) ) ;
#23042 = EDGE_LOOP ( 'NONE', ( #35548, #11862, #2708, #23905 ) ) ;
#23043 = CARTESIAN_POINT ( 'NONE',  ( -10.00000000000000000, 0.000000000000000000, 0.000000000000000000 ) ) ;
#23044 = ORIENTED_EDGE ( 'NONE', *, *, #16474, .F. ) ;
#23045 =( LENGTH_UNIT ( ) NAMED_UNIT ( * ) SI_UNIT ( .MILLI., .METRE. ) );
#23046 = DIRECTION ( 'NONE',  ( -1.000000000000000000, -0.000000000000000000, -0.000000000000000000 ) ) ;
#23047 = CARTESIAN_POINT ( 'NONE',  ( 17.99999999999999645, 0.000000000000000000, 0.000000000000000000 ) ) ;
#23048 = CARTESIAN_POINT ( 'NONE',  ( 60.46509673945340779, 31.00000000000000000, 46.37897171330492085 ) ) ;
#23050 = DIRECTION ( 'NONE',  ( -1.000000000000000000, 0.000000000000000000, 0.000000000000000000 ) ) ;
#23049 = DIRECTION ( 'NONE',  ( 0.000000000000000000, 0.000000000000000000, 1.000000000000000000 ) ) ;
#23051 = ORIENTED_EDGE ( 'NONE', *, *, #26695, .F. ) ;
#23052 = DIRECTION ( 'NONE',  ( 0.000000000000000000, 0.000000000000000000, 1.000000000000000000 ) ) ;
#23053 = ADVANCED_FACE ( 'NONE', ( #25228 ), #28902, .T. ) ;
#23054 = AXIS2_PLACEMENT_3D ( 'NONE', #12241, #15323, #5244 ) ;
#23055 = ORIENTED_EDGE ( 'NONE', *, *, #2257, .T. ) ;
#23056 = CARTESIAN_POINT ( 'NONE',  ( 17.99999999999999645, 107.1354928292875996, -44.47455650397954230 ) ) ;
#23057 = EDGE_CURVE ( 'NONE', #14617, #26000, #27586, .T. ) ;
#23058 = DIRECTION ( 'NONE',  ( 1.000000000000000000, 0.000000000000000000, 0.000000000000000000 ) ) ;
#23059 = CARTESIAN_POINT ( 'NONE',  ( -55.31949386280458469, 31.00000000000000711, 71.91600076666669850 ) ) ;
#23060 = CARTESIAN_POINT ( 'NONE',  ( 87.78546986784174067, 39.99999999999999289, 43.41392487578124815 ) ) ;
#23061 = CARTESIAN_POINT ( 'NONE',  ( 0.000000000000000000, 0.000000000000000000, 0.000000000000000000 ) ) ;
#23062 = AXIS2_PLACEMENT_3D ( 'NONE', #37207, #36783, #40261 ) ;
#23063 = CARTESIAN_POINT ( 'NONE',  ( 0.000000000000000000, 39.78933988720115877, 24.98727647985016276 ) ) ;
#23064 = ORIENTED_EDGE ( 'NONE', *, *, #8268, .F. ) ;
#23065 = CARTESIAN_POINT ( 'NONE',  ( 0.000000000000000000, 0.000000000000000000, 0.000000000000000000 ) ) ;
#23066 = ORIENTED_EDGE ( 'NONE', *, *, #22354, .T. ) ;
#23067 = AXIS2_PLACEMENT_3D ( 'NONE', #20896, #544, #30679 ) ;
#23068 = CARTESIAN_POINT ( 'NONE',  ( 18.00000000000000355, 43.83938735307268075, 18.28286404005813637 ) ) ;
#23069 = VECTOR ( 'NONE', #9144, 1000.000000000000000 ) ;
#23070 = CARTESIAN_POINT ( 'NONE',  ( 22.90854556226710415, -35.35525454449573601, -74.83297477053821467 ) ) ;
#23071 = VECTOR ( 'NONE', #26842, 1000.000000000000000 ) ;
#23072 = CARTESIAN_POINT ( 'NONE',  ( 0.000000000000000000, 31.08872492060014281, -41.68322423723068226 ) ) ;
#23073 = ORIENTED_EDGE ( 'NONE', *, *, #32193, .F. ) ;
#23074 = DIRECTION ( 'NONE',  ( 1.000000000000000000, -0.000000000000000000, -0.000000000000000000 ) ) ;
#23075 = ADVANCED_FACE ( 'NONE', ( #38474 ), #22379, .F. ) ;
#23076 = CARTESIAN_POINT ( 'NONE',  ( 17.99999999999999645, 11.41303419184972689, 111.6154788735836405 ) ) ;
#23077 = CARTESIAN_POINT ( 'NONE',  ( 17.99999999999999645, 9.484061862024356415, -30.03730300138970932 ) ) ;
#23079 = ORIENTED_EDGE ( 'NONE', *, *, #17361, .F. ) ;
#23078 = DIRECTION ( 'NONE',  ( 0.000000000000000000, 0.000000000000000000, 1.000000000000000000 ) ) ;
#23080 = CARTESIAN_POINT ( 'NONE',  ( 34.63398384099731686, 31.00000000000000355, -11.69655689657770203 ) ) ;
#23081 = CYLINDRICAL_SURFACE ( 'NONE', #31568, 116.0000000000000000 ) ;
#23082 = EDGE_CURVE ( 'NONE', #12005, #14223, #15193, .T. ) ;
#23084 = VERTEX_POINT ( 'NONE', #18468 ) ;
#23083 = CYLINDRICAL_SURFACE ( 'NONE', #282, 58.99999999999999289 ) ;
#23085 = ORIENTED_EDGE ( 'NONE', *, *, #5238, .F. ) ;
#23086 = CARTESIAN_POINT ( 'NONE',  ( 17.99999999999999645, 0.000000000000000000, 0.000000000000000000 ) ) ;
#23087 = DIRECTION ( 'NONE',  ( -1.000000000000000000, -0.000000000000000000, -0.000000000000000000 ) ) ;
#23088 = CARTESIAN_POINT ( 'NONE',  ( -44.44570800418432555, 40.00000000000000000, 25.56477902013099524 ) ) ;
#23089 = CARTESIAN_POINT ( 'NONE',  ( 18.00000000000000355, 22.82995208772688756, 41.06517797613672371 ) ) ;
#23090 = AXIS2_PLACEMENT_3D ( 'NONE', #6742, #33789, #21179 ) ;
#23091 = ADVANCED_FACE ( 'NONE', ( #8816 ), #9025, .T. ) ;
#23092 = CARTESIAN_POINT ( 'NONE',  ( -2.805705207896067144, 3.226868319750155312, -3.503898532754364581 ) ) ;
#23093 = EDGE_CURVE ( 'NONE', #13228, #16681, #18560, .T. ) ;
#23094 = LINE ( 'NONE', #19594, #8124 ) ;
#23095 = CIRCLE ( 'NONE', #4222, 2.500000000000002665 ) ;
#23096 = ORIENTED_EDGE ( 'NONE', *, *, #3344, .F. ) ;
#23097 = CYLINDRICAL_SURFACE ( 'NONE', #39043, 120.5010000000000190 ) ;
#23098 = ORIENTED_EDGE ( 'NONE', *, *, #20230, .T. ) ;
#23099 = AXIS2_PLACEMENT_3D ( 'NONE', #42819, #9891, #2466 ) ;
#23100 = CYLINDRICAL_SURFACE ( 'NONE', #16219, 116.0000000000000000 ) ;
#23101 = DIRECTION ( 'NONE',  ( 0.000000000000000000, 0.000000000000000000, 1.000000000000000000 ) ) ;
#23102 = AXIS2_PLACEMENT_3D ( 'NONE', #20610, #33885, #38 ) ;
#23103 = CARTESIAN_POINT ( 'NONE',  ( -32.14164714139042189, 31.00000000000000355, 36.65395011347077059 ) ) ;
#23104 = DIRECTION ( 'NONE',  ( -1.000000000000000000, -0.000000000000000000, -0.000000000000000000 ) ) ;
#23105 = ORIENTED_EDGE ( 'NONE', *, *, #8126, .F. ) ;
#23106 = VECTOR ( 'NONE', #23330, 1000.000000000000114 ) ;
#23107 = DIRECTION ( 'NONE',  ( 0.000000000000000000, 0.1837495178165637344, 0.9829730996839030066 ) ) ;
#23108 = CARTESIAN_POINT ( 'NONE',  ( -70.72766149062127283, 31.00000000000000711, 54.26934393422349956 ) ) ;
#23109 = VECTOR ( 'NONE', #18920, 1000.000000000000000 ) ;
#23110 = EDGE_CURVE ( 'NONE', #32554, #23227, #16435, .T. ) ;
#23111 = DIRECTION ( 'NONE',  ( 1.000000000000000000, 0.000000000000000000, 0.000000000000000000 ) ) ;
#23112 = ORIENTED_EDGE ( 'NONE', *, *, #18639, .T. ) ;
#23113 = CARTESIAN_POINT ( 'NONE',  ( -61.40313508884858607, 31.00000000000000711, 7.989450542815522027 ) ) ;
#23114 = CARTESIAN_POINT ( 'NONE',  ( 65.23019871244166268, 39.99999999999999289, 17.57949444736078703 ) ) ;
#23115 = VECTOR ( 'NONE', #20159, 1000.000000000000000 ) ;
#23116 = DIRECTION ( 'NONE',  ( 0.000000000000000000, -0.3140767120219556952, 0.9493976084683789507 ) ) ;
#23117 = ORIENTED_EDGE ( 'NONE', *, *, #23886, .F. ) ;
#23118 = CARTESIAN_POINT ( 'NONE',  ( -0.6810597143197697489, -4.461075778259609770, -3.598441714920717516 ) ) ;
#23119 = LINE ( 'NONE', #6273, #11771 ) ;
#23120 = DIRECTION ( 'NONE',  ( -1.000000000000000000, -0.000000000000000000, 0.000000000000000000 ) ) ;
#23122 = ORIENTED_EDGE ( 'NONE', *, *, #34406, .F. ) ;
#23121 = DIRECTION ( 'NONE',  ( 0.000000000000000000, -0.5264321628773627193, 0.8502171357296098853 ) ) ;
#23123 = CARTESIAN_POINT ( 'NONE',  ( 17.99999999999999645, 0.000000000000000000, 0.000000000000000000 ) ) ;
#23124 = VERTEX_POINT ( 'NONE', #31735 ) ;
#23125 = CARTESIAN_POINT ( 'NONE',  ( 0.000000000000000000, 28.62203781743003717, 14.19692359621465094 ) ) ;
#23126 = ADVANCED_FACE ( 'NONE', ( #21951 ), #15399, .T. ) ;
#23127 = CARTESIAN_POINT ( 'NONE',  ( -9.469526743414824921, 40.00000000000000000, -71.82433816204535049 ) ) ;
#23128 = DIRECTION ( 'NONE',  ( -1.000000000000000000, -0.000000000000000000, 0.000000000000000000 ) ) ;
#23129 = CIRCLE ( 'NONE', #41862, 36.00000000000000000 ) ;
#23130 = ORIENTED_EDGE ( 'NONE', *, *, #13821, .T. ) ;
#23131 = DIRECTION ( 'NONE',  ( 0.000000000000000000, 0.000000000000000000, 1.000000000000000000 ) ) ;
#23132 = CARTESIAN_POINT ( 'NONE',  ( -17.77999999999999758, 0.000000000000000000, 11.00000000000000000 ) ) ;
#23133 = CIRCLE ( 'NONE', #14747, 13.59999999999999787 ) ;
#23134 = VERTEX_POINT ( 'NONE', #29120 ) ;
#23135 = ADVANCED_FACE ( 'NONE', ( #42393 ), #12111, .T. ) ;
#23136 = ORIENTED_EDGE ( 'NONE', *, *, #37138, .T. ) ;
#23137 = DIRECTION ( 'NONE',  ( 0.000000000000000000, 0.000000000000000000, 1.000000000000000000 ) ) ;
#23138 = ORIENTED_EDGE ( 'NONE', *, *, #28823, .F. ) ;
#23139 = CIRCLE ( 'NONE', #36315, 120.5010000000000190 ) ;
#23140 = DIRECTION ( 'NONE',  ( -1.058513553088275437E-16, -1.000000000000000000, 8.813324511995299047E-17 ) ) ;
#23141 = FACE_OUTER_BOUND ( 'NONE', #26955, .T. ) ;
#23142 = EDGE_CURVE ( 'NONE', #16188, #36371, #13637, .T. ) ;
#23143 = LINE ( 'NONE', #2992, #9358 ) ;
#23144 = DIRECTION ( 'NONE',  ( -1.000000000000000000, -0.000000000000000000, 0.000000000000000000 ) ) ;
#23145 = ORIENTED_EDGE ( 'NONE', *, *, #3528, .T. ) ;
#23146 = FACE_OUTER_BOUND ( 'NONE', #16091, .T. ) ;
#23147 = VERTEX_POINT ( 'NONE', #33438 ) ;
#23148 = DIRECTION ( 'NONE',  ( 0.000000000000000000, 0.8747630845319590565, 0.4845508703326540934 ) ) ;
#23149 = DIRECTION ( 'NONE',  ( 0.000000000000000000, 0.000000000000000000, 1.000000000000000000 ) ) ;
#23150 = ORIENTED_EDGE ( 'NONE', *, *, #33797, .F. ) ;
#23151 = CARTESIAN_POINT ( 'NONE',  ( 17.99999999999999645, 64.58410930313661424, -101.7319213743675732 ) ) ;
#23152 = CARTESIAN_POINT ( 'NONE',  ( 0.000000000000000000, -56.51398178981889941, 96.92493144647428949 ) ) ;
#23153 = DIRECTION ( 'NONE',  ( 1.000000000000000000, 0.000000000000000000, 0.000000000000000000 ) ) ;
#23154 = CARTESIAN_POINT ( 'NONE',  ( -59.40491426035100631, 31.00000000000000711, 7.833300799371349932 ) ) ;
#23155 = CIRCLE ( 'NONE', #30789, 23.00000000000000000 ) ;
#23156 = AXIS2_PLACEMENT_3D ( 'NONE', #13678, #6886, #26755 ) ;
#23157 = EDGE_CURVE ( 'NONE', #41075, #36558, #42148, .T. ) ;
#23158 = EDGE_CURVE ( 'NONE', #27215, #40017, #36576, .T. ) ;
#23159 = ORIENTED_EDGE ( 'NONE', *, *, #26985, .T. ) ;
#23160 = CARTESIAN_POINT ( 'NONE',  ( -5.264430561742837078, 31.00000000000000355, 39.44269128747090747 ) ) ;
#23161 = EDGE_CURVE ( 'NONE', #11572, #10180, #28959, .T. ) ;
#23162 = EDGE_CURVE ( 'NONE', #39096, #22718, #17831, .T. ) ;
#23163 = VECTOR ( 'NONE', #6124, 1000.000000000000000 ) ;
#23164 = CARTESIAN_POINT ( 'NONE',  ( 62.51641183113888900, 39.99999999999999289, -16.75201923384928548 ) ) ;
#23165 = AXIS2_PLACEMENT_3D ( 'NONE', #40368, #39924, #13365 ) ;
#23166 = LINE ( 'NONE', #19462, #22899 ) ;
#23167 = DIRECTION ( 'NONE',  ( -1.000000000000000000, -0.000000000000000000, 0.000000000000000000 ) ) ;
#23168 = LINE ( 'NONE', #16387, #18958 ) ;
#23169 = PRODUCT_DEFINITION_SHAPE ( 'NONE', 'NONE',  #20446 ) ;
#23170 = EDGE_LOOP ( 'NONE', ( #12912, #2953, #30181, #14120 ) ) ;
#23171 = CARTESIAN_POINT ( 'NONE',  ( -39.95047694894377344, 40.00000000000000000, -5.256506769647570465 ) ) ;
#23172 = DIRECTION ( 'NONE',  ( -1.000000000000000000, 0.000000000000000000, -0.000000000000000000 ) ) ;
#23173 = DIRECTION ( 'NONE',  ( 0.000000000000000000, 0.000000000000000000, 1.000000000000000000 ) ) ;
#23174 = ORIENTED_EDGE ( 'NONE', *, *, #11125, .T. ) ;
#23175 = CARTESIAN_POINT ( 'NONE',  ( 106.4195705685741302, 106.4195705685767166, 10.00000000000000000 ) ) ;
#23176 = CARTESIAN_POINT ( 'NONE',  ( 9.000000000000001776, -13.00789606333398218, -115.2683592318616235 ) ) ;
#23177 = ORIENTED_EDGE ( 'NONE', *, *, #3351, .T. ) ;
#23178 = LINE ( 'NONE', #36425, #32599 ) ;
#23179 = ORIENTED_EDGE ( 'NONE', *, *, #23420, .F. ) ;
#23180 = VECTOR ( 'NONE', #37268, 1000.000000000000000 ) ;
#23181 = CIRCLE ( 'NONE', #28751, 116.0000000000000000 ) ;
#23182 = ORIENTED_EDGE ( 'NONE', *, *, #18839, .F. ) ;
#23183 = CARTESIAN_POINT ( 'NONE',  ( -10.00000000000000000, 0.000000000000000000, 0.000000000000000000 ) ) ;
#23184 = CIRCLE ( 'NONE', #8512, 116.0000000000000000 ) ;
#23185 = CARTESIAN_POINT ( 'NONE',  ( 72.29027477042623673, 31.00000000000000000, -63.25088587033864229 ) ) ;
#23186 = ORIENTED_EDGE ( 'NONE', *, *, #8514, .F. ) ;
#23187 = FACE_OUTER_BOUND ( 'NONE', #37075, .T. ) ;
#23188 = AXIS2_PLACEMENT_3D ( 'NONE', #3205, #29229, #29883 ) ;
#23189 = DIRECTION ( 'NONE',  ( 0.000000000000000000, 0.000000000000000000, 1.000000000000000000 ) ) ;
#23190 = DIRECTION ( 'NONE',  ( 0.000000000000000000, 0.000000000000000000, 1.000000000000000000 ) ) ;
#23191 = ORIENTED_EDGE ( 'NONE', *, *, #10735, .T. ) ;
#23192 = FACE_OUTER_BOUND ( 'NONE', #7644, .T. ) ;
#23193 = AXIS2_PLACEMENT_3D ( 'NONE', #35123, #41229, #21014 ) ;
#23194 = DIRECTION ( 'NONE',  ( 0.000000000000000000, -0.1062934856473523454, -0.9943348002101385363 ) ) ;
#23196 = FACE_OUTER_BOUND ( 'NONE', #20917, .T. ) ;
#23195 = CYLINDRICAL_SURFACE ( 'NONE', #105, 59.00000000000000000 ) ;
#23197 = CARTESIAN_POINT ( 'NONE',  ( -10.00000000000000000, 0.000000000000000000, 0.000000000000000000 ) ) ;
#23198 = VERTEX_POINT ( 'NONE', #26690 ) ;
#23199 =( NAMED_UNIT ( * ) SI_UNIT ( $, .STERADIAN. ) SOLID_ANGLE_UNIT ( ) );
#23200 = CARTESIAN_POINT ( 'NONE',  ( -26.30698076681265363, 31.00000000000000355, 12.97770382244945253 ) ) ;
#23201 = VERTEX_POINT ( 'NONE', #29974 ) ;
#23202 = FACE_OUTER_BOUND ( 'NONE', #32348, .T. ) ;
#23203 = CARTESIAN_POINT ( 'NONE',  ( 17.99999999999999645, -110.3490479609630910, -20.28201389785511211 ) ) ;
#23204 = ORIENTED_EDGE ( 'NONE', *, *, #13057, .T. ) ;
#23205 = EDGE_CURVE ( 'NONE', #34831, #14426, #2431, .T. ) ;
#23206 = EDGE_CURVE ( 'NONE', #35006, #35211, #33821, .T. ) ;
#23207 = CARTESIAN_POINT ( 'NONE',  ( 5.000000000000002665, 0.000000000000000000, -2.700000000000000622 ) ) ;
#23208 = CARTESIAN_POINT ( 'NONE',  ( -36.61132647064156487, 40.00000000000000000, -18.04288060775211378 ) ) ;
#23209 = CARTESIAN_POINT ( 'NONE',  ( -51.46673615999394968, 40.00000000000000000, 6.691140578787329041 ) ) ;
#23210 = EDGE_CURVE ( 'NONE', #12319, #15523, #22715, .T. ) ;
#23211 = AXIS2_PLACEMENT_3D ( 'NONE', #21826, #18551, #42467 ) ;
#23212 = ORIENTED_EDGE ( 'NONE', *, *, #5461, .F. ) ;
#23213 = ORIENTED_EDGE ( 'NONE', *, *, #27809, .T. ) ;
#23214 = SURFACE_STYLE_FILL_AREA ( #22570 ) ;
#23215 = CARTESIAN_POINT ( 'NONE',  ( 18.00000000000000355, -19.44205635905511897, -43.33776004284629124 ) ) ;
#23216 = VECTOR ( 'NONE', #6286, 1000.000000000000000 ) ;
#23217 = CARTESIAN_POINT ( 'NONE',  ( 18.00000000000000355, -43.83938735307280865, 18.28286404005783083 ) ) ;
#23218 = DIRECTION ( 'NONE',  ( 0.000000000000000000, -0.9996456111234522934, -0.02662052143778445915 ) ) ;
#23219 = DIRECTION ( 'NONE',  ( 0.000000000000000000, 0.000000000000000000, 1.000000000000000000 ) ) ;
#23220 = ORIENTED_EDGE ( 'NONE', *, *, #7050, .F. ) ;
#23221 = DIRECTION ( 'NONE',  ( 0.000000000000000000, 0.9822872507286879440, 0.1873813145857286533 ) ) ;
#23222 = VERTEX_POINT ( 'NONE', #25 ) ;
#23223 = DIRECTION ( 'NONE',  ( -1.000000000000000000, -0.000000000000000000, 0.000000000000000000 ) ) ;
#23224 = AXIS2_PLACEMENT_3D ( 'NONE', #27925, #34219, #14618 ) ;
#23225 = DIRECTION ( 'NONE',  ( 1.058513553088275437E-16, 1.000000000000000000, -8.813324511995299047E-17 ) ) ;
#23226 = EDGE_CURVE ( 'NONE', #34279, #29542, #473, .T. ) ;
#23227 = VERTEX_POINT ( 'NONE', #26051 ) ;
#23228 = DIRECTION ( 'NONE',  ( 0.000000000000000000, 0.000000000000000000, 1.000000000000000000 ) ) ;
#23229 = FACE_OUTER_BOUND ( 'NONE', #42751, .T. ) ;
#23230 = ORIENTED_EDGE ( 'NONE', *, *, #10666, .F. ) ;
#23231 = DIRECTION ( 'NONE',  ( 0.000000000000000000, 0.000000000000000000, 1.000000000000000000 ) ) ;
#23232 = ORIENTED_EDGE ( 'NONE', *, *, #12405, .F. ) ;
#23233 = DIRECTION ( 'NONE',  ( 0.000000000000000000, 0.000000000000000000, 1.000000000000000000 ) ) ;
#23234 = ORIENTED_EDGE ( 'NONE', *, *, #16757, .F. ) ;
#23236 = VERTEX_POINT ( 'NONE', #23019 ) ;
#23235 = DIRECTION ( 'NONE',  ( 0.000000000000000000, 0.4132121857683728749, 0.9106347728549155640 ) ) ;
#23237 = CARTESIAN_POINT ( 'NONE',  ( 66.37122006405570573, 31.00000000000000000, -8.639838683444628131 ) ) ;
#23238 = ORIENTED_EDGE ( 'NONE', *, *, #17821, .F. ) ;
#23239 = CARTESIAN_POINT ( 'NONE',  ( 0.000000000000000000, -104.2166695095716591, 60.49278301857773243 ) ) ;
#23240 = ORIENTED_EDGE ( 'NONE', *, *, #18402, .F. ) ;
#23241 = CARTESIAN_POINT ( 'NONE',  ( -101.9145453900123641, 17.11489954122026447, -1.407535261550449501 ) ) ;
#23242 = ORIENTED_EDGE ( 'NONE', *, *, #24633, .F. ) ;
#23243 = AXIS2_PLACEMENT_3D ( 'NONE', #34373, #30895, #4709 ) ;
#23244 = CARTESIAN_POINT ( 'NONE',  ( -5.410573124821300262, 40.00000000000000000, -84.40011308931431699 ) ) ;
#23246 = DIRECTION ( 'NONE',  ( 1.000000000000000000, 0.000000000000000000, 0.000000000000000000 ) ) ;
#23245 = CARTESIAN_POINT ( 'NONE',  ( 17.99999999999999645, 0.000000000000000000, 0.000000000000000000 ) ) ;
#23247 = CARTESIAN_POINT ( 'NONE',  ( 0.000000000000000000, -12.30077720129063046, -50.52416135122093976 ) ) ;
#23248 = ORIENTED_EDGE ( 'NONE', *, *, #31932, .T. ) ;
#23249 = CYLINDRICAL_SURFACE ( 'NONE', #24300, 59.00000000000000000 ) ;
#23250 = STYLED_ITEM ( 'NONE', ( #25455 ), #1547 ) ;
#23251 = ORIENTED_EDGE ( 'NONE', *, *, #42438, .T. ) ;
#23252 = AXIS2_PLACEMENT_3D ( 'NONE', #33728, #3605, #3172 ) ;
#23253 = DIRECTION ( 'NONE',  ( 1.000000000000000000, 0.000000000000000000, -0.000000000000000000 ) ) ;
#23254 = CARTESIAN_POINT ( 'NONE',  ( 19.99305134020393382, 31.00000000000000355, 74.61661993947731730 ) ) ;
#23256 = FACE_OUTER_BOUND ( 'NONE', #9668, .T. ) ;
#23255 = DIRECTION ( 'NONE',  ( 0.000000000000000000, 0.000000000000000000, 1.000000000000000000 ) ) ;
#23257 = ORIENTED_EDGE ( 'NONE', *, *, #20637, .T. ) ;
#23258 = EDGE_CURVE ( 'NONE', #16681, #14052, #19228, .T. ) ;
#23259 = DIRECTION ( 'NONE',  ( 1.000000000000000000, 0.000000000000000000, 0.000000000000000000 ) ) ;
#23260 = ORIENTED_EDGE ( 'NONE', *, *, #2958, .F. ) ;
#23261 = DIRECTION ( 'NONE',  ( -1.000000000000000000, 0.000000000000000000, 0.000000000000000000 ) ) ;
#23262 = CYLINDRICAL_SURFACE ( 'NONE', #1132, 47.49900000000000233 ) ;
#23263 = CARTESIAN_POINT ( 'NONE',  ( 17.99999999999999645, -15.21076497709635156, -119.5371223922156503 ) ) ;
#23264 = EDGE_CURVE ( 'NONE', #23398, #25997, #6178, .T. ) ;
#23265 = AXIS2_PLACEMENT_3D ( 'NONE', #17315, #14225, #27528 ) ;
#23266 = DIRECTION ( 'NONE',  ( -1.000000000000000000, 0.000000000000000000, 0.000000000000000000 ) ) ;
#23267 = ADVANCED_FACE ( 'NONE', ( #32998, #238 ), #3085, .T. ) ;
#23268 = CARTESIAN_POINT ( 'NONE',  ( -2.797566391619251075E-15, 1.860994515641065082E-14, 7.000000000000002665 ) ) ;
#23269 = VERTEX_POINT ( 'NONE', #12960 ) ;
#23270 = FACE_OUTER_BOUND ( 'NONE', #2591, .T. ) ;
#23271 = VERTEX_POINT ( 'NONE', #16454 ) ;
#23272 = DIRECTION ( 'NONE',  ( 1.000000000000000000, 0.000000000000000000, -0.000000000000000000 ) ) ;
#23273 = ADVANCED_FACE ( 'NONE', ( #39958 ), #36702, .F. ) ;
#23274 = CARTESIAN_POINT ( 'NONE',  ( 17.99999999999999645, -56.51398178981757070, -96.92493144647505687 ) ) ;
#23275 = CARTESIAN_POINT ( 'NONE',  ( 0.000000000000000000, -107.2885202478269946, 54.86040852957277281 ) ) ;
#23276 = VERTEX_POINT ( 'NONE', #39746 ) ;
#23277 = DIRECTION ( 'NONE',  ( -1.000000000000000000, 0.000000000000000000, 0.000000000000000000 ) ) ;
#23278 = COLOUR_RGB ( '', 0.09019608, 0.27058824, 0.51372549) ;
#23279 = CARTESIAN_POINT ( 'NONE',  ( 18.00000000000000355, 0.000000000000000000, 0.000000000000000000 ) ) ;
#23280 = CARTESIAN_POINT ( 'NONE',  ( 2.649999999999993694, 150.5000000000000284, 6.999999999999998224 ) ) ;
#23281 = AXIS2_PLACEMENT_3D ( 'NONE', #11493, #4928, #17416 ) ;
#23283 = ORIENTED_EDGE ( 'NONE', *, *, #38288, .F. ) ;
#23282 = LINE ( 'NONE', #27187, #27826 ) ;
#23284 = CARTESIAN_POINT ( 'NONE',  ( 19.31996883370903362, 31.00000000000000355, 33.58758284028576924 ) ) ;
#23285 = DIRECTION ( 'NONE',  ( 0.000000000000000000, 0.000000000000000000, 1.000000000000000000 ) ) ;
#23286 = AXIS2_PLACEMENT_3D ( 'NONE', #17114, #30403, #17555 ) ;
#23288 = ORIENTED_EDGE ( 'NONE', *, *, #10424, .T. ) ;
#23287 = DIRECTION ( 'NONE',  ( 0.000000000000000000, -0.5877852522924624790, -0.8090169943749551118 ) ) ;
#23289 = ORIENTED_EDGE ( 'NONE', *, *, #15160, .T. ) ;
#23290 = CARTESIAN_POINT ( 'NONE',  ( 0.000000000000000000, 0.000000000000000000, 0.000000000000000000 ) ) ;
#23291 = ADVANCED_FACE ( 'NONE', ( #23229 ), #9877, .F. ) ;
#23292 = DIRECTION ( 'NONE',  ( -1.000000000000000000, -0.000000000000000000, 0.000000000000000000 ) ) ;
#23293 = CARTESIAN_POINT ( 'NONE',  ( 14.32751628686350287, 40.00000000000000000, -53.13354968558886071 ) ) ;
#23294 = DIRECTION ( 'NONE',  ( 0.000000000000000000, 0.9618256431728199329, -0.2736629900720799480 ) ) ;
#23295 = DIRECTION ( 'NONE',  ( 1.000000000000000000, 0.000000000000000000, 0.000000000000000000 ) ) ;
#23296 = CIRCLE ( 'NONE', #37889, 59.00000000000000711 ) ;
#23297 = CARTESIAN_POINT ( 'NONE',  ( 0.6666666666666658525, -4.233901974057276085, -3.300726591567086476 ) ) ;
#23298 = ORIENTED_EDGE ( 'NONE', *, *, #29852, .T. ) ;
#23299 = DIRECTION ( 'NONE',  ( 0.000000000000000000, 0.000000000000000000, 1.000000000000000000 ) ) ;
#23300 = VERTEX_POINT ( 'NONE', #6822 ) ;
#23301 = DIRECTION ( 'NONE',  ( 0.000000000000000000, 0.000000000000000000, 1.000000000000000000 ) ) ;
#23302 = DIRECTION ( 'NONE',  ( 0.000000000000000000, 0.000000000000000000, 1.000000000000000000 ) ) ;
#23303 = CARTESIAN_POINT ( 'NONE',  ( 36.61186797162192619, 31.00000000000000355, 28.07927795628900469 ) ) ;
#23304 = DIRECTION ( 'NONE',  ( 1.000000000000000000, 0.000000000000000000, -0.000000000000000000 ) ) ;
#23305 = ORIENTED_EDGE ( 'NONE', *, *, #23206, .F. ) ;
#23306 = PRODUCT_DEFINITION_FORMATION_WITH_SPECIFIED_SOURCE ( 'ANY', '', #35641, .NOT_KNOWN. ) ;
#23307 = ADVANCED_FACE ( 'NONE', ( #16900 ), #30180, .T. ) ;
#23308 = DIRECTION ( 'NONE',  ( -1.000000000000000000, 0.000000000000000000, 0.000000000000000000 ) ) ;
#23309 = EDGE_LOOP ( 'NONE', ( #42535, #30048, #25835, #24610 ) ) ;
#23310 = CARTESIAN_POINT ( 'NONE',  ( -89.22528799552154055, 31.00000000000000711, 43.99828826784794700 ) ) ;
#23311 = EDGE_LOOP ( 'NONE', ( #6891, #25633 ) ) ;
#23312 = DIRECTION ( 'NONE',  ( 0.000000000000000000, 0.000000000000000000, 1.000000000000000000 ) ) ;
#23313 = ORIENTED_EDGE ( 'NONE', *, *, #22377, .F. ) ;
#23314 = CARTESIAN_POINT ( 'NONE',  ( 63.11376326756305843, 31.00000000000000000, -21.32174659671377626 ) ) ;
#23315 = CARTESIAN_POINT ( 'NONE',  ( -16.51797447735934199, 40.00000000000000000, -62.05742538352703974 ) ) ;
#23316 = CARTESIAN_POINT ( 'NONE',  ( 17.99999999999999645, 94.52951811191651643, -67.23221107124801676 ) ) ;
#23317 = EDGE_CURVE ( 'NONE', #2864, #27244, #35890, .T. ) ;
#23318 = ORIENTED_EDGE ( 'NONE', *, *, #41206, .F. ) ;
#23319 = EDGE_LOOP ( 'NONE', ( #42182, #9592, #35578, #25273 ) ) ;
#23320 = CARTESIAN_POINT ( 'NONE',  ( -0.5449313310646672903, -4.304185902836978883, -3.316620875263469159 ) ) ;
#23321 = VECTOR ( 'NONE', #4667, 1000.000000000000000 ) ;
#23322 = DIRECTION ( 'NONE',  ( -1.000000000000000000, 0.000000000000000000, 0.000000000000000000 ) ) ;
#23323 = DIRECTION ( 'NONE',  ( 0.000000000000000000, 0.000000000000000000, 1.000000000000000000 ) ) ;
#23324 = CIRCLE ( 'NONE', #12203, 20.00000000000000355 ) ;
#23326 = ORIENTED_EDGE ( 'NONE', *, *, #23485, .T. ) ;
#23325 = DIRECTION ( 'NONE',  ( 0.000000000000000000, -0.5000000000000009992, -0.8660254037844380415 ) ) ;
#23327 = EDGE_CURVE ( 'NONE', #12380, #17388, #27619, .T. ) ;
#23328 = DIRECTION ( 'NONE',  ( 0.000000000000000000, 0.000000000000000000, 1.000000000000000000 ) ) ;
#23329 = ORIENTED_EDGE ( 'NONE', *, *, #24194, .F. ) ;
#23330 = DIRECTION ( 'NONE',  ( 0.1305261922200494362, 0.9914448613738107152, -0.000000000000000000 ) ) ;
#23331 = CIRCLE ( 'NONE', #8659, 20.00000000000000711 ) ;
#23332 = CARTESIAN_POINT ( 'NONE',  ( 82.68608547523962216, 39.99999999999999289, 22.14036602612658200 ) ) ;
#23333 = DIRECTION ( 'NONE',  ( 0.000000000000000000, -0.2486898871648622611, 0.9685831611286290777 ) ) ;
#23334 = ORIENTED_EDGE ( 'NONE', *, *, #20142, .T. ) ;
#23335 = CARTESIAN_POINT ( 'NONE',  ( 0.000000000000000000, -118.8387007424469601, -19.94628303336605768 ) ) ;
#23336 = DIRECTION ( 'NONE',  ( -1.000000000000000000, -0.000000000000000000, -0.000000000000000000 ) ) ;
#23337 = ORIENTED_EDGE ( 'NONE', *, *, #15713, .F. ) ;
#23338 = ORIENTED_EDGE ( 'NONE', *, *, #16874, .T. ) ;
#23339 = CARTESIAN_POINT ( 'NONE',  ( -10.00000000000000000, 0.000000000000000000, 0.000000000000000000 ) ) ;
#23341 = VERTEX_POINT ( 'NONE', #30825 ) ;
#23340 = ADVANCED_FACE ( 'NONE', ( #37351 ), #21261, .F. ) ;
#23342 = CARTESIAN_POINT ( 'NONE',  ( -22.10416666678001718, 40.00000000000000000, -1.441157586896875564 ) ) ;
#23343 = FACE_OUTER_BOUND ( 'NONE', #23170, .T. ) ;
#23344 = CYLINDRICAL_SURFACE ( 'NONE', #22810, 20.00000000000000355 ) ;
#23345 = EDGE_CURVE ( 'NONE', #25590, #8139, #10893, .T. ) ;
#23346 = DIRECTION ( 'NONE',  ( -0.000000000000000000, -0.000000000000000000, 1.000000000000000000 ) ) ;
#23347 = CLOSED_SHELL ( 'NONE', ( #36295, #43156, #21065, #26472, #14050, #4998, #41509, #8088, #1088, #29400, #37979, #12866, #36322, #9969, #27858, #10755, #33249, #41398, #41479, #364, #37901, #16402, #40678, #42548, #2107, #30554 ) ) ;
#23348 = LINE ( 'NONE', #29448, #33154 ) ;
#23350 = ORIENTED_EDGE ( 'NONE', *, *, #20424, .F. ) ;
#23349 = CIRCLE ( 'NONE', #39294, 2.649999999999999467 ) ;
#23351 = CARTESIAN_POINT ( 'NONE',  ( -105.9879088449591933, 17.11489954122026447, 4.119280070842334496 ) ) ;
#23352 = VERTEX_POINT ( 'NONE', #4619 ) ;
#23353 = VECTOR ( 'NONE', #24246, 1000.000000000000000 ) ;
#23354 = DIRECTION ( 'NONE',  ( 1.000000000000000000, -0.000000000000000000, -0.000000000000000000 ) ) ;
#23355 = DIRECTION ( 'NONE',  ( -0.000000000000000000, -0.000000000000000000, 1.000000000000000000 ) ) ;
#23356 = VERTEX_POINT ( 'NONE', #34300 ) ;
#23357 = FACE_OUTER_BOUND ( 'NONE', #9939, .T. ) ;
#23358 = AXIS2_PLACEMENT_3D ( 'NONE', #9958, #23308, #6690 ) ;
#23359 = FACE_OUTER_BOUND ( 'NONE', #32868, .T. ) ;
#23360 = DIRECTION ( 'NONE',  ( 0.000000000000000000, 0.000000000000000000, 1.000000000000000000 ) ) ;
#23361 = CARTESIAN_POINT ( 'NONE',  ( 55.63593431947571588, 31.00000000000000000, -48.80962981700470493 ) ) ;
#23362 = ORIENTED_EDGE ( 'NONE', *, *, #129, .T. ) ;
#23363 = CARTESIAN_POINT ( 'NONE',  ( 15.66220904948440662, 31.00000000000000355, -31.63873590539992264 ) ) ;
#23364 = CARTESIAN_POINT ( 'NONE',  ( -62.26029918285335896, 40.00000000000000711, 30.70375207684418228 ) ) ;
#23365 = EDGE_CURVE ( 'NONE', #16031, #36814, #12262, .T. ) ;
#23366 = CARTESIAN_POINT ( 'NONE',  ( 21.00000000000000355, 0.000000000000000000, 0.000000000000000000 ) ) ;
#23367 = DIRECTION ( 'NONE',  ( 1.000000000000000000, 0.000000000000000000, -6.546126324440847704E-16 ) ) ;
#23368 = EDGE_CURVE ( 'NONE', #37579, #8622, #22738, .T. ) ;
#23369 = AXIS2_PLACEMENT_3D ( 'NONE', #36882, #33400, #15990 ) ;
#23370 = VERTEX_POINT ( 'NONE', #34738 ) ;
#23371 = DIRECTION ( 'NONE',  ( 1.000000000000000000, 0.000000000000000000, 0.000000000000000000 ) ) ;
#23372 = CARTESIAN_POINT ( 'NONE',  ( 0.000000000000000000, 0.000000000000000000, 0.000000000000000000 ) ) ;
#23373 = VERTEX_POINT ( 'NONE', #1125 ) ;
#23374 = CARTESIAN_POINT ( 'NONE',  ( 55.10416666547021691, 40.00000000000000000, 3.599741573803287853 ) ) ;
#23375 = CARTESIAN_POINT ( 'NONE',  ( 0.000000000000000000, 0.000000000000000000, 0.000000000000000000 ) ) ;
#23376 = CARTESIAN_POINT ( 'NONE',  ( 4.000000000000000000, 0.9868501483902631932, -0.09357334158579604100 ) ) ;
#23377 = AXIS2_PLACEMENT_3D ( 'NONE', #35312, #2133, #31410 ) ;
#23378 = VERTEX_POINT ( 'NONE', #27555 ) ;
#23379 = DIRECTION ( 'NONE',  ( 0.000000000000000000, 0.000000000000000000, 1.000000000000000000 ) ) ;
#23380 = DIRECTION ( 'NONE',  ( -1.000000000000000000, -0.000000000000000000, -0.000000000000000000 ) ) ;
#23381 = AXIS2_PLACEMENT_3D ( 'NONE', #21303, #35195, #8580 ) ;
#23382 = VERTEX_POINT ( 'NONE', #28002 ) ;
#23383 = DIRECTION ( 'NONE',  ( 0.000000000000000000, 0.000000000000000000, -1.000000000000000000 ) ) ;
#23384 = ORIENTED_EDGE ( 'NONE', *, *, #37683, .T. ) ;
#23385 = CIRCLE ( 'NONE', #10854, 20.00000000000000711 ) ;
#23386 = ORIENTED_EDGE ( 'NONE', *, *, #26445, .F. ) ;
#23387 = LINE ( 'NONE', #23618, #3447 ) ;
#23388 = EDGE_CURVE ( 'NONE', #31096, #19076, #40815, .T. ) ;
#23389 = CARTESIAN_POINT ( 'NONE',  ( 96.17895579821514218, 31.00000000000000000, -12.55124642863780515 ) ) ;
#23390 = EDGE_LOOP ( 'NONE', ( #1921, #28203, #21850, #28497 ) ) ;
#23391 = DIRECTION ( 'NONE',  ( 1.000000000000000000, 0.000000000000000000, 0.000000000000000000 ) ) ;
#23392 = EDGE_CURVE ( 'NONE', #30637, #37240, #17866, .T. ) ;
#23393 = EDGE_CURVE ( 'NONE', #39340, #14569, #25522, .T. ) ;
#23394 = EDGE_CURVE ( 'NONE', #32776, #4344, #5304, .T. ) ;
#23395 = ADVANCED_FACE ( 'NONE', ( #31475 ), #23869, .F. ) ;
#23396 = CYLINDRICAL_SURFACE ( 'NONE', #42133, 59.00000000000000000 ) ;
#23397 = FACE_OUTER_BOUND ( 'NONE', #25652, .T. ) ;
#23398 = VERTEX_POINT ( 'NONE', #37132 ) ;
#23399 = CYLINDRICAL_SURFACE ( 'NONE', #3589, 59.00000000000000000 ) ;
#23400 = CIRCLE ( 'NONE', #4543, 10.99999999999999645 ) ;
#23401 = CARTESIAN_POINT ( 'NONE',  ( 0.000000000000000000, 0.000000000000000000, 9.999999999999998224 ) ) ;
#23403 = DIRECTION ( 'NONE',  ( -1.000000000000000000, -0.000000000000000000, -0.000000000000000000 ) ) ;
#23402 = LINE ( 'NONE', #36664, #25981 ) ;
#23404 = CARTESIAN_POINT ( 'NONE',  ( 17.99999999999999645, 0.000000000000000000, 0.000000000000000000 ) ) ;
#23405 = AXIS2_PLACEMENT_3D ( 'NONE', #6554, #9635, #22983 ) ;
#23406 = ORIENTED_EDGE ( 'NONE', *, *, #9929, .F. ) ;
#23407 = AXIS2_PLACEMENT_3D ( 'NONE', #22906, #2754, #18989 ) ;
#23408 = FILL_AREA_STYLE_COLOUR ( '', #22601 ) ;
#23409 = CARTESIAN_POINT ( 'NONE',  ( 24.60508655230852781, 31.00000000000000355, 6.583411914924224284 ) ) ;
#23410 = ORIENTED_EDGE ( 'NONE', *, *, #5858, .F. ) ;
#23411 = CIRCLE ( 'NONE', #42859, 0.08401999999999888724 ) ;
#23412 = CYLINDRICAL_SURFACE ( 'NONE', #38684, 120.5010000000000190 ) ;
#23413 = DIRECTION ( 'NONE',  ( -1.000000000000000000, 0.000000000000000000, 0.000000000000000000 ) ) ;
#23414 = VERTEX_POINT ( 'NONE', #14044 ) ;
#23415 = CIRCLE ( 'NONE', #26199, 4.250000000000000000 ) ;
#23416 = DIRECTION ( 'NONE',  ( -1.000000000000000000, -0.000000000000000000, -0.000000000000000000 ) ) ;
#23417 = CARTESIAN_POINT ( 'NONE',  ( -40.10416666498607441, 40.00000000000000000, -2.617993869485698344 ) ) ;
#23418 = CARTESIAN_POINT ( 'NONE',  ( 15.70068437845367093, 40.00000000000000000, 46.50252577712053892 ) ) ;
#23419 = VECTOR ( 'NONE', #40397, 1000.000000000000000 ) ;
#23420 = EDGE_CURVE ( 'NONE', #27122, #30306, #19940, .T. ) ;
#23421 = ORIENTED_EDGE ( 'NONE', *, *, #6081, .F. ) ;
#23422 = ORIENTED_EDGE ( 'NONE', *, *, #17580, .T. ) ;
#23423 = DIRECTION ( 'NONE',  ( 0.000000000000000000, 0.000000000000000000, 1.000000000000000000 ) ) ;
#23424 = DIRECTION ( 'NONE',  ( 0.000000000000000000, -0.8477344278896755680, 0.5304209081197351905 ) ) ;
#23425 = EDGE_CURVE ( 'NONE', #38690, #2973, #4570, .T. ) ;
#23426 = DIRECTION ( 'NONE',  ( -1.000000000000000000, 0.000000000000000000, 0.000000000000000000 ) ) ;
#23427 = EDGE_LOOP ( 'NONE', ( #10675, #35922, #11960, #18652 ) ) ;
#23428 = CARTESIAN_POINT ( 'NONE',  ( 0.000000000000000000, 104.0201923570375300, 51.34003878071097660 ) ) ;
#23429 = ORIENTED_EDGE ( 'NONE', *, *, #737, .T. ) ;
#23430 = CARTESIAN_POINT ( 'NONE',  ( 17.99999999999999645, -59.07817985939071548, 105.0250430397506847 ) ) ;
#23431 = DIRECTION ( 'NONE',  ( 0.000000000000000000, 0.000000000000000000, 1.000000000000000000 ) ) ;
#23432 =( REPRESENTATION_RELATIONSHIP ('NONE','NONE', #330, #37437 ) REPRESENTATION_RELATIONSHIP_WITH_TRANSFORMATION ( #41182 )SHAPE_REPRESENTATION_RELATIONSHIP( ) );
#23433 = ORIENTED_EDGE ( 'NONE', *, *, #27416, .T. ) ;
#23434 = AXIS2_PLACEMENT_3D ( 'NONE', #26929, #37590, #23890 ) ;
#23435 = CARTESIAN_POINT ( 'NONE',  ( -8.749793197483594298, -2.055254544495723756, 2.972870684497274762 ) ) ;
#23436 = DIRECTION ( 'NONE',  ( 0.000000000000000000, 0.8993121301712174720, 0.4373073204588591723 ) ) ;
#23437 = ORIENTED_EDGE ( 'NONE', *, *, #41178, .T. ) ;
#23438 = DIRECTION ( 'NONE',  ( 0.000000000000000000, 0.000000000000000000, 1.000000000000000000 ) ) ;
#23439 = ORIENTED_EDGE ( 'NONE', *, *, #2978, .F. ) ;
#23440 = AXIS2_PLACEMENT_3D ( 'NONE', #22075, #15317, #15726 ) ;
#23441 = DIRECTION ( 'NONE',  ( 1.000000000000000000, 0.000000000000000000, -0.000000000000000000 ) ) ;
#23442 = AXIS2_PLACEMENT_3D ( 'NONE', #18296, #17643, #7988 ) ;
#23443 = VERTEX_POINT ( 'NONE', #37780 ) ;
#23444 = CIRCLE ( 'NONE', #8094, 13.59999999999999787 ) ;
#23446 = ORIENTED_EDGE ( 'NONE', *, *, #21608, .F. ) ;
#23445 = DIRECTION ( 'NONE',  ( 0.000000000000000000, 0.9826841245925215240, -0.1852887240871114727 ) ) ;
#23447 = CARTESIAN_POINT ( 'NONE',  ( 28.99662776679064891, 31.00000000000000355, -58.58186007941694129 ) ) ;
#23448 = ORIENTED_EDGE ( 'NONE', *, *, #19512, .F. ) ;
#23449 = CARTESIAN_POINT ( 'NONE',  ( 0.000000000000000000, 120.3696465864706227, 5.624871700596487223 ) ) ;
#23450 = EDGE_CURVE ( 'NONE', #32776, #20249, #21488, .T. ) ;
#23451 = AXIS2_PLACEMENT_3D ( 'NONE', #30071, #19199, #39636 ) ;
#23452 = EDGE_CURVE ( 'NONE', #8111, #21090, #7682, .T. ) ;
#23453 = ADVANCED_FACE ( 'NONE', ( #4176 ), #17551, .F. ) ;
#23454 = CIRCLE ( 'NONE', #8101, 47.49900000000000233 ) ;
#23455 = EDGE_LOOP ( 'NONE', ( #18415, #10596, #22507, #9681 ) ) ;
#23456 = CARTESIAN_POINT ( 'NONE',  ( 0.000000000000000000, 41.33768078145642022, -104.3046912715537076 ) ) ;
#23457 = ADVANCED_FACE ( 'NONE', ( #38219 ), #36380, .T. ) ;
#23458 = AXIS2_PLACEMENT_3D ( 'NONE', #17506, #27513, #37952 ) ;
#23459 = ORIENTED_EDGE ( 'NONE', *, *, #4195, .T. ) ;
#23460 = CARTESIAN_POINT ( 'NONE',  ( 66.32976035609178211, 39.99999999999999289, 58.33333674018342663 ) ) ;
#23462 = DIRECTION ( 'NONE',  ( -1.000000000000000000, 0.000000000000000000, 0.000000000000000000 ) ) ;
#23461 = CARTESIAN_POINT ( 'NONE',  ( 18.00000000000000355, 0.000000000000000000, 0.000000000000000000 ) ) ;
#23463 = EDGE_CURVE ( 'NONE', #40767, #12187, #28438, .T. ) ;
#23464 = DIRECTION ( 'NONE',  ( 0.000000000000000000, -0.5877852522924624790, -0.8090169943749551118 ) ) ;
#23465 = VERTEX_POINT ( 'NONE', #29649 ) ;
#23466 = DIRECTION ( 'NONE',  ( 1.000000000000000000, 0.000000000000000000, 0.000000000000000000 ) ) ;
#23467 = VERTEX_POINT ( 'NONE', #1778 ) ;
#23468 = CARTESIAN_POINT ( 'NONE',  ( 18.00000000000000355, 34.03046037009303149, -33.13733193845768454 ) ) ;
#23469 = CARTESIAN_POINT ( 'NONE',  ( -59.40286837853895463, 31.00000000000000711, 52.11376356991771530 ) ) ;
#23471 = CARTESIAN_POINT ( 'NONE',  ( 1.287237434362044075, 3.875615274277557809, -3.430618716626812059 ) ) ;
#23470 = DIRECTION ( 'NONE',  ( 0.000000000000000000, 0.5877852522924685852, 0.8090169943749506709 ) ) ;
#23472 = AXIS2_PLACEMENT_3D ( 'NONE', #33105, #2335, #5847 ) ;
#23473 = VERTEX_POINT ( 'NONE', #32904 ) ;
#23474 = VECTOR ( 'NONE', #37257, 1000.000000000000000 ) ;
#23475 = AXIS2_PLACEMENT_3D ( 'NONE', #100, #26350, #26548 ) ;
#23476 = CIRCLE ( 'NONE', #33187, 1.999999999999998668 ) ;
#23477 = FACE_OUTER_BOUND ( 'NONE', #11657, .T. ) ;
#23478 = CIRCLE ( 'NONE', #4627, 116.0000000000000000 ) ;
#23479 = VERTEX_POINT ( 'NONE', #42929 ) ;
#23480 = CARTESIAN_POINT ( 'NONE',  ( 17.99999999999999645, 6.007673836298004666, 35.49518073029998533 ) ) ;
#23481 = DIRECTION ( 'NONE',  ( -1.000000000000000000, -0.000000000000000000, -0.000000000000000000 ) ) ;
#23482 = CARTESIAN_POINT ( 'NONE',  ( 0.000000000000000000, 0.000000000000000000, 0.000000000000000000 ) ) ;
#23483 = AXIS2_PLACEMENT_3D ( 'NONE', #4279, #13711, #27017 ) ;
#23484 = DIRECTION ( 'NONE',  ( -1.000000000000000000, -0.000000000000000000, -0.000000000000000000 ) ) ;
#23485 = EDGE_CURVE ( 'NONE', #21051, #4034, #16473, .T. ) ;
#23486 = VECTOR ( 'NONE', #5863, 1000.000000000000000 ) ;
#23487 = ORIENTED_EDGE ( 'NONE', *, *, #11207, .F. ) ;
#23488 = DIRECTION ( 'NONE',  ( -1.000000000000000000, -0.000000000000000000, 0.000000000000000000 ) ) ;
#23489 = ORIENTED_EDGE ( 'NONE', *, *, #35256, .F. ) ;
#23490 = CARTESIAN_POINT ( 'NONE',  ( 0.000000000000000000, 0.000000000000000000, -4.694516984716113228 ) ) ;
#23491 = CIRCLE ( 'NONE', #1149, 116.0000000000000000 ) ;
#23492 = CARTESIAN_POINT ( 'NONE',  ( 17.99999999999999645, 35.72777019205808813, -106.3569410558013715 ) ) ;
#23493 = FACE_OUTER_BOUND ( 'NONE', #24635, .T. ) ;
#23494 = ORIENTED_EDGE ( 'NONE', *, *, #401, .T. ) ;
#23495 = VERTEX_POINT ( 'NONE', #8335 ) ;
#23496 = CARTESIAN_POINT ( 'NONE',  ( -15.99999999999997691, 31.00000000000000355, 5.571627607371296764E-15 ) ) ;
#23497 = CARTESIAN_POINT ( 'NONE',  ( -10.00000000000000000, 0.000000000000000000, 0.000000000000000000 ) ) ;
#23498 = DIRECTION ( 'NONE',  ( 0.000000000000000000, 0.000000000000000000, 1.000000000000000000 ) ) ;
#23500 = VERTEX_POINT ( 'NONE', #41707 ) ;
#23499 = DIRECTION ( 'NONE',  ( -1.000000000000000000, 0.000000000000000000, 0.000000000000000000 ) ) ;
#23501 = CARTESIAN_POINT ( 'NONE',  ( 36.56095242095437925, 31.00000000000000355, -4.755136101395175174 ) ) ;
#23502 = DIRECTION ( 'NONE',  ( -1.000000000000000000, 0.000000000000000000, -0.000000000000000000 ) ) ;
#23503 = VECTOR ( 'NONE', #134, 1000.000000000000000 ) ;
#23504 = EDGE_CURVE ( 'NONE', #976, #235, #26204, .T. ) ;
#23506 = ORIENTED_EDGE ( 'NONE', *, *, #72, .F. ) ;
#23505 = DIRECTION ( 'NONE',  ( 0.000000000000000000, -0.6783118362696222148, 0.7347741508630616369 ) ) ;
#23507 = ORIENTED_EDGE ( 'NONE', *, *, #32876, .F. ) ;
#23508 = DIRECTION ( 'NONE',  ( -1.000000000000000000, 0.000000000000000000, 0.000000000000000000 ) ) ;
#23509 = CARTESIAN_POINT ( 'NONE',  ( 18.00000000000000355, -26.17370628620681927, 39.63700417846155233 ) ) ;
#23510 = CARTESIAN_POINT ( 'NONE',  ( -32.53655534684257589, 40.00000000000000000, -42.55839752837238166 ) ) ;
#23511 = VECTOR ( 'NONE', #21363, 1000.000000000000000 ) ;
#23512 = CARTESIAN_POINT ( 'NONE',  ( -10.00000000000000000, 0.000000000000000000, 0.000000000000000000 ) ) ;
#23513 = VECTOR ( 'NONE', #22169, 1000.000000000000000 ) ;
#23514 = CARTESIAN_POINT ( 'NONE',  ( -10.50000000000000178, 1.285879139104721028E-15, -1.199999999999999956 ) ) ;
#23515 = CARTESIAN_POINT ( 'NONE',  ( 0.000000000000000000, 40.13512380274121938, -113.6206972269517905 ) ) ;
#23516 = ORIENTED_EDGE ( 'NONE', *, *, #8965, .F. ) ;
#23517 = CARTESIAN_POINT ( 'NONE',  ( 17.99999999999999645, 75.72520367775197769, -82.78868281115903471 ) ) ;
#23518 = EDGE_CURVE ( 'NONE', #19147, #41661, #36170, .T. ) ;
#23520 = ORIENTED_EDGE ( 'NONE', *, *, #34653, .F. ) ;
#23519 = CONICAL_SURFACE ( 'NONE', #32546, 2.041999999999999815, 1.047197551196591858 ) ;
#23521 = CARTESIAN_POINT ( 'NONE',  ( 0.000000000000000000, 42.60732521687572927, 19.80331771201673519 ) ) ;
#23522 = DIRECTION ( 'NONE',  ( -1.000000000000000000, -0.000000000000000000, 0.000000000000000000 ) ) ;
#23523 = CIRCLE ( 'NONE', #40913, 20.00000000000000711 ) ;
#23524 = EDGE_CURVE ( 'NONE', #38496, #3709, #31065, .T. ) ;
#23525 = CARTESIAN_POINT ( 'NONE',  ( 12.21457428495364006, 31.00000000000000355, 45.57612047952555656 ) ) ;
#23526 = CARTESIAN_POINT ( 'NONE',  ( 18.00000000000000355, 15.49408907645234201, -44.90087086784576087 ) ) ;
#23527 = ORIENTED_EDGE ( 'NONE', *, *, #9472, .F. ) ;
#23528 = CARTESIAN_POINT ( 'NONE',  ( 18.00000000000000355, 27.43636312076376527, -38.14186064215121519 ) ) ;
#23529 = VERTEX_POINT ( 'NONE', #21692 ) ;
#23530 = CARTESIAN_POINT ( 'NONE',  ( 72.43982367323130234, 31.00000000000000000, 63.53091779346544143 ) ) ;
#23531 = ORIENTED_EDGE ( 'NONE', *, *, #15160, .F. ) ;
#23532 = CARTESIAN_POINT ( 'NONE',  ( 0.000000000000000000, 0.000000000000000000, 0.000000000000000000 ) ) ;
#23533 = AXIS2_PLACEMENT_3D ( 'NONE', #4442, #41536, #17813 ) ;
#23534 = CARTESIAN_POINT ( 'NONE',  ( -44.72205690102930475, 31.00000000000000355, -58.47036224961646411 ) ) ;
#23535 = CARTESIAN_POINT ( 'NONE',  ( -58.00742674161275403, 40.00000000000000711, -44.63796826977546317 ) ) ;
#23536 = DIRECTION ( 'NONE',  ( -1.000000000000000000, -0.000000000000000000, -0.000000000000000000 ) ) ;
#23537 = CIRCLE ( 'NONE', #20060, 59.00000000000000711 ) ;
#23538 = AXIS2_PLACEMENT_3D ( 'NONE', #39486, #42748, #3256 ) ;
#23539 = VERTEX_POINT ( 'NONE', #6285 ) ;
#23540 = ORIENTED_EDGE ( 'NONE', *, *, #39654, .T. ) ;
#23541 = DIRECTION ( 'NONE',  ( 0.000000000000000000, 0.4610925014493206242, 0.8873520750565743187 ) ) ;
#23542 = CIRCLE ( 'NONE', #41634, 58.99999999999998579 ) ;
#23543 = FACE_OUTER_BOUND ( 'NONE', #11410, .T. ) ;
#23544 = DIRECTION ( 'NONE',  ( -1.000000000000000000, -0.000000000000000000, -0.000000000000000000 ) ) ;
#23545 = AXIS2_PLACEMENT_3D ( 'NONE', #25848, #39310, #16027 ) ;
#23547 = VERTEX_POINT ( 'NONE', #34946 ) ;
#23546 = CARTESIAN_POINT ( 'NONE',  ( 0.000000000000000000, -105.3681574666266414, 38.54638589714855357 ) ) ;
#23548 = DIRECTION ( 'NONE',  ( -1.000000000000000000, 0.000000000000000000, -0.000000000000000000 ) ) ;
#23549 = ORIENTED_EDGE ( 'NONE', *, *, #18536, .T. ) ;
#23550 = CARTESIAN_POINT ( 'NONE',  ( 2.687328764639642653, -3.067272167851299969, -0.05923475698271395140 ) ) ;
#23551 = CARTESIAN_POINT ( 'NONE',  ( 81.87674480462379734, 39.99999999999999289, -21.93767060400471891 ) ) ;
#23552 = CARTESIAN_POINT ( 'NONE',  ( 17.99999999999999645, 99.97660604679964536, 67.26937820704921478 ) ) ;
#23553 = ORIENTED_EDGE ( 'NONE', *, *, #43021, .F. ) ;
#23554 = DIRECTION ( 'NONE',  ( -1.000000000000000000, -0.000000000000000000, 0.000000000000000000 ) ) ;
#23555 = DIRECTION ( 'NONE',  ( 0.000000000000000000, -1.000000000000000000, 5.297542245118643184E-16 ) ) ;
#23556 = EDGE_CURVE ( 'NONE', #39267, #32325, #14388, .T. ) ;
#23557 = ORIENTED_EDGE ( 'NONE', *, *, #21357, .F. ) ;
#23558 = ADVANCED_FACE ( 'NONE', ( #1563 ), #18417, .T. ) ;
#23559 = DIRECTION ( 'NONE',  ( 0.000000000000000000, -0.5528000653612000770, 0.8333139190825106235 ) ) ;
#23560 = ORIENTED_EDGE ( 'NONE', *, *, #28285, .F. ) ;
#23561 = FACE_OUTER_BOUND ( 'NONE', #22122, .T. ) ;
#23562 = EDGE_LOOP ( 'NONE', ( #15392, #8817, #29975, #1635 ) ) ;
#23563 = CARTESIAN_POINT ( 'NONE',  ( 20.65150112226537260, 40.00000000000000000, -15.81946110361252877 ) ) ;
#23564 = DIRECTION ( 'NONE',  ( -1.000000000000000000, -0.000000000000000000, -0.000000000000000000 ) ) ;
#23565 = DIRECTION ( 'NONE',  ( 0.000000000000000000, 0.000000000000000000, 1.000000000000000000 ) ) ;
#23566 = AXIS2_PLACEMENT_3D ( 'NONE', #6386, #3520, #3311 ) ;
#23567 = DIRECTION ( 'NONE',  ( -1.000000000000000000, 0.000000000000000000, 0.000000000000000000 ) ) ;
#23568 = DIRECTION ( 'NONE',  ( 0.000000000000000000, -9.408669700213191589E-16, -1.000000000000000000 ) ) ;
#23569 = ORIENTED_EDGE ( 'NONE', *, *, #7014, .T. ) ;
#23570 = VECTOR ( 'NONE', #620, 1000.000000000000000 ) ;
#23572 = CARTESIAN_POINT ( 'NONE',  ( 17.99999999999999645, -114.1529630473452386, 38.59523323561398200 ) ) ;
#23571 = DIRECTION ( 'NONE',  ( 0.000000000000000000, 0.000000000000000000, 1.000000000000000000 ) ) ;
#23573 = ADVANCED_FACE ( 'NONE', ( #2572 ), #15930, .T. ) ;
#23574 = ORIENTED_EDGE ( 'NONE', *, *, #12746, .F. ) ;
#23575 = AXIS2_PLACEMENT_3D ( 'NONE', #27757, #11163, #869 ) ;
#23576 = AXIS2_PLACEMENT_3D ( 'NONE', #8377, #18252, #8808 ) ;
#23577 = DIRECTION ( 'NONE',  ( 1.000000000000000000, 0.000000000000000000, 0.000000000000000000 ) ) ;
#23578 = ADVANCED_FACE ( 'NONE', ( #42496 ), #6490, .F. ) ;
#23579 = DIRECTION ( 'NONE',  ( -0.000000000000000000, -0.000000000000000000, -1.000000000000000000 ) ) ;
#23580 = ORIENTED_EDGE ( 'NONE', *, *, #926, .T. ) ;
#23581 = CARTESIAN_POINT ( 'NONE',  ( 18.00000000000000355, -30.03615769709703898, -42.44795908869020451 ) ) ;
#23582 = AXIS2_PLACEMENT_3D ( 'NONE', #22112, #38631, #8757 ) ;
#23583 = DIRECTION ( 'NONE',  ( 1.000000000000000000, 0.000000000000000000, 0.000000000000000000 ) ) ;
#23584 = ITEM_DEFINED_TRANSFORMATION ( 'NONE', 'NONE', #14235,  #13552 ) ;
#23585 = FACE_OUTER_BOUND ( 'NONE', #4181, .T. ) ;
#23586 = CARTESIAN_POINT ( 'NONE',  ( -54.82550897924149069, 31.00000000000000711, 42.06954809655981364 ) ) ;
#23587 = CIRCLE ( 'NONE', #18037, 20.00000000000000711 ) ;
#23588 = VERTEX_POINT ( 'NONE', #14910 ) ;
#23589 = CARTESIAN_POINT ( 'NONE',  ( -21.81649963859176822, 31.00000000000000355, -37.93159502954523532 ) ) ;
#23590 = CARTESIAN_POINT ( 'NONE',  ( 50.46169669344906339, 40.00000000000000000, 57.51940134901310131 ) ) ;
#23591 = EDGE_CURVE ( 'NONE', #8918, #25725, #40091, .T. ) ;
#23592 = ADVANCED_FACE ( 'NONE', ( #28213 ), #8543, .F. ) ;
#23593 = DIRECTION ( 'NONE',  ( 0.000000000000000000, 0.000000000000000000, 1.000000000000000000 ) ) ;
#23594 = CYLINDRICAL_SURFACE ( 'NONE', #27738, 120.5010000000000190 ) ;
#23595 = EDGE_CURVE ( 'NONE', #21901, #26484, #21361, .T. ) ;
#23596 = AXIS2_PLACEMENT_3D ( 'NONE', #14479, #37994, #898 ) ;
#23597 = AXIS2_PLACEMENT_3D ( 'NONE', #12482, #25373, #38851 ) ;
#23598 = ORIENTED_EDGE ( 'NONE', *, *, #36496, .F. ) ;
#23599 = DIRECTION ( 'NONE',  ( 1.000000000000000000, 0.000000000000000000, 0.000000000000000000 ) ) ;
#23600 = CARTESIAN_POINT ( 'NONE',  ( -3.510273485745307287, -2.827716139362669967, -3.610536846335890004 ) ) ;
#23601 = AXIS2_PLACEMENT_3D ( 'NONE', #35935, #32466, #6065 ) ;
#23602 = AXIS2_PLACEMENT_3D ( 'NONE', #2913, #12572, #36516 ) ;
#23603 = ORIENTED_EDGE ( 'NONE', *, *, #5601, .F. ) ;
#23604 = CARTESIAN_POINT ( 'NONE',  ( 48.77780477658175329, 40.00000000000000000, -24.05648398140741406 ) ) ;
#23605 = AXIS2_PLACEMENT_3D ( 'NONE', #36944, #499, #33023 ) ;
#23606 = DIRECTION ( 'NONE',  ( -1.000000000000000000, 0.000000000000000000, 0.000000000000000000 ) ) ;
#23607 = CARTESIAN_POINT ( 'NONE',  ( -5.991980000000000750, 0.000000000000000000, 15.08402000000000065 ) ) ;
#23608 = VECTOR ( 'NONE', #6815, 1000.000000000000000 ) ;
#23609 = ORIENTED_EDGE ( 'NONE', *, *, #4857, .T. ) ;
#23610 = DIRECTION ( 'NONE',  ( -1.000000000000000000, 0.000000000000000000, -0.000000000000000000 ) ) ;
#23611 = CIRCLE ( 'NONE', #17956, 129.9999999999993463 ) ;
#23612 = DIRECTION ( 'NONE',  ( 0.000000000000000000, 0.000000000000000000, 1.000000000000000000 ) ) ;
#23613 = ORIENTED_EDGE ( 'NONE', *, *, #36054, .T. ) ;
#23614 = FACE_OUTER_BOUND ( 'NONE', #27906, .T. ) ;
#23615 = ORIENTED_EDGE ( 'NONE', *, *, #2727, .F. ) ;
#23616 = EDGE_CURVE ( 'NONE', #24001, #23236, #19251, .T. ) ;
#23617 = VERTEX_POINT ( 'NONE', #36593 ) ;
#23618 = CARTESIAN_POINT ( 'NONE',  ( 126.0000000000000284, 1.589209405437102375E-14, 367.6955262170047263 ) ) ;
#23619 = CARTESIAN_POINT ( 'NONE',  ( 6.309545988805660421, 31.00000000000000355, -94.59213238968112591 ) ) ;
#23620 = EDGE_LOOP ( 'NONE', ( #14915, #22858, #3318, #27077 ) ) ;
#23621 = LINE ( 'NONE', #3268, #17560 ) ;
#23622 = DIRECTION ( 'NONE',  ( -1.000000000000000000, 0.000000000000000000, -0.000000000000000000 ) ) ;
#23623 = LINE ( 'NONE', #29494, #17852 ) ;
#23624 = ORIENTED_EDGE ( 'NONE', *, *, #10125, .F. ) ;
#23625 = CARTESIAN_POINT ( 'NONE',  ( -10.00000000000000000, 0.000000000000000000, 0.000000000000000000 ) ) ;
#23626 = EDGE_CURVE ( 'NONE', #10198, #27036, #13727, .T. ) ;
#23627 = LINE ( 'NONE', #652, #38733 ) ;
#23628 = EDGE_CURVE ( 'NONE', #23271, #31610, #27031, .T. ) ;
#23629 = CIRCLE ( 'NONE', #33346, 100.0000000000000000 ) ;
#23630 = VECTOR ( 'NONE', #41861, 1000.000000000000000 ) ;
#23632 = CARTESIAN_POINT ( 'NONE',  ( 17.99999999999999645, 31.11570115861502828, -4.898994019976315784 ) ) ;
#23631 = CARTESIAN_POINT ( 'NONE',  ( 17.99999999999999645, 5.492704054968225336, -115.8698847939555776 ) ) ;
#23633 = EDGE_CURVE ( 'NONE', #35327, #31991, #5975, .T. ) ;
#23634 = CARTESIAN_POINT ( 'NONE',  ( -5.991980000000000750, 0.000000000000000000, 0.000000000000000000 ) ) ;
#23635 = CIRCLE ( 'NONE', #16660, 59.00000000000000711 ) ;
#23636 = VERTEX_POINT ( 'NONE', #4073 ) ;
#23637 = DIRECTION ( 'NONE',  ( -1.659994950812537852E-17, -1.000000000000000000, -1.377814977426231881E-16 ) ) ;
#23638 = CARTESIAN_POINT ( 'NONE',  ( 19.15075862373047144, 31.00000000000000355, -38.85840887180553693 ) ) ;
#23639 = EDGE_LOOP ( 'NONE', ( #16801, #8329, #30742, #35970 ) ) ;
#23640 = CARTESIAN_POINT ( 'NONE',  ( 106.4195705685756792, -106.4195705685758213, 6.999999999999667821 ) ) ;
#23641 = DIRECTION ( 'NONE',  ( 1.000000000000000000, 0.000000000000000000, 0.000000000000000000 ) ) ;
#23642 = EDGE_LOOP ( 'NONE', ( #32856, #1142, #2520, #34005 ) ) ;
#23643 = DIRECTION ( 'NONE',  ( 0.000000000000000000, 0.9980267284282717810, -0.06279051952930990443 ) ) ;
#23644 = CARTESIAN_POINT ( 'NONE',  ( 39.77940265867437120, 40.00000000000000000, 22.96373720238702276 ) ) ;
#23645 = CARTESIAN_POINT ( 'NONE',  ( -11.35616125661516307, 40.00000000000000000, -42.69191301636733726 ) ) ;
#23646 = ORIENTED_EDGE ( 'NONE', *, *, #2182, .T. ) ;
#23647 = DIRECTION ( 'NONE',  ( 0.000000000000000000, 0.000000000000000000, 1.000000000000000000 ) ) ;
#23648 = CARTESIAN_POINT ( 'NONE',  ( 0.000000000000000000, 13.22719389142019608, -28.58720592780581882 ) ) ;
#23649 = EDGE_CURVE ( 'NONE', #42330, #38968, #10432, .T. ) ;
#23650 = PRODUCT_DEFINITION ( 'UNKNOWN', '', #12151, #17407 ) ;
#23651 = CARTESIAN_POINT ( 'NONE',  ( 6.908545562266867002, -12.05525454449572997, -74.83297477053821467 ) ) ;
#23652 = ORIENTED_EDGE ( 'NONE', *, *, #33877, .T. ) ;
#23653 = CARTESIAN_POINT ( 'NONE',  ( 24.89583333603155069, 40.00000000000000000, -1.636246165087041016 ) ) ;
#23654 = ORIENTED_EDGE ( 'NONE', *, *, #9986, .T. ) ;
#23655 = CARTESIAN_POINT ( 'NONE',  ( 18.00000000000000355, 0.000000000000000000, 0.000000000000000000 ) ) ;
#23656 = DIRECTION ( 'NONE',  ( -1.000000000000000000, 0.000000000000000000, -0.000000000000000000 ) ) ;
#23657 = ORIENTED_EDGE ( 'NONE', *, *, #12439, .T. ) ;
#23658 = AXIS2_PLACEMENT_3D ( 'NONE', #24805, #28058, #31531 ) ;
#23659 = VECTOR ( 'NONE', #8008, 1000.000000000000114 ) ;
#23660 = CARTESIAN_POINT ( 'NONE',  ( 8.999999999999998224, 104.0201923570382405, -51.34003878070954130 ) ) ;
#23661 = DIRECTION ( 'NONE',  ( 1.000000000000000000, 0.000000000000000000, 0.000000000000000000 ) ) ;
#23662 = EDGE_LOOP ( 'NONE', ( #584, #32799, #42336, #22165, #25860 ) ) ;
#23663 = CARTESIAN_POINT ( 'NONE',  ( 17.99999999999999645, 0.000000000000000000, 0.000000000000000000 ) ) ;
#23664 = ORIENTED_EDGE ( 'NONE', *, *, #25631, .F. ) ;
#23665 = AXIS2_PLACEMENT_3D ( 'NONE', #30818, #18412, #14246 ) ;
#23666 = CARTESIAN_POINT ( 'NONE',  ( 0.000000000000000000, 91.51415974874679193, -64.91094698989203948 ) ) ;
#23667 = EDGE_CURVE ( 'NONE', #31449, #11136, #7142, .T. ) ;
#23668 = VERTEX_POINT ( 'NONE', #20497 ) ;
#23670 = ORIENTED_EDGE ( 'NONE', *, *, #32169, .F. ) ;
#23669 = CARTESIAN_POINT ( 'NONE',  ( 2.500000000000000000, 2.357898499370431722, -2.818925648462311528E-15 ) ) ;
#23671 = CARTESIAN_POINT ( 'NONE',  ( -48.52617905695110068, 31.00000000000000355, 37.10499320822106029 ) ) ;
#23672 = EDGE_LOOP ( 'NONE', ( #31439, #23931 ) ) ;
#23673 = CARTESIAN_POINT ( 'NONE',  ( 18.00000000000000355, -15.49408907645141653, -44.90087086784608061 ) ) ;
#23674 = ORIENTED_EDGE ( 'NONE', *, *, #5886, .F. ) ;
#23675 = DIRECTION ( 'NONE',  ( -1.000000000000000000, 0.000000000000000000, 0.000000000000000000 ) ) ;
#23676 = EDGE_CURVE ( 'NONE', #28489, #637, #39412, .T. ) ;
#23677 = ORIENTED_EDGE ( 'NONE', *, *, #36760, .F. ) ;
#23678 = CARTESIAN_POINT ( 'NONE',  ( 53.86549405311984628, 40.00000000000000000, 70.40131829845091715 ) ) ;
#23679 = EDGE_CURVE ( 'NONE', #41527, #31337, #37337, .T. ) ;
#23681 = DIRECTION ( 'NONE',  ( 0.000000000000000000, -0.9048270524660145808, -0.4257792915650830956 ) ) ;
#23680 = DIRECTION ( 'NONE',  ( -1.770125995894701695E-16, 1.000000000000000000, 0.000000000000000000 ) ) ;
#23682 = DIRECTION ( 'NONE',  ( 1.000000000000000000, -0.000000000000000000, -0.000000000000000000 ) ) ;
#23683 = ORIENTED_EDGE ( 'NONE', *, *, #11798, .T. ) ;
#23684 = DIRECTION ( 'NONE',  ( -1.000000000000000000, 0.000000000000000000, -0.000000000000000000 ) ) ;
#23685 = ORIENTED_EDGE ( 'NONE', *, *, #26763, .T. ) ;
#23686 = AXIS2_PLACEMENT_3D ( 'NONE', #373, #33771, #43152 ) ;
#23687 = DIRECTION ( 'NONE',  ( 0.000000000000000000, 0.000000000000000000, 1.000000000000000000 ) ) ;
#23688 = CARTESIAN_POINT ( 'NONE',  ( 41.75688748258168914, 31.00000000000000355, -72.32308762158416471 ) ) ;
#23689 = DIRECTION ( 'NONE',  ( 0.000000000000000000, 0.000000000000000000, -1.000000000000000000 ) ) ;
#23690 = AXIS2_PLACEMENT_3D ( 'NONE', #32772, #26027, #29512 ) ;
#23691 = ORIENTED_EDGE ( 'NONE', *, *, #3610, .T. ) ;
#23692 = VECTOR ( 'NONE', #23606, 1000.000000000000000 ) ;
#23693 = DIRECTION ( 'NONE',  ( -1.000000000000000000, 0.000000000000000000, 0.000000000000000000 ) ) ;
#23694 = EDGE_CURVE ( 'NONE', #36592, #33164, #42900, .T. ) ;
#23695 = ORIENTED_EDGE ( 'NONE', *, *, #16829, .F. ) ;
#23696 = CARTESIAN_POINT ( 'NONE',  ( 18.00000000000000355, -17.50309955389642269, 43.60271849949357659 ) ) ;
#23697 = DIRECTION ( 'NONE',  ( -1.000000000000000000, 0.000000000000000000, 0.000000000000000000 ) ) ;
#23698 = EDGE_CURVE ( 'NONE', #31287, #20730, #3844, .T. ) ;
#23699 = CARTESIAN_POINT ( 'NONE',  ( -91.96080130434580724, -14.05525454449571043, 14.45886780445738218 ) ) ;
#23700 = ADVANCED_FACE ( 'NONE', ( #30291 ), #24207, .F. ) ;
#23701 = EDGE_CURVE ( 'NONE', #16968, #11045, #26799, .T. ) ;
#23702 = DIRECTION ( 'NONE',  ( 0.000000000000000000, 0.000000000000000000, 1.000000000000000000 ) ) ;
#23703 = ORIENTED_EDGE ( 'NONE', *, *, #37791, .F. ) ;
#23704 = CARTESIAN_POINT ( 'NONE',  ( 17.99999999999999645, -111.2721026680459602, -14.38025178762732104 ) ) ;
#23705 = VERTEX_POINT ( 'NONE', #13941 ) ;
#23706 = DIRECTION ( 'NONE',  ( -1.000000000000000000, -0.000000000000000000, 0.000000000000000000 ) ) ;
#23707 = DIRECTION ( 'NONE',  ( 1.000000000000000000, 0.000000000000000000, 0.000000000000000000 ) ) ;
#23708 = CARTESIAN_POINT ( 'NONE',  ( 9.000000000000001776, 17.77780072541854040, -114.6296200873374147 ) ) ;
#23709 = ORIENTED_EDGE ( 'NONE', *, *, #25362, .T. ) ;
#23710 = ORIENTED_EDGE ( 'NONE', *, *, #3548, .F. ) ;
#23711 = LINE ( 'NONE', #36974, #21748 ) ;
#23712 = DIRECTION ( 'NONE',  ( -1.000000000000000000, -0.000000000000000000, -0.000000000000000000 ) ) ;
#23713 = CARTESIAN_POINT ( 'NONE',  ( 3.999999999999998224, 2.472263674411418588, -3.687027874309861897 ) ) ;
#23714 = AXIS2_PLACEMENT_3D ( 'NONE', #39103, #9439, #42155 ) ;
#23716 = ORIENTED_EDGE ( 'NONE', *, *, #31312, .T. ) ;
#23715 = CYLINDRICAL_SURFACE ( 'NONE', #12495, 13.60000000000000142 ) ;
#23717 = AXIS2_PLACEMENT_3D ( 'NONE', #6909, #997, #36804 ) ;
#23718 = CARTESIAN_POINT ( 'NONE',  ( 36.89914868738900822, 31.00000000000000355, -2.354335741662294534 ) ) ;
#23719 = VECTOR ( 'NONE', #1078, 1000.000000000000000 ) ;
#23720 = CARTESIAN_POINT ( 'NONE',  ( 0.000000000000000000, 0.000000000000000000, 0.000000000000000000 ) ) ;
#23722 = ORIENTED_EDGE ( 'NONE', *, *, #16996, .T. ) ;
#23721 = DIRECTION ( 'NONE',  ( -1.000000000000000000, 0.000000000000000000, -0.000000000000000000 ) ) ;
#23723 = ORIENTED_EDGE ( 'NONE', *, *, #42433, .T. ) ;
#23724 = DIRECTION ( 'NONE',  ( 1.000000000000000000, 0.000000000000000000, 0.000000000000000000 ) ) ;
#23725 = DIRECTION ( 'NONE',  ( -1.000000000000000000, 0.000000000000000000, 0.000000000000000000 ) ) ;
#23726 = CARTESIAN_POINT ( 'NONE',  ( -48.87578956996785706, 40.00000000000000000, 16.50293044077288940 ) ) ;
#23727 = LINE ( 'NONE', #23514, #25678 ) ;
#23728 = CARTESIAN_POINT ( 'NONE',  ( -105.9879088449591933, 31.00000000000000355, 2.119280070842335384 ) ) ;
#23729 = EDGE_LOOP ( 'NONE', ( #6223, #15406, #7696, #23122 ) ) ;
#23730 = DIRECTION ( 'NONE',  ( -1.000000000000000000, -0.000000000000000000, -0.000000000000000000 ) ) ;
#23731 = ORIENTED_EDGE ( 'NONE', *, *, #34416, .T. ) ;
#23732 = CARTESIAN_POINT ( 'NONE',  ( -45.51113419504475388, -2.055254544495720648, 56.57887602028989704 ) ) ;
#23733 = CARTESIAN_POINT ( 'NONE',  ( 17.99999999999999645, -23.21237537461669120, -109.7700237000594541 ) ) ;
#23734 = CARTESIAN_POINT ( 'NONE',  ( -8.160545988181935328, 31.00000000000000355, -61.88879904071598048 ) ) ;
#23735 = DIRECTION ( 'NONE',  ( 1.000000000000000000, 0.000000000000000000, 0.000000000000000000 ) ) ;
#23736 = VERTEX_POINT ( 'NONE', #33987 ) ;
#23737 = CYLINDRICAL_SURFACE ( 'NONE', #19195, 51.99999999999999289 ) ;
#23738 = ORIENTED_EDGE ( 'NONE', *, *, #1659, .T. ) ;
#23739 = CARTESIAN_POINT ( 'NONE',  ( 94.59594211465898184, 31.00000000000000000, 12.45590092308117569 ) ) ;
#23740 = AXIS2_PLACEMENT_3D ( 'NONE', #5433, #31414, #32049 ) ;
#23741 = VECTOR ( 'NONE', #28061, 1000.000000000000000 ) ;
#23742 = EDGE_LOOP ( 'NONE', ( #33436, #930, #23429, #36520 ) ) ;
#23743 = CARTESIAN_POINT ( 'NONE',  ( 17.99999999999999645, 113.8630351447205697, 22.16324045874448601 ) ) ;
#23744 = CARTESIAN_POINT ( 'NONE',  ( 0.000000000000000000, 0.000000000000000000, -1.199999999999999956 ) ) ;
#23745 = CARTESIAN_POINT ( 'NONE',  ( -19.10382689932575673, 31.00000000000000355, -71.73905014346600240 ) ) ;
#23746 = CARTESIAN_POINT ( 'NONE',  ( -36.82253293460209420, 40.00000000000000000, -63.98115709648401150 ) ) ;
#23747 = EDGE_CURVE ( 'NONE', #508, #34279, #40119, .T. ) ;
#23748 = ADVANCED_FACE ( 'NONE', ( #40069 ), #20721, .T. ) ;
#23749 = VECTOR ( 'NONE', #842, 1000.000000000000000 ) ;
#23750 = CYLINDRICAL_SURFACE ( 'NONE', #27886, 59.00000000000000000 ) ;
#23751 = ADVANCED_FACE ( 'NONE', ( #29881 ), #40721, .F. ) ;
#23752 = ORIENTED_EDGE ( 'NONE', *, *, #2370, .T. ) ;
#23753 = LINE ( 'NONE', #37021, #11666 ) ;
#23754 = ORIENTED_EDGE ( 'NONE', *, *, #34461, .T. ) ;
#23755 = LINE ( 'NONE', #4061, #35313 ) ;
#23756 = CYLINDRICAL_SURFACE ( 'NONE', #21997, 31.49899999999999878 ) ;
#23758 = ORIENTED_EDGE ( 'NONE', *, *, #612, .T. ) ;
#23757 = CARTESIAN_POINT ( 'NONE',  ( 8.999999999999998224, 24.70533337038260413, -26.18485254986667243 ) ) ;
#23759 = DIRECTION ( 'NONE',  ( -1.000000000000000000, -0.000000000000000000, 0.000000000000000000 ) ) ;
#23760 = ORIENTED_EDGE ( 'NONE', *, *, #28656, .T. ) ;
#23761 = DIRECTION ( 'NONE',  ( -1.000000000000000000, 0.000000000000000000, 0.000000000000000000 ) ) ;
#23762 = CARTESIAN_POINT ( 'NONE',  ( 11.43299787627070607, 40.00000000000000000, 86.72764684403134083 ) ) ;
#23763 = DIRECTION ( 'NONE',  ( -1.000000000000000000, 0.000000000000000000, 0.000000000000000000 ) ) ;
#23764 = ORIENTED_EDGE ( 'NONE', *, *, #6426, .F. ) ;
#23765 = ADVANCED_FACE ( 'NONE', ( #3204 ), #16585, .F. ) ;
#23766 = DIRECTION ( 'NONE',  ( 0.1305261922200494362, 0.9914448613738107152, -0.000000000000000000 ) ) ;
#23767 = CARTESIAN_POINT ( 'NONE',  ( 17.99999999999999645, 0.000000000000000000, 0.000000000000000000 ) ) ;
#23768 = ORIENTED_EDGE ( 'NONE', *, *, #19612, .F. ) ;
#23769 = VECTOR ( 'NONE', #5613, 1000.000000000000000 ) ;
#23770 =( LENGTH_UNIT ( ) NAMED_UNIT ( * ) SI_UNIT ( .MILLI., .METRE. ) );
#23771 = ORIENTED_EDGE ( 'NONE', *, *, #33029, .F. ) ;
#23772 = DIRECTION ( 'NONE',  ( -1.000000000000000000, -0.000000000000000000, -0.000000000000000000 ) ) ;
#23774 = ORIENTED_EDGE ( 'NONE', *, *, #38620, .F. ) ;
#23773 = CIRCLE ( 'NONE', #16105, 120.5010000000000190 ) ;
#23775 = CARTESIAN_POINT ( 'NONE',  ( -17.43724119492421565, 40.00000000000000000, -15.29674861594511803 ) ) ;
#23776 = CARTESIAN_POINT ( 'NONE',  ( 18.00000000000000355, 46.21320724403648939, 10.97699764141968970 ) ) ;
#23777 = CIRCLE ( 'NONE', #9104, 58.99999999999999289 ) ;
#23778 = DIRECTION ( 'NONE',  ( 0.000000000000000000, -1.224646799147343346E-16, 1.000000000000000000 ) ) ;
#23779 = AXIS2_PLACEMENT_3D ( 'NONE', #20090, #10442, #16806 ) ;
#23780 = DIRECTION ( 'NONE',  ( 1.000000000000000000, 0.000000000000000000, 0.000000000000000000 ) ) ;
#23781 = CIRCLE ( 'NONE', #2122, 59.00000000000000000 ) ;
#23782 = EDGE_CURVE ( 'NONE', #41100, #15795, #39861, .T. ) ;
#23783 = DIRECTION ( 'NONE',  ( -1.000000000000000000, 0.000000000000000000, 0.000000000000000000 ) ) ;
#23784 = ORIENTED_EDGE ( 'NONE', *, *, #4982, .T. ) ;
#23786 = DIRECTION ( 'NONE',  ( 0.000000000000000000, 0.000000000000000000, 1.000000000000000000 ) ) ;
#23785 = DIRECTION ( 'NONE',  ( -1.000000000000000000, 0.000000000000000000, 0.000000000000000000 ) ) ;
#23787 = VERTEX_POINT ( 'NONE', #9985 ) ;
#23788 = CARTESIAN_POINT ( 'NONE',  ( 17.99999999999999645, 0.000000000000000000, 0.000000000000000000 ) ) ;
#23789 = CARTESIAN_POINT ( 'NONE',  ( -14.11622541012940601, 31.00000000000000355, -16.08312669853564358 ) ) ;
#23790 = ORIENTED_EDGE ( 'NONE', *, *, #26488, .T. ) ;
#23791 = DIRECTION ( 'NONE',  ( -1.000000000000000000, -0.000000000000000000, -0.000000000000000000 ) ) ;
#23792 = AXIS2_PLACEMENT_3D ( 'NONE', #16665, #19935, #10295 ) ;
#23793 = DIRECTION ( 'NONE',  ( 1.000000000000000000, -1.373900992973642263E-15, -3.996523416598957436E-16 ) ) ;
#23794 = LINE ( 'NONE', #16827, #37236 ) ;
#23795 = CARTESIAN_POINT ( 'NONE',  ( -60.02123122004734768, 31.00000000000000711, 34.66859033927303813 ) ) ;
#23796 = VERTEX_POINT ( 'NONE', #23335 ) ;
#23797 = CARTESIAN_POINT ( 'NONE',  ( -41.03896728213481992, 31.00000000000000355, -11.06873348903806864 ) ) ;
#23798 = EDGE_CURVE ( 'NONE', #10925, #25151, #35953, .T. ) ;
#23799 = CARTESIAN_POINT ( 'NONE',  ( 55.27058341129635721, 39.99999999999999289, -63.02248852588876105 ) ) ;
#23800 = AXIS2_PLACEMENT_3D ( 'NONE', #31762, #37848, #34155 ) ;
#23801 = AXIS2_PLACEMENT_3D ( 'NONE', #42406, #26065, #43047 ) ;
#23802 = CARTESIAN_POINT ( 'NONE',  ( 18.00000000000000355, 22.43957647427220081, -41.27978878573604504 ) ) ;
#23803 = AXIS2_PLACEMENT_3D ( 'NONE', #18216, #910, #18008 ) ;
#23804 = CARTESIAN_POINT ( 'NONE',  ( 17.99999999999999645, 0.000000000000000000, 0.000000000000000000 ) ) ;
#23805 = EDGE_CURVE ( 'NONE', #17354, #2165, #21376, .T. ) ;
#23806 = CIRCLE ( 'NONE', #22418, 59.00000000000000000 ) ;
#23807 = ORIENTED_EDGE ( 'NONE', *, *, #15826, .F. ) ;
#23808 = CYLINDRICAL_SURFACE ( 'NONE', #39963, 20.00000000000000355 ) ;
#23809 = CARTESIAN_POINT ( 'NONE',  ( 0.000000000000000000, 26.17370628620709638, -39.63700417846136048 ) ) ;
#23810 = EDGE_CURVE ( 'NONE', #10648, #34172, #5165, .T. ) ;
#23811 = ORIENTED_EDGE ( 'NONE', *, *, #21949, .T. ) ;
#23812 = CARTESIAN_POINT ( 'NONE',  ( -25.89845354150052259, 40.00000000000000000, -44.83417823681238445 ) ) ;
#23813 = CARTESIAN_POINT ( 'NONE',  ( 18.00000000000000355, -31.08872492059984793, 41.68322423723088832 ) ) ;
#23814 = CARTESIAN_POINT ( 'NONE',  ( 139.5000000000000000, 1.708382284810557841E-14, -20.00000000000000000 ) ) ;
#23815 = CIRCLE ( 'NONE', #27256, 58.99999999999999289 ) ;
#23816 = ORIENTED_EDGE ( 'NONE', *, *, #33627, .T. ) ;
#23817 = EDGE_CURVE ( 'NONE', #27469, #31476, #35053, .T. ) ;
#23818 = CARTESIAN_POINT ( 'NONE',  ( 17.99999999999999645, -0.6819280456820884240, -115.9979955608738607 ) ) ;
#23819 = CARTESIAN_POINT ( 'NONE',  ( 17.99999999999999645, 114.1157422997283248, 20.82300072952973480 ) ) ;
#23820 = ORIENTED_EDGE ( 'NONE', *, *, #10243, .F. ) ;
#23821 = CARTESIAN_POINT ( 'NONE',  ( -25.39999999999999147, 0.000000000000000000, 0.000000000000000000 ) ) ;
#23822 = ORIENTED_EDGE ( 'NONE', *, *, #14457, .F. ) ;
#23823 = CIRCLE ( 'NONE', #4987, 47.49900000000000233 ) ;
#23824 = DIRECTION ( 'NONE',  ( -1.000000000000000000, 0.000000000000000000, 0.000000000000000000 ) ) ;
#23825 = ORIENTED_EDGE ( 'NONE', *, *, #29246, .F. ) ;
#23826 = FACE_OUTER_BOUND ( 'NONE', #6306, .T. ) ;
#23827 = DIRECTION ( 'NONE',  ( 0.000000000000000000, 0.000000000000000000, 1.000000000000000000 ) ) ;
#23828 = VERTEX_POINT ( 'NONE', #14592 ) ;
#23829 = CARTESIAN_POINT ( 'NONE',  ( -17.77999999999999758, 0.000000000000000000, 0.000000000000000000 ) ) ;
#23830 = CARTESIAN_POINT ( 'NONE',  ( -31.75000000000000000, 0.000000000000000000, 0.000000000000000000 ) ) ;
#23831 = CARTESIAN_POINT ( 'NONE',  ( 9.000000000000001776, -104.6166166098442147, -50.11350645393781633 ) ) ;
#23832 = ORIENTED_EDGE ( 'NONE', *, *, #17519, .T. ) ;
#23833 = CARTESIAN_POINT ( 'NONE',  ( 17.99999999999999645, 0.000000000000000000, 0.000000000000000000 ) ) ;
#23835 = EDGE_CURVE ( 'NONE', #9577, #33598, #11613, .T. ) ;
#23834 = CIRCLE ( 'NONE', #61, 47.49900000000000233 ) ;
#23836 = AXIS2_PLACEMENT_3D ( 'NONE', #21816, #11529, #1462 ) ;
#23837 = CARTESIAN_POINT ( 'NONE',  ( 0.000000000000000000, 0.000000000000000000, 0.000000000000000000 ) ) ;
#23839 = CARTESIAN_POINT ( 'NONE',  ( 0.000000000000000000, 0.000000000000000000, 6.999999999999998224 ) ) ;
#23838 = FACE_OUTER_BOUND ( 'NONE', #4794, .T. ) ;
#23840 = CIRCLE ( 'NONE', #3565, 59.00000000000000000 ) ;
#23841 = DIRECTION ( 'NONE',  ( -1.000000000000000000, -0.000000000000000000, -0.000000000000000000 ) ) ;
#23842 = ORIENTED_EDGE ( 'NONE', *, *, #16267, .T. ) ;
#23843 = CARTESIAN_POINT ( 'NONE',  ( 106.4195705685763471, 1.999999999999996669, 106.4195705685744855 ) ) ;
#23844 = CARTESIAN_POINT ( 'NONE',  ( 17.99999999999999645, 24.70533337038223110, 26.18485254986702060 ) ) ;
#23845 = CARTESIAN_POINT ( 'NONE',  ( 39.78947517253659072, 31.00000000000000355, -19.62497191778171413 ) ) ;
#23846 = ORIENTED_EDGE ( 'NONE', *, *, #32720, .F. ) ;
#23847 = DIRECTION ( 'NONE',  ( 0.000000000000000000, 0.3140767120219495334, -0.9493976084683810601 ) ) ;
#23848 = CARTESIAN_POINT ( 'NONE',  ( 18.00000000000000355, 0.2227391519116599106, 46.98410307550730636 ) ) ;
#23849 = ORIENTED_EDGE ( 'NONE', *, *, #38942, .F. ) ;
#23850 = CARTESIAN_POINT ( 'NONE',  ( 17.99999999999999645, 52.19040376560434424, 99.31985817764196156 ) ) ;
#23851 = CARTESIAN_POINT ( 'NONE',  ( -6.851565232941113415, 40.00000000000000000, -51.95325991929587417 ) ) ;
#23852 = CARTESIAN_POINT ( 'NONE',  ( 41.62382930722196051, 40.00000000000000000, -20.43270582883756248 ) ) ;
#23853 = EDGE_LOOP ( 'NONE', ( #18266, #13982, #7521, #40919 ) ) ;
#23854 = CARTESIAN_POINT ( 'NONE',  ( 0.000000000000000000, -92.10690493017015967, -64.06707842432270184 ) ) ;
#23855 = CARTESIAN_POINT ( 'NONE',  ( 17.99999999999999645, 117.9424311864592312, -24.69967462998914698 ) ) ;
#23856 = FACE_OUTER_BOUND ( 'NONE', #8533, .T. ) ;
#23857 = EDGE_CURVE ( 'NONE', #18138, #3911, #40847, .T. ) ;
#23858 = VECTOR ( 'NONE', #15730, 1000.000000000000000 ) ;
#23859 = ORIENTED_EDGE ( 'NONE', *, *, #26345, .T. ) ;
#23860 = CARTESIAN_POINT ( 'NONE',  ( 7.411374251232441424, 40.00000000000000000, -21.84767871671174788 ) ) ;
#23861 = EDGE_LOOP ( 'NONE', ( #36028, #11143, #14784, #7119 ) ) ;
#23862 = DIRECTION ( 'NONE',  ( -1.000000000000000000, -0.000000000000000000, -0.000000000000000000 ) ) ;
#23863 = AXIS2_PLACEMENT_3D ( 'NONE', #24279, #18382, #31642 ) ;
#23864 = DIRECTION ( 'NONE',  ( 0.000000000000000000, 0.000000000000000000, 1.000000000000000000 ) ) ;
#23865 = CIRCLE ( 'NONE', #5025, 20.00000000000000355 ) ;
#23866 = ORIENTED_EDGE ( 'NONE', *, *, #23032, .F. ) ;
#23867 = DIRECTION ( 'NONE',  ( 1.000000000000000000, 0.000000000000000000, 0.000000000000000000 ) ) ;
#23868 = VECTOR ( 'NONE', #2983, 1000.000000000000000 ) ;
#23869 = CYLINDRICAL_SURFACE ( 'NONE', #22068, 59.00000000000000000 ) ;
#23870 = ADVANCED_FACE ( 'NONE', ( #38325 ), #8239, .T. ) ;
#23871 = ORIENTED_EDGE ( 'NONE', *, *, #24098, .F. ) ;
#23872 = DIRECTION ( 'NONE',  ( 0.000000000000000000, 0.7525707698561353576, 0.6585113790650422017 ) ) ;
#23873 = ORIENTED_EDGE ( 'NONE', *, *, #29230, .T. ) ;
#23874 = DIRECTION ( 'NONE',  ( -3.996523416598930318E-16, 2.658563593772947863E-15, 1.000000000000000000 ) ) ;
#23875 = CIRCLE ( 'NONE', #2207, 19.59999999999999432 ) ;
#23876 = ORIENTED_EDGE ( 'NONE', *, *, #40622, .F. ) ;
#23878 = ORIENTED_EDGE ( 'NONE', *, *, #35961, .T. ) ;
#23877 = DIRECTION ( 'NONE',  ( 1.000000000000000000, -1.373900992973641868E-15, -3.273063162220443081E-16 ) ) ;
#23879 = CARTESIAN_POINT ( 'NONE',  ( -45.90931453311223720, 31.00000000000000355, 40.13788153756826915 ) ) ;
#23880 = ORIENTED_EDGE ( 'NONE', *, *, #36111, .F. ) ;
#23881 = DIRECTION ( 'NONE',  ( 1.000000000000000000, 0.000000000000000000, 0.000000000000000000 ) ) ;
#23882 = ORIENTED_EDGE ( 'NONE', *, *, #8734, .F. ) ;
#23883 = DIRECTION ( 'NONE',  ( 1.000000000000000000, 0.000000000000000000, 0.000000000000000000 ) ) ;
#23884 = ORIENTED_EDGE ( 'NONE', *, *, #41226, .T. ) ;
#23885 = CARTESIAN_POINT ( 'NONE',  ( -81.27520743796613090, 40.00000000000000711, 10.59408403753070083 ) ) ;
#23886 = EDGE_CURVE ( 'NONE', #2740, #24215, #34844, .T. ) ;
#23887 = ADVANCED_FACE ( 'NONE', ( #4958 ), #34195, .T. ) ;
#23889 = CARTESIAN_POINT ( 'NONE',  ( 0.000000000000000000, 0.000000000000000000, 0.000000000000000000 ) ) ;
#23888 = CARTESIAN_POINT ( 'NONE',  ( 17.99999999999999645, -120.3696465864705800, -5.624871700597302571 ) ) ;
#23890 = DIRECTION ( 'NONE',  ( 0.000000000000000000, -0.8443279255020087470, -0.5358267949790065376 ) ) ;
#23891 = ORIENTED_EDGE ( 'NONE', *, *, #657, .T. ) ;
#23892 = DIRECTION ( 'NONE',  ( 1.000000000000000000, 0.000000000000000000, 0.000000000000000000 ) ) ;
#23893 = VERTEX_POINT ( 'NONE', #41153 ) ;
#23894 = SURFACE_STYLE_USAGE ( .BOTH. , #24552 ) ;
#23895 = CIRCLE ( 'NONE', #37804, 36.00000000000000000 ) ;
#23896 = DIRECTION ( 'NONE',  ( 0.000000000000000000, 0.4817536741017100499, 0.8763066800438663595 ) ) ;
#23897 = AXIS2_PLACEMENT_3D ( 'NONE', #2551, #39200, #23116 ) ;
#23898 = CARTESIAN_POINT ( 'NONE',  ( -85.90019077458921970, 31.00000000000000711, -29.16093118951848240 ) ) ;
#23899 = DIRECTION ( 'NONE',  ( 0.000000000000000000, 0.000000000000000000, -1.000000000000000000 ) ) ;
#23900 = ORIENTED_EDGE ( 'NONE', *, *, #12858, .T. ) ;
#23901 = AXIS2_PLACEMENT_3D ( 'NONE', #7799, #8241, #41154 ) ;
#23902 = CARTESIAN_POINT ( 'NONE',  ( -6.200000000000003730, 19.19999999999999929, 0.000000000000000000 ) ) ;
#23903 = EDGE_CURVE ( 'NONE', #30236, #8713, #18625, .T. ) ;
#23904 = AXIS2_PLACEMENT_3D ( 'NONE', #6789, #30793, #868 ) ;
#23905 = ORIENTED_EDGE ( 'NONE', *, *, #39250, .T. ) ;
#23906 = DIRECTION ( 'NONE',  ( -1.000000000000000000, 0.000000000000000000, -0.000000000000000000 ) ) ;
#23907 = CARTESIAN_POINT ( 'NONE',  ( 0.000000000000000000, 0.6505223195690489346, -51.99593080916756804 ) ) ;
#23908 = CARTESIAN_POINT ( 'NONE',  ( 17.99999999999999645, 84.09610293794069946, 74.27057253243037849 ) ) ;
#23909 = ADVANCED_FACE ( 'NONE', ( #14365 ), #28106, .T. ) ;
#23910 = VERTEX_POINT ( 'NONE', #18316 ) ;
#23911 = DIRECTION ( 'NONE',  ( 0.000000000000000000, 0.6736956436465584286, -0.7390089172206579793 ) ) ;
#23912 = ORIENTED_EDGE ( 'NONE', *, *, #35388, .F. ) ;
#23913 = CARTESIAN_POINT ( 'NONE',  ( 139.5000000000000000, 1.708382284810557841E-14, 9.999999999999998224 ) ) ;
#23914 = EDGE_CURVE ( 'NONE', #23636, #2185, #4290, .T. ) ;
#23915 = DIRECTION ( 'NONE',  ( 3.009274222672345096E-17, 1.000000000000000000, -2.455023325076454960E-18 ) ) ;
#23916 = CARTESIAN_POINT ( 'NONE',  ( 18.00000000000000355, -30.93515269692137792, 36.04401931830242489 ) ) ;
#23917 = EDGE_LOOP ( 'NONE', ( #14354, #11297, #24090, #35752 ) ) ;
#23918 = ORIENTED_EDGE ( 'NONE', *, *, #25156, .F. ) ;
#23919 = CARTESIAN_POINT ( 'NONE',  ( 17.99999999999999645, 23.79363200506992015, -27.01597816121622486 ) ) ;
#23920 = CARTESIAN_POINT ( 'NONE',  ( 0.000000000000000000, -112.8457601792513714, -26.86697618949492039 ) ) ;
#23921 = CIRCLE ( 'NONE', #5079, 59.00000000000000000 ) ;
#23922 = LINE ( 'NONE', #13668, #27856 ) ;
#23924 = ORIENTED_EDGE ( 'NONE', *, *, #18035, .F. ) ;
#23923 = LINE ( 'NONE', #10148, #15988 ) ;
#23925 = CARTESIAN_POINT ( 'NONE',  ( -16.82630558382797403, 31.00000000000000355, -29.24196894321154971 ) ) ;
#23926 = CARTESIAN_POINT ( 'NONE',  ( 2.250206802516407034, 117.9447454555042754, 2.972870684497274762 ) ) ;
#23927 = AXIS2_PLACEMENT_3D ( 'NONE', #24637, #37888, #13031 ) ;
#23928 =( GEOMETRIC_REPRESENTATION_CONTEXT ( 3 ) GLOBAL_UNCERTAINTY_ASSIGNED_CONTEXT ( ( #6302 ) ) GLOBAL_UNIT_ASSIGNED_CONTEXT ( ( #25879, #2263, #22198 ) ) REPRESENTATION_CONTEXT ( 'NONE', 'WORKASPACE' ) );
#23930 = VERTEX_POINT ( 'NONE', #7798 ) ;
#23929 = CARTESIAN_POINT ( 'NONE',  ( 0.000000000000000000, 0.000000000000000000, -4.000000000000000000 ) ) ;
#23931 = ORIENTED_EDGE ( 'NONE', *, *, #175, .T. ) ;
#23932 = CARTESIAN_POINT ( 'NONE',  ( 9.000000000000001776, 39.64889472655731595, 33.64468972902522381 ) ) ;
#23933 = CARTESIAN_POINT ( 'NONE',  ( -40.56882557769177566, 40.00000000000000000, 31.01417895415859505 ) ) ;
#23934 = EDGE_CURVE ( 'NONE', #8291, #26427, #41546, .T. ) ;
#23935 = ADVANCED_FACE ( 'NONE', ( #21807 ), #37677, .T. ) ;
#23936 = CARTESIAN_POINT ( 'NONE',  ( 9.000000000000001776, 58.30069736313799211, -100.2847380560561419 ) ) ;
#23937 = EDGE_CURVE ( 'NONE', #5066, #36133, #1838, .T. ) ;
#23938 = EDGE_CURVE ( 'NONE', #24620, #41098, #41602, .T. ) ;
#23940 = ADVANCED_FACE ( 'NONE', ( #25082 ), #31159, .T. ) ;
#23939 = UNCERTAINTY_MEASURE_WITH_UNIT (LENGTH_MEASURE( 1.000000000000000082E-05 ), #36668, 'distance_accuracy_value', 'NONE');
#23941 = CARTESIAN_POINT ( 'NONE',  ( 0.000000000000000000, -0.2227391519119825691, 46.98410307550729215 ) ) ;
#23942 = EDGE_LOOP ( 'NONE', ( #5286, #33600, #8869, #9683, #14793 ) ) ;
#23943 = DIRECTION ( 'NONE',  ( -1.000000000000000000, -0.000000000000000000, -0.000000000000000000 ) ) ;
#23944 = VERTEX_POINT ( 'NONE', #15879 ) ;
#23945 = CARTESIAN_POINT ( 'NONE',  ( 17.99999999999999645, 79.18387647320761857, 84.76976882518788159 ) ) ;
#23946 = FACE_OUTER_BOUND ( 'NONE', #38183, .T. ) ;
#23947 = CARTESIAN_POINT ( 'NONE',  ( -7.547223091130065953, 31.00000000000000355, 57.33767041057931380 ) ) ;
#23948 = CARTESIAN_POINT ( 'NONE',  ( 17.99999999999999645, 0.000000000000000000, 0.000000000000000000 ) ) ;
#23949 = ORIENTED_EDGE ( 'NONE', *, *, #34721, .F. ) ;
#23950 = CARTESIAN_POINT ( 'NONE',  ( -2.650000000000202860, 150.5000000000013642, 7.000000000000418332 ) ) ;
#23951 = VERTEX_POINT ( 'NONE', #9293 ) ;
#23952 = CIRCLE ( 'NONE', #7180, 19.19999999999999574 ) ;
#23953 = CARTESIAN_POINT ( 'NONE',  ( -6.381360069252544953, 31.00000000000000355, 97.60416666604666602 ) ) ;
#23954 = B_SPLINE_CURVE_WITH_KNOTS ( 'NONE', 3,
 ( #14356, #36809, #30073, #34392, #17652, #40287 ),
 .UNSPECIFIED., .F., .F.,
 ( 4, 2, 4 ),
 ( -3.640115492410698714E-06, 0.0002066546034006521879, 0.0004169493222937151081 ),
 .UNSPECIFIED. ) ;
#23955 = ORIENTED_EDGE ( 'NONE', *, *, #1246, .T. ) ;
#23956 = CARTESIAN_POINT ( 'NONE',  ( 17.99999999999999645, -31.11570115861491814, -4.898994019976963266 ) ) ;
#23957 = DIRECTION ( 'NONE',  ( -1.000000000000000000, 0.000000000000000000, 0.000000000000000000 ) ) ;
#23958 = CARTESIAN_POINT ( 'NONE',  ( -32.59403919554602425, 31.00000000000000355, -66.35267222981636337 ) ) ;
#23959 = CARTESIAN_POINT ( 'NONE',  ( 20.39742982868580157, 40.00000000000000000, 76.57971376067894198 ) ) ;
#23960 = CARTESIAN_POINT ( 'NONE',  ( 18.00000000000000355, 36.34385289850590794, 29.77717097092089205 ) ) ;
#23961 =( GEOMETRIC_REPRESENTATION_CONTEXT ( 3 ) GLOBAL_UNCERTAINTY_ASSIGNED_CONTEXT ( ( #19021 ) ) GLOBAL_UNIT_ASSIGNED_CONTEXT ( ( #4648, #1372, #3986 ) ) REPRESENTATION_CONTEXT ( 'NONE', 'WORKASPACE' ) );
#23962 = EDGE_CURVE ( 'NONE', #22707, #38985, #1741, .T. ) ;
#23963 = ORIENTED_EDGE ( 'NONE', *, *, #38291, .T. ) ;
#23964 = CARTESIAN_POINT ( 'NONE',  ( 18.00000000000000355, -47.49120266317495975, 0.8606222198173691940 ) ) ;
#23965 = ORIENTED_EDGE ( 'NONE', *, *, #42184, .F. ) ;
#23966 = CIRCLE ( 'NONE', #6477, 31.49899999999999878 ) ;
#23967 = LINE ( 'NONE', #17870, #33913 ) ;
#23968 = CYLINDRICAL_SURFACE ( 'NONE', #2457, 59.00000000000000000 ) ;
#23969 = EDGE_CURVE ( 'NONE', #31070, #28304, #7411, .T. ) ;
#23971 = VERTEX_POINT ( 'NONE', #2723 ) ;
#23970 = LINE ( 'NONE', #24196, #17183 ) ;
#23972 = DIRECTION ( 'NONE',  ( 0.000000000000000000, 0.9618256431728180456, 0.2736629900720866648 ) ) ;
#23973 = EDGE_CURVE ( 'NONE', #7856, #30129, #5337, .T. ) ;
#23974 = ORIENTED_EDGE ( 'NONE', *, *, #11617, .F. ) ;
#23975 = CARTESIAN_POINT ( 'NONE',  ( 17.99999999999999645, 21.56073507908678977, -23.57770962728541875 ) ) ;
#23976 = AXIS2_PLACEMENT_3D ( 'NONE', #33443, #23874, #16904 ) ;
#23977 = CARTESIAN_POINT ( 'NONE',  ( -66.93673649651354651, 40.00000000000000711, 58.72203107584222437 ) ) ;
#23978 = CARTESIAN_POINT ( 'NONE',  ( -2.000000000000006661, 3.464101615137750834, 0.000000000000000000 ) ) ;
#23979 = ORIENTED_EDGE ( 'NONE', *, *, #4676, .F. ) ;
#23980 = DIRECTION ( 'NONE',  ( -1.000000000000000000, 0.000000000000000000, -0.000000000000000000 ) ) ;
#23981 = CIRCLE ( 'NONE', #9303, 13.59999999999999964 ) ;
#23982 = DIRECTION ( 'NONE',  ( 0.000000000000000000, -0.7525707698561440173, 0.6585113790650322096 ) ) ;
#23983 = CIRCLE ( 'NONE', #37204, 51.99999999999999289 ) ;
#23984 = ORIENTED_EDGE ( 'NONE', *, *, #25061, .T. ) ;
#23985 = LINE ( 'NONE', #40304, #33735 ) ;
#23986 = AXIS2_PLACEMENT_3D ( 'NONE', #22105, #31254, #25367 ) ;
#23987 = ORIENTED_EDGE ( 'NONE', *, *, #38220, .F. ) ;
#23988 = DIRECTION ( 'NONE',  ( 1.000000000000000000, 0.000000000000000000, 0.000000000000000000 ) ) ;
#23989 = EDGE_LOOP ( 'NONE', ( #26662, #20771, #38271, #11726 ) ) ;
#23990 = CARTESIAN_POINT ( 'NONE',  ( -11.85532105537472880, 40.00000000000000000, -20.54123584193517260 ) ) ;
#23991 = LINE ( 'NONE', #27458, #5619 ) ;
#23992 = CARTESIAN_POINT ( 'NONE',  ( 17.99999999999999645, 0.000000000000000000, 0.000000000000000000 ) ) ;
#23993 = EDGE_CURVE ( 'NONE', #2012, #37721, #33200, .T. ) ;
#23994 = EDGE_CURVE ( 'NONE', #31505, #29860, #42349, .T. ) ;
#23995 = DIRECTION ( 'NONE',  ( 0.000000000000000000, -0.6783118362696075598, -0.7347741508630751817 ) ) ;
#23996 = ORIENTED_EDGE ( 'NONE', *, *, #37912, .F. ) ;
#23997 = EDGE_LOOP ( 'NONE', ( #40547, #23260, #6128, #33450, #35042, #22179, #12723, #30817, #4634, #23871, #28947, #15727, #7522, #29339, #5081, #39758, #40072, #36428, #7247, #29949, #20128, #23820, #15304, #42770, #22863, #25784, #18886, #7386, #24912, #16014, #13381, #34274, #9177, #21447, #28339, #6942, #27965, #8439, #18617, #23145, #27426, #29694, #37252, #936, #41730, #34193, #40579, #6511, #20396, #4780, #12617, #37771, #12852, #23771, #32237, #37066, #25732, #17611, #24138, #38090, #31424, #15754, #30986, #34506, #17156, #17433, #38494, #28074, #115, #23212, #37050, #39832, #33433, #35605, #22480, #38859, #35052, #9280, #40599, #19684, #840, #15488, #20650, #24543, #24410, #35583, #29351, #7691, #38030, #17552, #24528, #12537, #6062, #42807, #42414, #16281, #22267, #12980, #20402, #21344, #19954, #32587, #4250, #15603, #17639, #40410, #10121, #38931, #15212, #8940, #19207, #25438, #13605, #3806, #6303, #39743, #5208, #19192, #40353, #1461, #31532, #41152, #5378, #5851, #13403, #27050, #15253, #42778, #14503, #145, #20188, #42306, #15980, #30838, #27729, #30815, #26618, #42587, #12790, #6154, #37154, #5756, #18245, #28218, #32310, #16299, #38867, #1267, #1083, #35199, #28592, #30520, #4124, #19529, #25549, #20897, #25173, #1384, #12055, #19215, #38381, #27735, #32269, #9479, #33910, #38613, #13513, #29589, #27673, #35952, #7221, #10555, #13136, #12509, #34218, #21696, #16554, #25423, #33142, #14111, #13386, #16208, #38026, #32122, #13006, #38135, #37974, #7136, #22329, #5598, #31756, #15512, #3606, #11828, #11334, #3427, #5498, #40921, #36542, #32895, #36451, #6135, #36906, #6189, #5415, #35534, #7077, #25081, #40254, #33068, #29018, #17394, #29629, #5437, #28398, #22382, #39684, #32247, #27423, #2099, #18685, #13264, #19265, #5406, #34226, #1037, #42048, #10936, #10222, #21751, #14730, #18566, #37789, #33549, #33285, #22053, #12116, #33100, #14750, #21198, #42104, #39036, #27695, #29761, #36446, #40485, #20340, #30592, #34869, #17121, #3895, #30369, #22076, #21347, #12404, #9898, #16308, #4726, #1991, #23085, #19213, #1375, #20605, #5981, #17761, #39052, #29391, #40152, #34603, #25965, #43165, #26135, #10812, #41471, #16166, #38956, #41161, #36996, #15348, #14522, #26010, #29022, #36943, #1371, #36384, #17998, #15124, #36330, #9710, #6982, #1728, #5462, #28731, #2188, #27698, #10745, #13588, #24733, #23337, #17111, #10008, #41026, #41511, #41881, #31898, #13617, #21772, #9282, #1947, #30214, #23234, #20347, #1068, #15805, #16696, #41476, #465, #9477, #27383, #27277, #33119, #29924, #24121, #10051, #8316, #23760, #40943, #24985, #10226, #32560, #4171, #10695, #5516, #5873, #27160, #39696, #35401, #12195, #23918, #1648, #9383, #35130, #4903, #4127, #8961, #24417, #30975, #12716, #10897, #18199, #5621, #14018, #4852, #7597, #20756, #13997, #11816, #182, #38166, #3650, #28885, #36799, #36828, #11526, #17303, #22996, #10075, #27904, #29857, #35315, #2826, #18215, #29467, #16039, #28548, #24094, #38641, #17080, #1938, #9511, #35728, #43097, #8281, #7308, #24707, #14886, #27294, #25230, #23448, #40068, #34875, #18787, #29123, #9457, #16475, #21005, #24415, #5789, #29843, #42158, #15474, #17832, #5173, #25852, #24747, #31635, #14867, #39495, #348, #40134, #42580, #16522, #20164, #28916, #12009, #34358, #34329, #18994, #36914, #3167, #40470, #10800, #35831, #38115, #28121, #27013, #16013, #41574, #10579, #22871, #27870, #26908, #42886, #7343, #18490, #35255, #2620, #32951, #4384, #7367, #14571, #30335, #6151, #21404, #33842, #8300, #2422, #1522, #3714, #10438, #26541, #41916, #11460, #27377, #25326, #33125, #17421, #30712, #33233, #34741, #28278, #25267, #2294, #41959, #1687, #42857, #31378, #6041, #23738, #6371, #42282, #39120, #15067, #3398, #12778, #13215, #32887 ) ) ;
#23999 = DIRECTION ( 'NONE',  ( 0.000000000000000000, 0.7164567402983116340, 0.6976315211349882750 ) ) ;
#23998 = DIRECTION ( 'NONE',  ( 1.000000000000000000, 0.000000000000000000, 0.000000000000000000 ) ) ;
#24000 = EDGE_CURVE ( 'NONE', #8370, #19993, #14415, .T. ) ;
#24001 = VERTEX_POINT ( 'NONE', #41007 ) ;
#24002 = CIRCLE ( 'NONE', #17024, 59.00000000000001421 ) ;
#24003 = DIRECTION ( 'NONE',  ( -1.000000000000000000, -0.000000000000000000, -0.000000000000000000 ) ) ;
#24004 = CARTESIAN_POINT ( 'NONE',  ( -23.46968090759046888, 31.00000000000000355, -20.57717900685300449 ) ) ;
#24005 = ORIENTED_EDGE ( 'NONE', *, *, #37983, .T. ) ;
#24006 = CARTESIAN_POINT ( 'NONE',  ( 0.000000000000000000, 0.000000000000000000, 0.000000000000000000 ) ) ;
#24007 = CARTESIAN_POINT ( 'NONE',  ( -4.000000000000000000, -2.309401076758512694, -3.433295621305382461 ) ) ;
#24008 = CONTEXT_DEPENDENT_SHAPE_REPRESENTATION ( #17585, #6051 ) ;
#24009 = CYLINDRICAL_SURFACE ( 'NONE', #34405, 116.0000000000000000 ) ;
#24010 = CARTESIAN_POINT ( 'NONE',  ( 44.85399723358655422, 31.00000000000000355, -58.47732767552992073 ) ) ;
#24011 = AXIS2_PLACEMENT_3D ( 'NONE', #7283, #20644, #33915 ) ;
#24012 = EDGE_CURVE ( 'NONE', #22493, #41473, #26922, .T. ) ;
#24013 = VERTEX_POINT ( 'NONE', #34467 ) ;
#24014 = CARTESIAN_POINT ( 'NONE',  ( -22.33566874673848091, 31.00000000000000355, 45.10700316349001326 ) ) ;
#24015 = CIRCLE ( 'NONE', #19135, 20.00000000000000000 ) ;
#24016 = CARTESIAN_POINT ( 'NONE',  ( -59.40286837855683899, 40.00000000000000711, 52.11376356989983805 ) ) ;
#24017 = DIRECTION ( 'NONE',  ( 0.000000000000000000, 0.000000000000000000, 1.000000000000000000 ) ) ;
#24018 = DIRECTION ( 'NONE',  ( -1.000000000000000000, -0.000000000000000000, -0.000000000000000000 ) ) ;
#24019 = CARTESIAN_POINT ( 'NONE',  ( 17.99999999999999645, 0.000000000000000000, 0.000000000000000000 ) ) ;
#24021 = EDGE_LOOP ( 'NONE', ( #37010, #15200, #24648, #25317 ) ) ;
#24020 = CARTESIAN_POINT ( 'NONE',  ( 17.99999999999999645, 104.2166695095720854, -60.49278301857700768 ) ) ;
#24022 = LINE ( 'NONE', #17275, #21197 ) ;
#24023 = CARTESIAN_POINT ( 'NONE',  ( 17.99999999999999645, 0.000000000000000000, 0.000000000000000000 ) ) ;
#24024 = CIRCLE ( 'NONE', #41389, 31.49900000000000233 ) ;
#24025 = ORIENTED_EDGE ( 'NONE', *, *, #35990, .F. ) ;
#24026 = CARTESIAN_POINT ( 'NONE',  ( -38.74991464700507748, 40.00000000000000000, 44.18781823130588293 ) ) ;
#24027 = LINE ( 'NONE', #21429, #8252 ) ;
#24028 = COLOUR_RGB ( '', 0.08235294, 0.09019608, 0.10196078) ;
#24029 = CARTESIAN_POINT ( 'NONE',  ( 17.99999999999999645, -64.58410930313591791, 101.7319213743680422 ) ) ;
#24030 = ORIENTED_EDGE ( 'NONE', *, *, #22511, .T. ) ;
#24031 = CARTESIAN_POINT ( 'NONE',  ( 17.99999999999999645, 0.000000000000000000, 0.000000000000000000 ) ) ;
#24032 = CARTESIAN_POINT ( 'NONE',  ( -10.00000000000000000, 0.000000000000000000, 0.000000000000000000 ) ) ;
#24033 = ORIENTED_EDGE ( 'NONE', *, *, #13707, .F. ) ;
#24034 = CARTESIAN_POINT ( 'NONE',  ( 17.99999999999999645, -35.78425302087541837, 3.935382540232670312 ) ) ;
#24035 = ORIENTED_EDGE ( 'NONE', *, *, #15713, .T. ) ;
#24036 = CIRCLE ( 'NONE', #7264, 116.0000000000000000 ) ;
#24037 = CIRCLE ( 'NONE', #37918, 4.500000000000000888 ) ;
#24038 = DIRECTION ( 'NONE',  ( 0.000000000000000000, -0.6845471059286952764, 0.7289686274214055572 ) ) ;
#24039 = ORIENTED_EDGE ( 'NONE', *, *, #18345, .T. ) ;
#24040 = CIRCLE ( 'NONE', #11508, 116.0000000000000000 ) ;
#24041 = CARTESIAN_POINT ( 'NONE',  ( 8.999999999999998224, 0.000000000000000000, -13.40000000000000213 ) ) ;
#24042 = CARTESIAN_POINT ( 'NONE',  ( -132.0000507999999968, 0.000000000000000000, 0.000000000000000000 ) ) ;
#24043 = ORIENTED_EDGE ( 'NONE', *, *, #7349, .T. ) ;
#24044 = CARTESIAN_POINT ( 'NONE',  ( 0.000000000000000000, 0.000000000000000000, 0.000000000000000000 ) ) ;
#24045 = EDGE_CURVE ( 'NONE', #32420, #22146, #642, .T. ) ;
#24046 = CARTESIAN_POINT ( 'NONE',  ( -31.75000000000000000, 0.000000000000000000, 0.000000000000000000 ) ) ;
#24047 = ORIENTED_EDGE ( 'NONE', *, *, #736, .T. ) ;
#24048 = DIRECTION ( 'NONE',  ( 1.000000000000000000, 0.000000000000000000, 0.000000000000000000 ) ) ;
#24049 = CIRCLE ( 'NONE', #21266, 20.00000000000000711 ) ;
#24050 = DIRECTION ( 'NONE',  ( -1.000000000000000000, 0.000000000000000000, 0.000000000000000000 ) ) ;
#24051 = DIRECTION ( 'NONE',  ( 0.000000000000000000, -1.224646799147343346E-16, 1.000000000000000000 ) ) ;
#24052 = DIRECTION ( 'NONE',  ( -1.000000000000000000, 0.000000000000000000, -0.000000000000000000 ) ) ;
#24053 = VERTEX_POINT ( 'NONE', #13999 ) ;
#24054 = EDGE_CURVE ( 'NONE', #13970, #23910, #19977, .T. ) ;
#24056 = VECTOR ( 'NONE', #19765, 1000.000000000000000 ) ;
#24055 = CARTESIAN_POINT ( 'NONE',  ( -83.76341667917203893, 1.657770380241494775E-26, 6.300002081858475655 ) ) ;
#24057 = DIRECTION ( 'NONE',  ( 0.000000000000000000, -6.938893903907226800E-15, 1.000000000000000000 ) ) ;
#24058 = CARTESIAN_POINT ( 'NONE',  ( 9.621748599878955588, 31.00000000000000355, 35.89595399306684698 ) ) ;
#24059 = ORIENTED_EDGE ( 'NONE', *, *, #23082, .F. ) ;
#24060 = DIRECTION ( 'NONE',  ( 0.000000000000000000, -0.8951632913550664483, 0.4457383557765300930 ) ) ;
#24061 = EDGE_CURVE ( 'NONE', #41239, #37517, #25550, .T. ) ;
#24062 = CARTESIAN_POINT ( 'NONE',  ( 0.000000000000000000, 0.000000000000000000, 0.000000000000000000 ) ) ;
#24063 = VERTEX_POINT ( 'NONE', #4806 ) ;
#24064 = VECTOR ( 'NONE', #38067, 1000.000000000000000 ) ;
#24065 = DIRECTION ( 'NONE',  ( 0.000000000000000000, 0.000000000000000000, 1.000000000000000000 ) ) ;
#24066 = CARTESIAN_POINT ( 'NONE',  ( 3.436116956419347002, 40.00000000000000000, -52.60416666537189911 ) ) ;
#24067 = AXIS2_PLACEMENT_3D ( 'NONE', #8135, #3588, #30244 ) ;
#24068 = CARTESIAN_POINT ( 'NONE',  ( -62.09442273004785307, 40.00000000000000711, -4.163950221635984938 ) ) ;
#24069 = AXIS2_PLACEMENT_3D ( 'NONE', #10655, #40311, #7374 ) ;
#24070 = CIRCLE ( 'NONE', #5228, 51.99999999999999289 ) ;
#24071 = DIRECTION ( 'NONE',  ( 0.000000000000000000, 0.000000000000000000, 1.000000000000000000 ) ) ;
#24072 = LINE ( 'NONE', #17981, #5387 ) ;
#24073 = AXIS2_PLACEMENT_3D ( 'NONE', #26563, #30901, #14129 ) ;
#24074 = CARTESIAN_POINT ( 'NONE',  ( 17.99999999999999645, 0.000000000000000000, 0.000000000000000000 ) ) ;
#24075 = CYLINDRICAL_SURFACE ( 'NONE', #13424, 116.0000000000000000 ) ;
#24076 = CIRCLE ( 'NONE', #27547, 116.0000000000000000 ) ;
#24077 = ORIENTED_EDGE ( 'NONE', *, *, #4522, .T. ) ;
#24078 = CARTESIAN_POINT ( 'NONE',  ( -9.022452542771789652, 40.00000000000000000, 26.59230923919664491 ) ) ;
#24079 = ORIENTED_EDGE ( 'NONE', *, *, #32316, .T. ) ;
#24080 = DIRECTION ( 'NONE',  ( 0.000000000000000000, 0.000000000000000000, 1.000000000000000000 ) ) ;
#24081 = ADVANCED_FACE ( 'NONE', ( #10703 ), #7639, .T. ) ;
#24082 = CYLINDRICAL_SURFACE ( 'NONE', #27748, 59.00000000000000000 ) ;
#24083 = ORIENTED_EDGE ( 'NONE', *, *, #27982, .F. ) ;
#24084 = CYLINDRICAL_SURFACE ( 'NONE', #29847, 59.00000000000000000 ) ;
#24085 = CARTESIAN_POINT ( 'NONE',  ( 4.858130855304160865E-15, 5.778671572660278980E-15, 2.000000000000001776 ) ) ;
#24086 = ORIENTED_EDGE ( 'NONE', *, *, #904, .T. ) ;
#24087 = DIRECTION ( 'NONE',  ( 0.000000000000000000, 1.000000000000000000, 0.000000000000000000 ) ) ;
#24088 = ORIENTED_EDGE ( 'NONE', *, *, #19160, .T. ) ;
#24089 = DIRECTION ( 'NONE',  ( 0.000000000000000000, 0.000000000000000000, -1.000000000000000000 ) ) ;
#24090 = ORIENTED_EDGE ( 'NONE', *, *, #24737, .T. ) ;
#24092 = ORIENTED_EDGE ( 'NONE', *, *, #37073, .T. ) ;
#24091 = PLANE ( 'NONE',  #16017 ) ;
#24093 = CARTESIAN_POINT ( 'NONE',  ( 68.60033760563639760, 31.00000000000000000, -33.70054013428169526 ) ) ;
#24094 = ORIENTED_EDGE ( 'NONE', *, *, #8134, .F. ) ;
#24095 = DIRECTION ( 'NONE',  ( -1.000000000000000000, 0.000000000000000000, 0.000000000000000000 ) ) ;
#24096 = AXIS2_PLACEMENT_3D ( 'NONE', #24044, #13799, #27092 ) ;
#24097 = AXIS2_PLACEMENT_3D ( 'NONE', #33828, #30584, #40788 ) ;
#24098 = EDGE_CURVE ( 'NONE', #2567, #17290, #8105, .T. ) ;
#24099 = EDGE_LOOP ( 'NONE', ( #29033, #2442, #15031, #24035 ) ) ;
#24100 = AXIS2_PLACEMENT_3D ( 'NONE', #4372, #17745, #21029 ) ;
#24101 = LINE ( 'NONE', #40199, #13330 ) ;
#24102 = ORIENTED_EDGE ( 'NONE', *, *, #25839, .F. ) ;
#24103 = CARTESIAN_POINT ( 'NONE',  ( -46.83686391397709770, 40.00000000000000000, -81.34213072392142863 ) ) ;
#24104 = VECTOR ( 'NONE', #11543, 1000.000000000000000 ) ;
#24106 = CARTESIAN_POINT ( 'NONE',  ( 17.99999999999999645, 68.61497464550731706, -99.05794392877534449 ) ) ;
#24105 = CYLINDRICAL_SURFACE ( 'NONE', #16876, 120.5010000000000190 ) ;
#24107 = AXIS2_PLACEMENT_3D ( 'NONE', #22624, #29363, #9491 ) ;
#24108 = DIRECTION ( 'NONE',  ( 0.000000000000000000, 0.000000000000000000, 1.000000000000000000 ) ) ;
#24109 = FACE_OUTER_BOUND ( 'NONE', #594, .T. ) ;
#24110 = ORIENTED_EDGE ( 'NONE', *, *, #29946, .T. ) ;
#24111 = EDGE_CURVE ( 'NONE', #606, #23443, #1079, .T. ) ;
#24112 = CARTESIAN_POINT ( 'NONE',  ( 0.000000000000000000, 22.82995208772746665, -41.06517797613638976 ) ) ;
#24113 = DIRECTION ( 'NONE',  ( -1.000000000000000000, 0.000000000000000000, 0.000000000000000000 ) ) ;
#24114 = ADVANCED_FACE ( 'NONE', ( #27746 ), #7426, .F. ) ;
#24115 = CARTESIAN_POINT ( 'NONE',  ( 82.68608547523962216, 31.00000000000000000, 22.14036602612658200 ) ) ;
#24116 = CARTESIAN_POINT ( 'NONE',  ( 17.99999999999999645, 19.47322409167312429, -30.27859877001380084 ) ) ;
#24117 = ORIENTED_EDGE ( 'NONE', *, *, #4828, .F. ) ;
#24118 = EDGE_CURVE ( 'NONE', #26052, #29277, #410, .T. ) ;
#24119 = CARTESIAN_POINT ( 'NONE',  ( 9.000000000000001776, 13.00789606333472470, 115.2683592318615382 ) ) ;
#24120 = VERTEX_POINT ( 'NONE', #20789 ) ;
#24121 = ORIENTED_EDGE ( 'NONE', *, *, #32267, .F. ) ;
#24122 = DIRECTION ( 'NONE',  ( 0.000000000000000000, 0.000000000000000000, 1.000000000000000000 ) ) ;
#24123 = DIRECTION ( 'NONE',  ( 1.000000000000000000, 0.000000000000000000, 0.000000000000000000 ) ) ;
#24125 = LINE ( 'NONE', #34126, #16431 ) ;
#24124 = AXIS2_PLACEMENT_3D ( 'NONE', #38656, #25399, #18020 ) ;
#24126 = CARTESIAN_POINT ( 'NONE',  ( 0.000000000000000000, -111.8797445107944100, -8.437727291343872338 ) ) ;
#24127 = CIRCLE ( 'NONE', #29685, 19.99999999999999289 ) ;
#24128 = VERTEX_POINT ( 'NONE', #37093 ) ;
#24129 = FACE_OUTER_BOUND ( 'NONE', #13852, .T. ) ;
#24130 = ORIENTED_EDGE ( 'NONE', *, *, #27957, .F. ) ;
#24131 = ADVANCED_FACE ( 'NONE', ( #37735 ), #7196, .F. ) ;
#24132 = LINE ( 'NONE', #23913, #27713 ) ;
#24133 = ADVANCED_FACE ( 'NONE', ( #2579 ), #35114, .F. ) ;
#24134 = DIRECTION ( 'NONE',  ( -3.996523416598930318E-16, 2.658563593772947863E-15, 1.000000000000000000 ) ) ;
#24135 = AXIS2_PLACEMENT_3D ( 'NONE', #37746, #1315, #24702 ) ;
#24136 = CARTESIAN_POINT ( 'NONE',  ( 0.000000000000000000, -21.56073507908629594, -23.57770962728587705 ) ) ;
#24137 = ORIENTED_EDGE ( 'NONE', *, *, #30353, .F. ) ;
#24138 = ORIENTED_EDGE ( 'NONE', *, *, #9814, .F. ) ;
#24139 = CARTESIAN_POINT ( 'NONE',  ( 17.99999999999999645, 0.000000000000000000, 0.000000000000000000 ) ) ;
#24140 = DIRECTION ( 'NONE',  ( 3.996523416598930318E-16, -2.658563593772947863E-15, -1.000000000000000000 ) ) ;
#24141 = AXIS2_PLACEMENT_3D ( 'NONE', #10530, #17997, #31263 ) ;
#24142 = CARTESIAN_POINT ( 'NONE',  ( 17.99999999999999645, 0.000000000000000000, 0.000000000000000000 ) ) ;
#24143 = ORIENTED_EDGE ( 'NONE', *, *, #42715, .T. ) ;
#24145 = ORIENTED_EDGE ( 'NONE', *, *, #32909, .F. ) ;
#24144 = DIRECTION ( 'NONE',  ( -3.996523416598930318E-16, 2.658563593772947863E-15, 1.000000000000000000 ) ) ;
#24146 = ADVANCED_FACE ( 'NONE', ( #41667 ), #32071, .T. ) ;
#24147 = CARTESIAN_POINT ( 'NONE',  ( 38.14553738579559905, 31.00000000000000355, 29.36968266378863746 ) ) ;
#24148 = CARTESIAN_POINT ( 'NONE',  ( -105.3367680159044966, 17.11489954122026447, 2.032994142711228136 ) ) ;
#24149 = EDGE_CURVE ( 'NONE', #38578, #31578, #38088, .T. ) ;
#24151 = ORIENTED_EDGE ( 'NONE', *, *, #40266, .F. ) ;
#24150 = CARTESIAN_POINT ( 'NONE',  ( 17.99999999999999645, 0.000000000000000000, 0.000000000000000000 ) ) ;
#24152 = ORIENTED_EDGE ( 'NONE', *, *, #15129, .F. ) ;
#24153 = CARTESIAN_POINT ( 'NONE',  ( 4.211140560182196957, -2.431303136016555122, -3.745885042887436622 ) ) ;
#24154 = CARTESIAN_POINT ( 'NONE',  ( 7.664524495375378166, 40.00000000000000000, 58.91906827748253050 ) ) ;
#24155 = CIRCLE ( 'NONE', #28333, 58.99999999999998579 ) ;
#24156 = DIRECTION ( 'NONE',  ( 0.000000000000000000, 0.000000000000000000, 1.000000000000000000 ) ) ;
#24157 = CIRCLE ( 'NONE', #15800, 59.00000000000000000 ) ;
#24158 = DIRECTION ( 'NONE',  ( 1.000000000000000000, -0.000000000000000000, -0.000000000000000000 ) ) ;
#24160 = ORIENTED_EDGE ( 'NONE', *, *, #24667, .T. ) ;
#24159 = CIRCLE ( 'NONE', #5320, 59.00000000000000711 ) ;
#24161 = CARTESIAN_POINT ( 'NONE',  ( 9.000000000000001776, -115.5737863835461496, -9.934782381634844839 ) ) ;
#24162 = AXIS2_PLACEMENT_3D ( 'NONE', #31557, #1650, #14346 ) ;
#24163 = ORIENTED_EDGE ( 'NONE', *, *, #6612, .F. ) ;
#24164 = EDGE_CURVE ( 'NONE', #2864, #21604, #25343, .T. ) ;
#24165 = AXIS2_PLACEMENT_3D ( 'NONE', #26462, #9860, #32778 ) ;
#24166 = CARTESIAN_POINT ( 'NONE',  ( 0.000000000000000000, 0.000000000000000000, 0.000000000000000000 ) ) ;
#24167 = CARTESIAN_POINT ( 'NONE',  ( 17.99999999999999645, -115.5737863835461496, -9.934782381634859050 ) ) ;
#24168 = AXIS2_PLACEMENT_3D ( 'NONE', #32968, #28865, #2412 ) ;
#24169 = EDGE_CURVE ( 'NONE', #31896, #4351, #2352, .T. ) ;
#24170 = CARTESIAN_POINT ( 'NONE',  ( 53.64558601427197004, 31.00000000000000355, 14.36188897069615500 ) ) ;
#24171 = CARTESIAN_POINT ( 'NONE',  ( 58.80287614962789888, -14.05525454449572109, 69.29271901957253021 ) ) ;
#24173 = ORIENTED_EDGE ( 'NONE', *, *, #18243, .T. ) ;
#24172 = AXIS2_PLACEMENT_3D ( 'NONE', #40980, #7832, #10912 ) ;
#24174 = EDGE_CURVE ( 'NONE', #29749, #18043, #11813, .T. ) ;
#24176 = AXIS2_PLACEMENT_3D ( 'NONE', #18530, #27899, #14807 ) ;
#24175 = CARTESIAN_POINT ( 'NONE',  ( 0.000000000000000000, -34.78944633786284868, 9.257128253673496232 ) ) ;
#24177 = VERTEX_POINT ( 'NONE', #34909 ) ;
#24178 = CARTESIAN_POINT ( 'NONE',  ( -18.63466726053507472, 40.00000000000000000, -9.179856479542758407 ) ) ;
#24179 = ORIENTED_EDGE ( 'NONE', *, *, #38884, .T. ) ;
#24180 = FACE_OUTER_BOUND ( 'NONE', #18253, .T. ) ;
#24181 = LINE ( 'NONE', #21135, #434 ) ;
#24182 = CARTESIAN_POINT ( 'NONE',  ( -5.321195512787073589, 31.00000000000000355, 79.59297073838583003 ) ) ;
#24183 = CARTESIAN_POINT ( 'NONE',  ( -64.43604943162229404, 40.00000000000000711, 49.29347324003091302 ) ) ;
#24184 = CIRCLE ( 'NONE', #7419, 36.00000000000000000 ) ;
#24185 = DIRECTION ( 'NONE',  ( 0.000000000000000000, 0.000000000000000000, 1.000000000000000000 ) ) ;
#24186 = ORIENTED_EDGE ( 'NONE', *, *, #11057, .T. ) ;
#24187 = DIRECTION ( 'NONE',  ( 0.000000000000000000, 0.000000000000000000, 1.000000000000000000 ) ) ;
#24188 = ORIENTED_EDGE ( 'NONE', *, *, #34031, .F. ) ;
#24189 = SURFACE_STYLE_FILL_AREA ( #37233 ) ;
#24190 = EDGE_CURVE ( 'NONE', #6476, #20315, #22289, .T. ) ;
#24191 = CARTESIAN_POINT ( 'NONE',  ( 17.99999999999999645, 3.803237743091921974, 31.26855263151016828 ) ) ;
#24192 = ADVANCED_FACE ( 'NONE', ( #5230 ), #35537, .T. ) ;
#24193 = CIRCLE ( 'NONE', #3226, 20.00000000000000711 ) ;
#24194 = EDGE_CURVE ( 'NONE', #37603, #42396, #24911, .T. ) ;
#24195 = EDGE_CURVE ( 'NONE', #5010, #36072, #5366, .T. ) ;
#24197 = ORIENTED_EDGE ( 'NONE', *, *, #20755, .F. ) ;
#24196 = CARTESIAN_POINT ( 'NONE',  ( -12.69999999999999929, 0.000000000000000000, -12.59999999999999964 ) ) ;
#24198 = FACE_OUTER_BOUND ( 'NONE', #407, .T. ) ;
#24200 = ORIENTED_EDGE ( 'NONE', *, *, #6160, .F. ) ;
#24199 = CIRCLE ( 'NONE', #3230, 58.99999999999999289 ) ;
#24201 = CARTESIAN_POINT ( 'NONE',  ( 18.00000000000000355, 0.000000000000000000, 0.000000000000000000 ) ) ;
#24202 = AXIS2_PLACEMENT_3D ( 'NONE', #12948, #13, #20372 ) ;
#24203 = CARTESIAN_POINT ( 'NONE',  ( -36.24314215638268877, 40.00000000000000000, -73.49571118816069770 ) ) ;
#24204 = FACE_OUTER_BOUND ( 'NONE', #11872, .T. ) ;
#24205 = CIRCLE ( 'NONE', #42270, 13.59999999999999787 ) ;
#24206 = ORIENTED_EDGE ( 'NONE', *, *, #25501, .F. ) ;
#24207 = CYLINDRICAL_SURFACE ( 'NONE', #9500, 59.00000000000000000 ) ;
#24208 = CARTESIAN_POINT ( 'NONE',  ( 0.000000000000000000, -120.4984140710909344, 0.7894348306980505381 ) ) ;
#24209 = AXIS2_PLACEMENT_3D ( 'NONE', #2922, #19570, #32843 ) ;
#24210 = ORIENTED_EDGE ( 'NONE', *, *, #4999, .F. ) ;
#24211 = VECTOR ( 'NONE', #12022, 1000.000000000000000 ) ;
#24212 = FILL_AREA_STYLE_COLOUR ( '', #31664 ) ;
#24213 = ORIENTED_EDGE ( 'NONE', *, *, #21108, .T. ) ;
#24214 = LINE ( 'NONE', #34201, #27506 ) ;
#24215 = VERTEX_POINT ( 'NONE', #18597 ) ;
#24216 = DIRECTION ( 'NONE',  ( 0.000000000000000000, 0.000000000000000000, 1.000000000000000000 ) ) ;
#24217 = CARTESIAN_POINT ( 'NONE',  ( -5.991980000000000750, 0.000000000000000000, 0.000000000000000000 ) ) ;
#24218 = VECTOR ( 'NONE', #13469, 1000.000000000000000 ) ;
#24219 = CARTESIAN_POINT ( 'NONE',  ( 0.000000000000000000, -109.1131968884000258, 26.12628443611856355 ) ) ;
#24220 = CARTESIAN_POINT ( 'NONE',  ( 0.000000000000000000, -32.49609705003694415, -15.49205204337308395 ) ) ;
#24221 = VERTEX_POINT ( 'NONE', #15723 ) ;
#24223 = DIRECTION ( 'NONE',  ( 1.000000000000000000, -0.000000000000000000, -0.000000000000000000 ) ) ;
#24222 = CARTESIAN_POINT ( 'NONE',  ( 0.000000000000000000, 6.109652351741791776, 46.58570277113511793 ) ) ;
#24224 = ORIENTED_EDGE ( 'NONE', *, *, #6083, .T. ) ;
#24225 = EDGE_CURVE ( 'NONE', #8904, #31415, #9540, .T. ) ;
#24226 = DIRECTION ( 'NONE',  ( 0.000000000000000000, 0.9911528310040075285, -0.1327255272837188915 ) ) ;
#24227 = EDGE_CURVE ( 'NONE', #42671, #4007, #20042, .T. ) ;
#24228 = CARTESIAN_POINT ( 'NONE',  ( -12.50349052776452297, 31.00000000000000355, 25.37591446456323041 ) ) ;
#24229 = VERTEX_POINT ( 'NONE', #31864 ) ;
#24230 = DIRECTION ( 'NONE',  ( 0.000000000000000000, -0.9574220383620081209, 0.2886919473396123981 ) ) ;
#24231 = FACE_BOUND ( 'NONE', #26034, .T. ) ;
#24232 = AXIS2_PLACEMENT_3D ( 'NONE', #41467, #17536, #30809 ) ;
#24233 = ITEM_DEFINED_TRANSFORMATION ( 'NONE', 'NONE', #35107,  #13552 ) ;
#24234 = AXIS2_PLACEMENT_3D ( 'NONE', #14912, #12062, #15349 ) ;
#24235 = CARTESIAN_POINT ( 'NONE',  ( -106.4195705685749402, 106.4195705685765745, 10.00000000000033573 ) ) ;
#24236 = CARTESIAN_POINT ( 'NONE',  ( -69.34045338167970840, 31.00000000000000711, 9.142281554609933636 ) ) ;
#24237 = VECTOR ( 'NONE', #28093, 1000.000000000000000 ) ;
#24238 = AXIS2_PLACEMENT_3D ( 'NONE', #17608, #30877, #26965 ) ;
#24239 = EDGE_LOOP ( 'NONE', ( #8474, #14149, #38515, #21740 ) ) ;
#24241 = CARTESIAN_POINT ( 'NONE',  ( 34.59698569360211451, 31.00000000000000355, -30.23997570423561498 ) ) ;
#24240 = CIRCLE ( 'NONE', #5394, 10.49999999999999467 ) ;
#24242 = CARTESIAN_POINT ( 'NONE',  ( 66.75212336275305347, 39.99999999999999289, -51.21939497476837744 ) ) ;
#24243 = DIRECTION ( 'NONE',  ( 0.000000000000000000, -0.5877852522924624790, -0.8090169943749551118 ) ) ;
#24244 = EDGE_CURVE ( 'NONE', #37542, #39731, #1867, .T. ) ;
#24245 = CARTESIAN_POINT ( 'NONE',  ( 17.99999999999999645, -72.00556975657644898, -86.04342158279462183 ) ) ;
#24246 = DIRECTION ( 'NONE',  ( -3.996523416598930318E-16, 2.658563593772947863E-15, 1.000000000000000000 ) ) ;
#24247 = EDGE_CURVE ( 'NONE', #30236, #18949, #2157, .T. ) ;
#24248 = EDGE_CURVE ( 'NONE', #3479, #13442, #4636, .T. ) ;
#24249 = EDGE_CURVE ( 'NONE', #16448, #37680, #8852, .T. ) ;
#24251 = ORIENTED_EDGE ( 'NONE', *, *, #25085, .T. ) ;
#24250 = CARTESIAN_POINT ( 'NONE',  ( 0.5999999999999994227, -12.75000000000000000, -1.199999999999999956 ) ) ;
#24252 = CARTESIAN_POINT ( 'NONE',  ( 18.00000000000000355, -36.34385289850569478, -29.77717097092114429 ) ) ;
#24253 = DIRECTION ( 'NONE',  ( -1.000000000000000000, -0.000000000000000000, 0.000000000000000000 ) ) ;
#24254 = EDGE_CURVE ( 'NONE', #19014, #26640, #1733, .T. ) ;
#24255 = ORIENTED_EDGE ( 'NONE', *, *, #41789, .F. ) ;
#24256 = CARTESIAN_POINT ( 'NONE',  ( -40.58740609958903889, 40.00000000000000000, -31.12922691583434798 ) ) ;
#24257 = CARTESIAN_POINT ( 'NONE',  ( 1.598609366639573350E-14, -1.063425437509180407E-13, -40.00000000000000000 ) ) ;
#24258 = FACE_OUTER_BOUND ( 'NONE', #20940, .T. ) ;
#24259 = VERTEX_POINT ( 'NONE', #8297 ) ;
#24260 = VECTOR ( 'NONE', #17341, 1000.000000000000000 ) ;
#24261 = CARTESIAN_POINT ( 'NONE',  ( 18.00000000000000355, -18.53613841426823328, 48.58406706613896375 ) ) ;
#24262 = CARTESIAN_POINT ( 'NONE',  ( -4.000000000000000000, -2.309401076758515803, -0.4999999999999995559 ) ) ;
#24263 = VERTEX_POINT ( 'NONE', #16354 ) ;
#24264 = DIRECTION ( 'NONE',  ( 0.000000000000000000, 0.000000000000000000, 1.000000000000000000 ) ) ;
#24265 = ADVANCED_FACE ( 'NONE', ( #29446 ), #33355, .T. ) ;
#24266 = EDGE_LOOP ( 'NONE', ( #1220, #5604, #8401, #7194 ) ) ;
#24267 = AXIS2_PLACEMENT_3D ( 'NONE', #39260, #22747, #36001 ) ;
#24268 = DIRECTION ( 'NONE',  ( 0.000000000000000000, -0.2486898871648416942, -0.9685831611286345177 ) ) ;
#24269 = EDGE_LOOP ( 'NONE', ( #33692, #8818, #8924, #21864 ) ) ;
#24270 = VECTOR ( 'NONE', #20649, 1000.000000000000000 ) ;
#24271 = CARTESIAN_POINT ( 'NONE',  ( 0.000000000000000000, 109.4038418350910433, -50.51029986767441216 ) ) ;
#24272 = DIRECTION ( 'NONE',  ( 1.000000000000000000, -0.000000000000000000, -0.000000000000000000 ) ) ;
#24273 = EDGE_LOOP ( 'NONE', ( #23487, #15219, #37477, #8113 ) ) ;
#24274 = B_SPLINE_CURVE_WITH_KNOTS ( 'NONE', 3,
 ( #30338, #3674, #36419, #30566, #23376, #37295, #10691, #30128 ),
 .UNSPECIFIED., .F., .F.,
 ( 4, 2, 2, 4 ),
 ( 0.005725059856848645212, 0.006314084072593634418, 0.006903108288338624492, 0.008081156719828603771 ),
 .UNSPECIFIED. ) ;
#24275 = CIRCLE ( 'NONE', #15881, 20.00000000000000355 ) ;
#24276 = FACE_OUTER_BOUND ( 'NONE', #38749, .T. ) ;
#24277 = LINE ( 'NONE', #28170, #26167 ) ;
#24278 = ORIENTED_EDGE ( 'NONE', *, *, #18158, .F. ) ;
#24279 = CARTESIAN_POINT ( 'NONE',  ( 0.000000000000000000, 0.000000000000000000, -4.974599999999998801 ) ) ;
#24280 = CIRCLE ( 'NONE', #13114, 20.00000000000000355 ) ;
#24281 = DIRECTION ( 'NONE',  ( 0.000000000000000000, -0.8747630845319658288, 0.4845508703326421585 ) ) ;
#24282 = DIRECTION ( 'NONE',  ( 1.000000000000000000, 0.000000000000000000, 0.000000000000000000 ) ) ;
#24283 = CARTESIAN_POINT ( 'NONE',  ( -24.74979319748359785, 5.944745455504278020, 2.972870684497277427 ) ) ;
#24284 = ADVANCED_FACE ( 'NONE', ( #12654 ), #23344, .T. ) ;
#24285 = VERTEX_POINT ( 'NONE', #2991 ) ;
#24286 = CARTESIAN_POINT ( 'NONE',  ( -83.76341667917206735, -0.9999999999999806821, 6.300002081858462333 ) ) ;
#24287 = LINE ( 'NONE', #14015, #36444 ) ;
#24288 = CARTESIAN_POINT ( 'NONE',  ( 16.30133787010129254, 31.00000000000000355, 33.04822796959624753 ) ) ;
#24289 = VERTEX_POINT ( 'NONE', #3437 ) ;
#24291 = CYLINDRICAL_SURFACE ( 'NONE', #4449, 2.649999999999957723 ) ;
#24290 = DIRECTION ( 'NONE',  ( -1.000000000000000000, -0.000000000000000000, 0.000000000000000000 ) ) ;
#24292 = CARTESIAN_POINT ( 'NONE',  ( 0.000000000000000000, -109.3506818544112917, 38.70953859160975696 ) ) ;
#24293 = VECTOR ( 'NONE', #19258, 1000.000000000000000 ) ;
#24294 = ORIENTED_EDGE ( 'NONE', *, *, #42296, .T. ) ;
#24295 = CARTESIAN_POINT ( 'NONE',  ( 17.99999999999999645, 0.000000000000000000, 0.000000000000000000 ) ) ;
#24296 = CARTESIAN_POINT ( 'NONE',  ( 44.91824650936478491, 40.00000000000000000, 5.910997147197376123 ) ) ;
#24297 = AXIS2_PLACEMENT_3D ( 'NONE', #12428, #18793, #15495 ) ;
#24298 = CARTESIAN_POINT ( 'NONE',  ( 56.89991739620084843, 40.00000000000000000, -3.630084216720919521 ) ) ;
#24299 = CIRCLE ( 'NONE', #29854, 20.00000000000000711 ) ;
#24300 = AXIS2_PLACEMENT_3D ( 'NONE', #30423, #23684, #39566 ) ;
#24301 = VECTOR ( 'NONE', #28004, 1000.000000000000000 ) ;
#24302 = CARTESIAN_POINT ( 'NONE',  ( 17.99999999999999645, 75.72520367775085504, 82.78868281116005789 ) ) ;
#24303 = CARTESIAN_POINT ( 'NONE',  ( 0.000000000000000000, 87.74575819880170968, 75.87280091124503656 ) ) ;
#24304 = EDGE_CURVE ( 'NONE', #6283, #28510, #40873, .T. ) ;
#24305 = ADVANCED_FACE ( 'NONE', ( #42506 ), #6088, .T. ) ;
#24306 = CYLINDRICAL_SURFACE ( 'NONE', #15084, 116.0000000000000000 ) ;
#24307 = DIRECTION ( 'NONE',  ( -1.000000000000000000, 0.000000000000000000, -0.000000000000000000 ) ) ;
#24308 = EDGE_CURVE ( 'NONE', #26693, #26169, #1172, .T. ) ;
#24309 = ORIENTED_EDGE ( 'NONE', *, *, #8340, .F. ) ;
#24310 = CARTESIAN_POINT ( 'NONE',  ( 19.04566582976364941, 40.00000000000000000, -14.62000746238684989 ) ) ;
#24311 = ORIENTED_EDGE ( 'NONE', *, *, #13645, .F. ) ;
#24312 = CYLINDRICAL_SURFACE ( 'NONE', #41747, 120.5010000000000190 ) ;
#24313 = FACE_OUTER_BOUND ( 'NONE', #33168, .T. ) ;
#24314 = ORIENTED_EDGE ( 'NONE', *, *, #36863, .T. ) ;
#24315 = DIRECTION ( 'NONE',  ( -1.000000000000000000, 0.000000000000000000, 0.000000000000000000 ) ) ;
#24316 = DIRECTION ( 'NONE',  ( 1.000000000000000000, 0.000000000000000000, 0.000000000000000000 ) ) ;
#24317 = ORIENTED_EDGE ( 'NONE', *, *, #28578, .T. ) ;
#24318 = LINE ( 'NONE', #21263, #36798 ) ;
#24319 = VERTEX_POINT ( 'NONE', #22940 ) ;
#24320 = ADVANCED_FACE ( 'NONE', ( #23141 ), #39662, .T. ) ;
#24321 = VERTEX_POINT ( 'NONE', #19439 ) ;
#24323 = ORIENTED_EDGE ( 'NONE', *, *, #18271, .F. ) ;
#24322 = CARTESIAN_POINT ( 'NONE',  ( 0.000000000000000000, 0.000000000000000000, 0.000000000000000000 ) ) ;
#24324 = CARTESIAN_POINT ( 'NONE',  ( -61.81085491475939619, 31.00000000000000711, 35.57109242551294415 ) ) ;
#24325 = ORIENTED_EDGE ( 'NONE', *, *, #29534, .F. ) ;
#24326 = LINE ( 'NONE', #30837, #20296 ) ;
#24327 = AXIS2_PLACEMENT_3D ( 'NONE', #32948, #33389, #3474 ) ;
#24328 = AXIS2_PLACEMENT_3D ( 'NONE', #1505, #11571, #24914 ) ;
#24329 = AXIS2_PLACEMENT_3D ( 'NONE', #25646, #5741, #36053 ) ;
#24330 = ORIENTED_EDGE ( 'NONE', *, *, #9253, .T. ) ;
#24331 = DIRECTION ( 'NONE',  ( -1.000000000000000000, -0.000000000000000000, -0.000000000000000000 ) ) ;
#24332 = EDGE_LOOP ( 'NONE', ( #12624, #22979, #14432, #7974 ) ) ;
#24333 = CARTESIAN_POINT ( 'NONE',  ( -91.59543978412355614, 40.00000000000000711, -12.18496625897608254 ) ) ;
#24334 = CIRCLE ( 'NONE', #10267, 0.4000000000000001887 ) ;
#24335 = B_SPLINE_CURVE_WITH_KNOTS ( 'NONE', 3,
 ( #28440, #18852, #32313, #8337, #12271 ),
 .UNSPECIFIED., .F., .F.,
 ( 4, 1, 4 ),
 ( 0.000000000000000000, 0.002309401076758505356, 0.004618802153517010713 ),
 .UNSPECIFIED. ) ;
#24337 = DIRECTION ( 'NONE',  ( -1.000000000000000000, 0.000000000000000000, 0.000000000000000000 ) ) ;
#24336 = CARTESIAN_POINT ( 'NONE',  ( 8.999999999999998224, -37.07968990261405651, -109.9140418541961282 ) ) ;
#24338 = DIRECTION ( 'NONE',  ( -1.000000000000000000, -0.000000000000000000, -0.000000000000000000 ) ) ;
#24339 = EDGE_CURVE ( 'NONE', #34983, #17035, #18662, .T. ) ;
#24340 = LINE ( 'NONE', #28238, #6839 ) ;
#24341 = EDGE_LOOP ( 'NONE', ( #19773, #19687, #42865, #17744 ) ) ;
#24342 = DIRECTION ( 'NONE',  ( 0.000000000000000000, 0.000000000000000000, 1.000000000000000000 ) ) ;
#24343 = FACE_OUTER_BOUND ( 'NONE', #16822, .T. ) ;
#24344 = CARTESIAN_POINT ( 'NONE',  ( -89.89583333403318477, 31.00000000000000711, 5.890486217120591839 ) ) ;
#24345 = CARTESIAN_POINT ( 'NONE',  ( 0.000000000000000000, -43.83938735307255286, -18.28286404005844901 ) ) ;
#24346 = VERTEX_POINT ( 'NONE', #30097 ) ;
#24347 = CARTESIAN_POINT ( 'NONE',  ( 15.59370980024836051, 40.00000000000000000, -20.29731371384565364 ) ) ;
#24348 = ORIENTED_EDGE ( 'NONE', *, *, #18062, .T. ) ;
#24349 = VERTEX_POINT ( 'NONE', #150 ) ;
#24350 = CARTESIAN_POINT ( 'NONE',  ( 17.99999999999999645, 21.48775762007893420, -23.64423737150114135 ) ) ;
#24351 = AXIS2_PLACEMENT_3D ( 'NONE', #14310, #539, #37190 ) ;
#24352 = CARTESIAN_POINT ( 'NONE',  ( -106.4195705685748550, -106.4195705685759776, 9.999999999999998224 ) ) ;
#24353 = AXIS2_PLACEMENT_3D ( 'NONE', #10147, #9728, #23498 ) ;
#24354 = ADVANCED_FACE ( 'NONE', ( #9788 ), #26810, .F. ) ;
#24355 = CARTESIAN_POINT ( 'NONE',  ( 17.99999999999999645, 31.48608500567870294, 0.9019157472705636724 ) ) ;
#24356 = VERTEX_POINT ( 'NONE', #16594 ) ;
#24357 = DIRECTION ( 'NONE',  ( 1.000000000000000000, 0.000000000000000000, -0.000000000000000000 ) ) ;
#24358 = ORIENTED_EDGE ( 'NONE', *, *, #16992, .F. ) ;
#24359 = DIRECTION ( 'NONE',  ( 3.892440008040322386E-16, -2.658563593772947863E-15, -1.000000000000000000 ) ) ;
#24360 = DIRECTION ( 'NONE',  ( -1.000000000000000000, 0.000000000000000000, 0.000000000000000000 ) ) ;
#24361 = EDGE_CURVE ( 'NONE', #33336, #32964, #27685, .T. ) ;
#24362 = DIRECTION ( 'NONE',  ( 0.000000000000000000, 0.4999999999999992784, -0.8660254037844389297 ) ) ;
#24363 = CARTESIAN_POINT ( 'NONE',  ( 0.000000000000000000, -119.0898412705475522, 18.38751498043690802 ) ) ;
#24364 = VERTEX_POINT ( 'NONE', #43153 ) ;
#24365 = ORIENTED_EDGE ( 'NONE', *, *, #1409, .T. ) ;
#24366 = DIRECTION ( 'NONE',  ( 0.000000000000000000, -0.8747630845319657178, 0.4845508703326421029 ) ) ;
#24367 = CARTESIAN_POINT ( 'NONE',  ( 18.00000000000000355, 27.79676263918241119, -37.88001506494740056 ) ) ;
#24368 = EDGE_CURVE ( 'NONE', #3942, #3164, #26174, .T. ) ;
#24369 = CARTESIAN_POINT ( 'NONE',  ( -31.75000000000000000, -18.77999999999999403, 2.299886688798728717E-15 ) ) ;
#24370 = ORIENTED_EDGE ( 'NONE', *, *, #2149, .F. ) ;
#24372 = ORIENTED_EDGE ( 'NONE', *, *, #37838, .F. ) ;
#24371 = CARTESIAN_POINT ( 'NONE',  ( 0.000000000000000000, 37.07968990261625208, -109.9140418541953750 ) ) ;
#24373 = ADVANCED_FACE ( 'NONE', ( #6938 ), #20297, .T. ) ;
#24374 = CARTESIAN_POINT ( 'NONE',  ( 31.88898475263450649, 31.00000000000000355, 36.48290236124523744 ) ) ;
#24375 = LINE ( 'NONE', #21760, #25160 ) ;
#24377 = DIRECTION ( 'NONE',  ( -1.000000000000000000, 0.000000000000000000, -0.000000000000000000 ) ) ;
#24376 = DIRECTION ( 'NONE',  ( 1.000000000000000000, 0.000000000000000000, 0.000000000000000000 ) ) ;
#24378 = UNCERTAINTY_MEASURE_WITH_UNIT (LENGTH_MEASURE( 1.000000000000000082E-05 ), #17378, 'distance_accuracy_value', 'NONE');
#24379 = EDGE_LOOP ( 'NONE', ( #39548, #21944, #31431, #15994 ) ) ;
#24380 = CARTESIAN_POINT ( 'NONE',  ( 59.60939625460783731, 39.99999999999999289, -29.27517545779414831 ) ) ;
#24381 = AXIS2_PLACEMENT_3D ( 'NONE', #42601, #5964, #2880 ) ;
#24382 = AXIS2_PLACEMENT_3D ( 'NONE', #36901, #36034, #39292 ) ;
#24383 = LINE ( 'NONE', #550, #21430 ) ;
#24384 = CYLINDRICAL_SURFACE ( 'NONE', #3124, 59.00000000000000000 ) ;
#24385 = ORIENTED_EDGE ( 'NONE', *, *, #29530, .F. ) ;
#24386 = AXIS2_PLACEMENT_3D ( 'NONE', #41421, #37519, #24469 ) ;
#24387 = CARTESIAN_POINT ( 'NONE',  ( 17.99999999999999645, 92.10690493017145286, -64.06707842432085442 ) ) ;
#24388 = EDGE_CURVE ( 'NONE', #13634, #41864, #15943, .T. ) ;
#24389 = ORIENTED_EDGE ( 'NONE', *, *, #8739, .T. ) ;
#24390 =( LENGTH_UNIT ( ) NAMED_UNIT ( * ) SI_UNIT ( .MILLI., .METRE. ) );
#24391 = EDGE_CURVE ( 'NONE', #22786, #20683, #25583, .T. ) ;
#24392 = CARTESIAN_POINT ( 'NONE',  ( 0.000000000000000000, 0.000000000000000000, 0.000000000000000000 ) ) ;
#24393 = CARTESIAN_POINT ( 'NONE',  ( 0.000000000000000000, 19.44205635905542096, 43.33776004284615624 ) ) ;
#24395 = EDGE_CURVE ( 'NONE', #15861, #42903, #26952, .T. ) ;
#24394 = CARTESIAN_POINT ( 'NONE',  ( 34.44467569804516671, 31.00000000000000355, 44.88666365967159777 ) ) ;
#24396 = CARTESIAN_POINT ( 'NONE',  ( 17.99999999999999645, -111.2559044912527355, 32.83479428644638887 ) ) ;
#24397 = ORIENTED_EDGE ( 'NONE', *, *, #34416, .F. ) ;
#24398 =( NAMED_UNIT ( * ) SI_UNIT ( $, .STERADIAN. ) SOLID_ANGLE_UNIT ( ) );
#24399 = ORIENTED_EDGE ( 'NONE', *, *, #4670, .F. ) ;
#24400 = CARTESIAN_POINT ( 'NONE',  ( -23.02120395722396395, 40.00000000000000000, 17.66995642160909696 ) ) ;
#24401 = EDGE_LOOP ( 'NONE', ( #24699, #17887, #28784, #22495 ) ) ;
#24402 = DIRECTION ( 'NONE',  ( 3.009274222672345096E-17, 1.000000000000000000, -2.455023325076455345E-18 ) ) ;
#24403 = DIRECTION ( 'NONE',  ( 0.000000000000000000, 0.000000000000000000, -1.000000000000000000 ) ) ;
#24404 = CARTESIAN_POINT ( 'NONE',  ( 76.30724621508588257, 31.00000000000000000, -9.942258256679791018 ) ) ;
#24405 = CARTESIAN_POINT ( 'NONE',  ( 74.90833963778730720, 39.99999999999999289, 20.17845691863183077 ) ) ;
#24406 = CARTESIAN_POINT ( 'NONE',  ( 9.000000000000001776, -11.65176648921111635, 115.4133282497342066 ) ) ;
#24407 = ADVANCED_FACE ( 'NONE', ( #9997 ), #38283, .T. ) ;
#24408 = ORIENTED_EDGE ( 'NONE', *, *, #20669, .F. ) ;
#24409 = CARTESIAN_POINT ( 'NONE',  ( -80.96080130434580724, -40.05525454449572464, 14.45886780445738395 ) ) ;
#24410 = ORIENTED_EDGE ( 'NONE', *, *, #1761, .F. ) ;
#24411 = AXIS2_PLACEMENT_3D ( 'NONE', #35618, #5737, #19093 ) ;
#24412 = DIRECTION ( 'NONE',  ( -1.000000000000000000, 0.000000000000000000, 0.000000000000000000 ) ) ;
#24413 = CYLINDRICAL_SURFACE ( 'NONE', #5963, 120.5010000000000190 ) ;
#24415 = ORIENTED_EDGE ( 'NONE', *, *, #36791, .F. ) ;
#24414 = CARTESIAN_POINT ( 'NONE',  ( 20.00000000000000000, 2.449293598294706513E-15, -6.000000000000000000 ) ) ;
#24416 = DIRECTION ( 'NONE',  ( -1.000000000000000000, 0.000000000000000000, -0.000000000000000000 ) ) ;
#24417 = ORIENTED_EDGE ( 'NONE', *, *, #13485, .T. ) ;
#24418 = CARTESIAN_POINT ( 'NONE',  ( 17.99999999999999645, -109.1131968884000258, 26.12628443611856355 ) ) ;
#24419 = EDGE_CURVE ( 'NONE', #2932, #4859, #14764, .T. ) ;
#24420 = CARTESIAN_POINT ( 'NONE',  ( 12.12865573427490062, 40.00000000000000000, -92.11205733446308841 ) ) ;
#24421 = CARTESIAN_POINT ( 'NONE',  ( 17.99999999999999645, 0.000000000000000000, 0.000000000000000000 ) ) ;
#24422 = ORIENTED_EDGE ( 'NONE', *, *, #32149, .T. ) ;
#24423 = CARTESIAN_POINT ( 'NONE',  ( 17.99999999999999645, 15.21076497709875497, -119.5371223922153519 ) ) ;
#24424 = CYLINDRICAL_SURFACE ( 'NONE', #20447, 158.5000000000000284 ) ;
#24425 = EDGE_CURVE ( 'NONE', #848, #31963, #18275, .T. ) ;
#24426 = ORIENTED_EDGE ( 'NONE', *, *, #26096, .T. ) ;
#24427 = DIRECTION ( 'NONE',  ( -1.000000000000000000, -0.000000000000000000, -0.000000000000000000 ) ) ;
#24428 = EDGE_LOOP ( 'NONE', ( #19649, #26893, #18262, #26121 ) ) ;
#24429 = B_SPLINE_CURVE_WITH_KNOTS ( 'NONE', 3,
 ( #36958, #7069, #31075, #41079, #17589, #20640, #20870, #20423 ),
 .UNSPECIFIED., .F., .F.,
 ( 4, 2, 2, 4 ),
 ( 7.780516681398759253E-20, 0.002450665683189819696, 0.003675998524784729327, 0.004901331366379639391 ),
 .UNSPECIFIED. ) ;
#24430 = CARTESIAN_POINT ( 'NONE',  ( -24.93870012979089168, 40.00000000000000000, -21.94074674037796058 ) ) ;
#24431 = LINE ( 'NONE', #41164, #38285 ) ;
#24432 = DIRECTION ( 'NONE',  ( -1.000000000000000000, 0.000000000000000000, -0.000000000000000000 ) ) ;
#24433 = DIRECTION ( 'NONE',  ( 1.000000000000000000, 0.000000000000000000, 0.000000000000000000 ) ) ;
#24434 = ORIENTED_EDGE ( 'NONE', *, *, #34060, .F. ) ;
#24436 = DIRECTION ( 'NONE',  ( -1.000000000000000000, 0.000000000000000000, 0.000000000000000000 ) ) ;
#24435 = CARTESIAN_POINT ( 'NONE',  ( 0.000000000000000000, 0.000000000000000000, -25.00000000000000000 ) ) ;
#24437 = VERTEX_POINT ( 'NONE', #4693 ) ;
#24439 = ADVANCED_FACE ( 'NONE', ( #41326 ), #21765, .F. ) ;
#24438 = AXIS2_PLACEMENT_3D ( 'NONE', #15294, #11562, #8695 ) ;
#24440 = CARTESIAN_POINT ( 'NONE',  ( -10.00000000000000000, 0.000000000000000000, 0.000000000000000000 ) ) ;
#24441 = AXIS2_PLACEMENT_3D ( 'NONE', #31560, #11080, #1227 ) ;
#24444 = EDGE_CURVE ( 'NONE', #40202, #2894, #1413, .T. ) ;
#24443 = CARTESIAN_POINT ( 'NONE',  ( -25.30796725786148826, 31.00000000000000355, 14.62256337265529815 ) ) ;
#24442 = CIRCLE ( 'NONE', #23779, 13.59999999999999787 ) ;
#24445 = ORIENTED_EDGE ( 'NONE', *, *, #5272, .F. ) ;
#24446 = DIRECTION ( 'NONE',  ( -1.000000000000000000, 0.000000000000000000, 0.000000000000000000 ) ) ;
#24447 = AXIS2_PLACEMENT_3D ( 'NONE', #25791, #2608, #9612 ) ;
#24448 = CARTESIAN_POINT ( 'NONE',  ( -4.000000000000000888, -1.539600717839011201, -3.300726591567081591 ) ) ;
#24449 = CONTEXT_DEPENDENT_SHAPE_REPRESENTATION ( #32318, #17277 ) ;
#24450 = DIRECTION ( 'NONE',  ( 0.000000000000000000, 0.000000000000000000, 1.000000000000000000 ) ) ;
#24451 = CARTESIAN_POINT ( 'NONE',  ( -39.25113411183426848, 31.00000000000000355, 67.98392962655870519 ) ) ;
#24452 = EDGE_LOOP ( 'NONE', ( #42277, #26272, #739, #5434 ) ) ;
#24453 = EDGE_CURVE ( 'NONE', #5690, #28933, #36707, .T. ) ;
#24454 = CARTESIAN_POINT ( 'NONE',  ( -40.27082278477694643, 31.00000000000000355, 10.71261860272906397 ) ) ;
#24455 = CARTESIAN_POINT ( 'NONE',  ( -71.24862878704732339, 40.00000000000000711, 35.13526414049667324 ) ) ;
#24456 = EDGE_CURVE ( 'NONE', #42289, #19812, #36017, .T. ) ;
#24457 = ADVANCED_FACE ( 'NONE', ( #35015 ), #24815, .T. ) ;
#24458 = DIRECTION ( 'NONE',  ( -1.000000000000000000, -0.000000000000000000, -0.000000000000000000 ) ) ;
#24459 = FACE_OUTER_BOUND ( 'NONE', #2242, .T. ) ;
#24460 = LINE ( 'NONE', #20979, #3064 ) ;
#24462 = ORIENTED_EDGE ( 'NONE', *, *, #32426, .T. ) ;
#24461 = CARTESIAN_POINT ( 'NONE',  ( 17.99999999999999645, 0.000000000000000000, 0.000000000000000000 ) ) ;
#24463 = CARTESIAN_POINT ( 'NONE',  ( 106.4195705685756792, -106.4195705685758213, 9.999999999999671374 ) ) ;
#24464 = CIRCLE ( 'NONE', #11209, 14.91999999999999993 ) ;
#24465 = FACE_OUTER_BOUND ( 'NONE', #43059, .T. ) ;
#24466 = EDGE_CURVE ( 'NONE', #38673, #17173, #13661, .T. ) ;
#24467 = ORIENTED_EDGE ( 'NONE', *, *, #34297, .F. ) ;
#24468 = CARTESIAN_POINT ( 'NONE',  ( 17.40022565512299479, 40.00000000000000000, 64.93645345284011228 ) ) ;
#24469 = DIRECTION ( 'NONE',  ( 0.000000000000000000, -0.9574220383620022368, -0.2886919473396315494 ) ) ;
#24471 = CARTESIAN_POINT ( 'NONE',  ( 0.000000000000000000, 0.000000000000000000, 0.000000000000000000 ) ) ;
#24470 = VECTOR ( 'NONE', #38120, 1000.000000000000000 ) ;
#24472 = ORIENTED_EDGE ( 'NONE', *, *, #9218, .T. ) ;
#24473 = ADVANCED_FACE ( 'NONE', ( #8194 ), #21556, .F. ) ;
#24474 = CIRCLE ( 'NONE', #8331, 59.00000000000000711 ) ;
#24475 = CARTESIAN_POINT ( 'NONE',  ( 0.000000000000000000, -2.123073309834832667, -47.45152853935337589 ) ) ;
#24476 = FACE_OUTER_BOUND ( 'NONE', #17349, .T. ) ;
#24477 = VECTOR ( 'NONE', #19205, 1000.000000000000000 ) ;
#24478 = ORIENTED_EDGE ( 'NONE', *, *, #33722, .F. ) ;
#24479 = CARTESIAN_POINT ( 'NONE',  ( 17.99999999999999645, 0.000000000000000000, 0.000000000000000000 ) ) ;
#24480 = ORIENTED_EDGE ( 'NONE', *, *, #37787, .F. ) ;
#24481 = CYLINDRICAL_SURFACE ( 'NONE', #35089, 20.00000000000000000 ) ;
#24482 = ORIENTED_EDGE ( 'NONE', *, *, #2840, .F. ) ;
#24483 = DIRECTION ( 'NONE',  ( -1.000000000000000000, -0.000000000000000000, 0.000000000000000000 ) ) ;
#24484 = DIRECTION ( 'NONE',  ( 0.000000000000000000, -0.9407002666710364558, 0.3392388661180213427 ) ) ;
#24485 = VERTEX_POINT ( 'NONE', #31539 ) ;
#24486 = ADVANCED_FACE ( 'NONE', ( #14980 ), #23519, .F. ) ;
#24487 = DIRECTION ( 'NONE',  ( -1.000000000000000000, 0.000000000000000000, 0.000000000000000000 ) ) ;
#24488 = DIRECTION ( 'NONE',  ( -3.614007241618348771E-16, 1.000000000000000000, 0.000000000000000000 ) ) ;
#24489 = ORIENTED_EDGE ( 'NONE', *, *, #17311, .F. ) ;
#24490 = CARTESIAN_POINT ( 'NONE',  ( 17.99999999999999645, -111.2721026680459602, 44.61974821237267719 ) ) ;
#24491 = DIRECTION ( 'NONE',  ( 1.000000000000000000, 0.000000000000000000, 0.000000000000000000 ) ) ;
#24492 = EDGE_CURVE ( 'NONE', #17035, #34983, #26200, .T. ) ;
#24493 = AXIS2_PLACEMENT_3D ( 'NONE', #6417, #35457, #25461 ) ;
#24494 = ADVANCED_FACE ( 'NONE', ( #27041 ), #40310, .T. ) ;
#24495 = DIRECTION ( 'NONE',  ( 0.000000000000000000, 0.000000000000000000, 1.000000000000000000 ) ) ;
#24496 = EDGE_CURVE ( 'NONE', #3911, #22441, #13763, .T. ) ;
#24497 = EDGE_CURVE ( 'NONE', #11322, #32708, #39363, .T. ) ;
#24498 = VECTOR ( 'NONE', #39980, 1000.000000000000000 ) ;
#24499 = DIRECTION ( 'NONE',  ( 0.000000000000000000, 0.8443279255020164076, -0.5358267949789947693 ) ) ;
#24500 = ORIENTED_EDGE ( 'NONE', *, *, #24361, .T. ) ;
#24501 = DIRECTION ( 'NONE',  ( -0.3092963776483742544, -2.892725781604664163E-17, -0.9509656937942579935 ) ) ;
#24502 = DIRECTION ( 'NONE',  ( -1.000000000000000000, -0.000000000000000000, -0.000000000000000000 ) ) ;
#24503 = CARTESIAN_POINT ( 'NONE',  ( -20.88694679984194380, 31.00000000000000355, -36.15586224631631751 ) ) ;
#24504 = AXIS2_PLACEMENT_3D ( 'NONE', #39329, #6193, #39129 ) ;
#24505 = EDGE_LOOP ( 'NONE', ( #31191, #30997, #36207, #30937 ) ) ;
#24507 = DIRECTION ( 'NONE',  ( -1.000000000000000000, 0.000000000000000000, 0.000000000000000000 ) ) ;
#24506 = CYLINDRICAL_SURFACE ( 'NONE', #20541, 59.00000000000000000 ) ;
#24508 = CIRCLE ( 'NONE', #23102, 59.00000000000000711 ) ;
#24509 = DIRECTION ( 'NONE',  ( 0.000000000000000000, 0.000000000000000000, 1.000000000000000000 ) ) ;
#24510 = ORIENTED_EDGE ( 'NONE', *, *, #6370, .F. ) ;
#24511 = AXIS2_PLACEMENT_3D ( 'NONE', #10586, #6438, #40238 ) ;
#24512 = FACE_OUTER_BOUND ( 'NONE', #7904, .T. ) ;
#24513 = CARTESIAN_POINT ( 'NONE',  ( -46.94946386092573221, 40.00000000000000000, 15.94926099647653928 ) ) ;
#24514 = CARTESIAN_POINT ( 'NONE',  ( -39.97893566998936876, 40.00000000000000000, -35.18630237794886995 ) ) ;
#24515 = VECTOR ( 'NONE', #32278, 1000.000000000000000 ) ;
#24516 = CYLINDRICAL_SURFACE ( 'NONE', #36006, 20.00000000000000355 ) ;
#24517 = DIRECTION ( 'NONE',  ( -1.000000000000000000, 0.000000000000000000, 0.000000000000000000 ) ) ;
#24518 = DIRECTION ( 'NONE',  ( -1.000000000000000000, -0.000000000000000000, -0.000000000000000000 ) ) ;
#24519 = DIRECTION ( 'NONE',  ( 0.000000000000000000, 0.000000000000000000, 1.000000000000000000 ) ) ;
#24520 = ORIENTED_EDGE ( 'NONE', *, *, #24308, .T. ) ;
#24521 = CARTESIAN_POINT ( 'NONE',  ( -29.59829689555773058, 40.00000000000000000, 3.906358533625565954 ) ) ;
#24522 = VERTEX_POINT ( 'NONE', #7456 ) ;
#24523 = DIRECTION ( 'NONE',  ( 0.000000000000000000, 0.000000000000000000, 1.000000000000000000 ) ) ;
#24524 = CARTESIAN_POINT ( 'NONE',  ( 18.00000000000000355, -43.83938735307255286, -18.28286404005844901 ) ) ;
#24525 = ORIENTED_EDGE ( 'NONE', *, *, #27354, .T. ) ;
#24526 = DIRECTION ( 'NONE',  ( 0.000000000000000000, 0.000000000000000000, 1.000000000000000000 ) ) ;
#24527 = DIRECTION ( 'NONE',  ( 0.000000000000000000, 0.000000000000000000, 1.000000000000000000 ) ) ;
#24528 = ORIENTED_EDGE ( 'NONE', *, *, #24768, .F. ) ;
#24529 = FACE_OUTER_BOUND ( 'NONE', #40891, .T. ) ;
#24530 = EDGE_CURVE ( 'NONE', #8821, #7115, #3864, .T. ) ;
#24531 = ORIENTED_EDGE ( 'NONE', *, *, #5828, .T. ) ;
#24532 = AXIS2_PLACEMENT_3D ( 'NONE', #17127, #14265, #254 ) ;
#24533 = EDGE_LOOP ( 'NONE', ( #17869, #20132, #39966, #42220 ) ) ;
#24534 = APPLICATION_CONTEXT ( 'automotive_design' ) ;
#24535 = CARTESIAN_POINT ( 'NONE',  ( 18.00000000000000355, -38.92705108641749945, 27.21837053747784552 ) ) ;
#24536 = CARTESIAN_POINT ( 'NONE',  ( 77.09314031436156256, 31.00000000000000000, 5.156213784760050878 ) ) ;
#24537 = ORIENTED_EDGE ( 'NONE', *, *, #2978, .T. ) ;
#24538 = CARTESIAN_POINT ( 'NONE',  ( 9.000000000000000000, -35.78425302087536863, -3.935382540233169912 ) ) ;
#24539 = VECTOR ( 'NONE', #20129, 1000.000000000000000 ) ;
#24540 = LINE ( 'NONE', #31275, #14306 ) ;
#24541 = ORIENTED_EDGE ( 'NONE', *, *, #30213, .F. ) ;
#24542 = CARTESIAN_POINT ( 'NONE',  ( 0.000000000000000000, 0.000000000000000000, -6.000000000000000000 ) ) ;
#24543 = ORIENTED_EDGE ( 'NONE', *, *, #32482, .T. ) ;
#24544 = CARTESIAN_POINT ( 'NONE',  ( -91.21105805184879500, 40.00000000000000711, 11.89862498596346718 ) ) ;
#24545 = AXIS2_PLACEMENT_3D ( 'NONE', #42614, #19752, #26496 ) ;
#24546 = DIRECTION ( 'NONE',  ( 1.000000000000000000, 0.000000000000000000, 0.000000000000000000 ) ) ;
#24547 = EDGE_CURVE ( 'NONE', #3132, #8703, #15851, .T. ) ;
#24548 = ADVANCED_FACE ( 'NONE', ( #10970 ), #24306, .F. ) ;
#24549 = CARTESIAN_POINT ( 'NONE',  ( 9.000000000000001776, 35.78484819117633720, 110.3423972910434117 ) ) ;
#24550 = DIRECTION ( 'NONE',  ( 1.000000000000000000, 0.000000000000000000, 0.000000000000000000 ) ) ;
#24551 = ORIENTED_EDGE ( 'NONE', *, *, #36496, .T. ) ;
#24552 = SURFACE_SIDE_STYLE ('',( #21074 ) ) ;
#24553 = ADVANCED_FACE ( 'NONE', ( #29579 ), #36519, .T. ) ;
#24554 = CARTESIAN_POINT ( 'NONE',  ( 18.00000000000000355, 0.000000000000000000, 0.000000000000000000 ) ) ;
#24555 = ORIENTED_EDGE ( 'NONE', *, *, #2911, .F. ) ;
#24556 = DIRECTION ( 'NONE',  ( -1.000000000000000000, -0.000000000000000000, -0.000000000000000000 ) ) ;
#24557 = CARTESIAN_POINT ( 'NONE',  ( 73.03870520561201829, 31.00000000000000000, -42.18585045165268355 ) ) ;
#24558 = DIRECTION ( 'NONE',  ( 0.000000000000000000, 0.9407002666710341243, -0.3392388661180279485 ) ) ;
#24559 = VERTEX_POINT ( 'NONE', #27545 ) ;
#24560 = CARTESIAN_POINT ( 'NONE',  ( -20.28213647683248766, 40.00000000000000000, 23.06128528321566051 ) ) ;
#24561 = ORIENTED_EDGE ( 'NONE', *, *, #39319, .T. ) ;
#24562 = EDGE_CURVE ( 'NONE', #21218, #15532, #30377, .T. ) ;
#24563 = ORIENTED_EDGE ( 'NONE', *, *, #42373, .F. ) ;
#24564 = CARTESIAN_POINT ( 'NONE',  ( 0.000000000000000000, 0.000000000000000000, -20.00000000000000000 ) ) ;
#24565 = CARTESIAN_POINT ( 'NONE',  ( 0.000000000000000000, -13.22719389141998469, 28.58720592780591474 ) ) ;
#24566 = CARTESIAN_POINT ( 'NONE',  ( -158.5000000000000284, 1.941065176648555254E-14, 6.999999999999998224 ) ) ;
#24567 = AXIS2_PLACEMENT_3D ( 'NONE', #36382, #25956, #43146 ) ;
#24568 = FACE_OUTER_BOUND ( 'NONE', #11268, .T. ) ;
#24569 = VERTEX_POINT ( 'NONE', #9716 ) ;
#24570 = LINE ( 'NONE', #33691, #3294 ) ;
#24571 = ORIENTED_EDGE ( 'NONE', *, *, #8542, .T. ) ;
#24572 = DIRECTION ( 'NONE',  ( -1.000000000000000000, 0.000000000000000000, -0.000000000000000000 ) ) ;
#24573 = AXIS2_PLACEMENT_3D ( 'NONE', #5294, #2008, #21714 ) ;
#24574 = DIRECTION ( 'NONE',  ( -1.058513553088275437E-16, -1.000000000000000000, 8.813324511995299047E-17 ) ) ;
#24575 = PLANE ( 'NONE',  #6766 ) ;
#24576 = DIRECTION ( 'NONE',  ( -1.000000000000000000, 0.000000000000000000, -0.000000000000000000 ) ) ;
#24577 = EDGE_LOOP ( 'NONE', ( #39747, #15785, #10784, #16603 ) ) ;
#24578 = EDGE_CURVE ( 'NONE', #9874, #41456, #40818, .T. ) ;
#24579 = ORIENTED_EDGE ( 'NONE', *, *, #40387, .T. ) ;
#24580 = DIRECTION ( 'NONE',  ( -3.009274222672345096E-17, -1.000000000000000000, 2.455023325076454960E-18 ) ) ;
#24581 = DIRECTION ( 'NONE',  ( -1.000000000000000000, -0.000000000000000000, 0.000000000000000000 ) ) ;
#24582 = ORIENTED_EDGE ( 'NONE', *, *, #1766, .F. ) ;
#24584 = ORIENTED_EDGE ( 'NONE', *, *, #9882, .F. ) ;
#24583 = CARTESIAN_POINT ( 'NONE',  ( 17.99999999999999645, -90.81729652456118629, -72.16798910853708549 ) ) ;
#24585 = CARTESIAN_POINT ( 'NONE',  ( 40.10317558968866081, 31.00000000000000355, -23.06553963618950931 ) ) ;
#24586 = DIRECTION ( 'NONE',  ( -1.000000000000000000, 0.000000000000000000, 0.000000000000000000 ) ) ;
#24588 = DIRECTION ( 'NONE',  ( -1.000000000000000000, 0.000000000000000000, 0.000000000000000000 ) ) ;
#24587 = CYLINDRICAL_SURFACE ( 'NONE', #11241, 47.49900000000000233 ) ;
#24589 = ORIENTED_EDGE ( 'NONE', *, *, #16164, .F. ) ;
#24590 = AXIS2_PLACEMENT_3D ( 'NONE', #9594, #13104, #6509 ) ;
#24591 = CARTESIAN_POINT ( 'NONE',  ( 17.99999999999999645, 0.000000000000000000, 0.000000000000000000 ) ) ;
#24592 = CARTESIAN_POINT ( 'NONE',  ( -50.06114249711410480, 40.00000000000000000, -38.53249520213266521 ) ) ;
#24593 = AXIS2_PLACEMENT_3D ( 'NONE', #22794, #13384, #29965 ) ;
#24594 = DIRECTION ( 'NONE',  ( 0.000000000000000000, 0.8747630845319591675, 0.4845508703326539823 ) ) ;
#24595 = AXIS2_PLACEMENT_3D ( 'NONE', #28107, #34846, #4959 ) ;
#24596 = EDGE_CURVE ( 'NONE', #38106, #30670, #30478, .T. ) ;
#24597 = CARTESIAN_POINT ( 'NONE',  ( 18.00000000000000355, 0.000000000000000000, 0.000000000000000000 ) ) ;
#24598 = ORIENTED_EDGE ( 'NONE', *, *, #40936, .T. ) ;
#24599 = DIRECTION ( 'NONE',  ( 0.000000000000000000, 0.000000000000000000, 1.000000000000000000 ) ) ;
#24600 = ORIENTED_EDGE ( 'NONE', *, *, #18176, .F. ) ;
#24601 = CIRCLE ( 'NONE', #32902, 1.000000000000000444 ) ;
#24602 = DIRECTION ( 'NONE',  ( 0.000000000000000000, 0.000000000000000000, -1.000000000000000000 ) ) ;
#24603 = CARTESIAN_POINT ( 'NONE',  ( 17.99999999999999645, -41.33768078145568836, 104.3046912715539918 ) ) ;
#24604 = CARTESIAN_POINT ( 'NONE',  ( 18.36587843422771016, 31.00000000000000355, 54.06640964556338957 ) ) ;
#24605 = CYLINDRICAL_SURFACE ( 'NONE', #15583, 116.0000000000000000 ) ;
#24606 = ORIENTED_EDGE ( 'NONE', *, *, #31018, .T. ) ;
#24607 = ADVANCED_FACE ( 'NONE', ( #22855, #16280 ), #27327, .T. ) ;
#24608 = EDGE_CURVE ( 'NONE', #6919, #23668, #37340, .T. ) ;
#24609 = CARTESIAN_POINT ( 'NONE',  ( 8.999999999999998224, 115.9750404417044081, 2.406240749597859718 ) ) ;
#24610 = ORIENTED_EDGE ( 'NONE', *, *, #19160, .F. ) ;
#24611 = CARTESIAN_POINT ( 'NONE',  ( -2.127120017302697619, 40.00000000000000000, -32.39583333539214038 ) ) ;
#24612 = EDGE_CURVE ( 'NONE', #25122, #4616, #38019, .T. ) ;
#24613 = VERTEX_POINT ( 'NONE', #39793 ) ;
#24614 = CARTESIAN_POINT ( 'NONE',  ( -132.0000507999999968, 9.184850993605147944E-16, -7.500000000000000000 ) ) ;
#24615 = DIRECTION ( 'NONE',  ( 1.000000000000000000, -0.000000000000000000, -0.000000000000000000 ) ) ;
#24616 = CARTESIAN_POINT ( 'NONE',  ( -60.98551593175036345, 31.00000000000000711, 53.34359504441579247 ) ) ;
#24617 = CARTESIAN_POINT ( 'NONE',  ( -5.410573124821300262, 40.00000000000000000, -84.40011308931431699 ) ) ;
#24618 = CARTESIAN_POINT ( 'NONE',  ( 0.000000000000000000, 0.000000000000000000, 0.000000000000000000 ) ) ;
#24619 = AXIS2_PLACEMENT_3D ( 'NONE', #8673, #34648, #38136 ) ;
#24620 = VERTEX_POINT ( 'NONE', #6222 ) ;
#24621 = DIRECTION ( 'NONE',  ( 0.000000000000000000, 0.9968120070307500136, 0.07978610555308653096 ) ) ;
#24622 = ORIENTED_EDGE ( 'NONE', *, *, #36251, .T. ) ;
#24623 = DIRECTION ( 'NONE',  ( 0.000000000000000000, 0.000000000000000000, 1.000000000000000000 ) ) ;
#24624 = CARTESIAN_POINT ( 'NONE',  ( 17.99999999999999645, -27.24480646643618442, 15.80846360676574669 ) ) ;
#24625 = AXIS2_PLACEMENT_3D ( 'NONE', #32905, #19430, #6491 ) ;
#24627 = ORIENTED_EDGE ( 'NONE', *, *, #24244, .T. ) ;
#24626 = DIRECTION ( 'NONE',  ( 1.058513553088275437E-16, 1.000000000000000000, -8.813324511995299047E-17 ) ) ;
#24628 = CARTESIAN_POINT ( 'NONE',  ( -20.39032260654148132, 17.11489954122026447, 1.150830359615497844 ) ) ;
#24629 = ORIENTED_EDGE ( 'NONE', *, *, #40403, .F. ) ;
#24630 = DIRECTION ( 'NONE',  ( 1.000000000000000000, 0.000000000000000000, 0.000000000000000000 ) ) ;
#24631 = CARTESIAN_POINT ( 'NONE',  ( -25.38139813252123034, 40.00000000000000000, 94.78629358389331117 ) ) ;
#24632 = CARTESIAN_POINT ( 'NONE',  ( 6.075999999999990742, 19.11698000000008335, 0.000000000000000000 ) ) ;
#24633 = EDGE_CURVE ( 'NONE', #14673, #2894, #29081, .T. ) ;
#24634 = VECTOR ( 'NONE', #18132, 1000.000000000000000 ) ;
#24635 = EDGE_LOOP ( 'NONE', ( #28576, #26057, #42523, #18904 ) ) ;
#24636 = DIRECTION ( 'NONE',  ( 0.000000000000000000, -7.709882115452474222E-16, -1.000000000000000000 ) ) ;
#24637 = CARTESIAN_POINT ( 'NONE',  ( -10.00000000000000000, 0.000000000000000000, 0.000000000000000000 ) ) ;
#24639 = CARTESIAN_POINT ( 'NONE',  ( 0.000000000000000000, 0.000000000000000000, 0.000000000000000000 ) ) ;
#24638 = CARTESIAN_POINT ( 'NONE',  ( 17.99999999999999645, 120.3696465864706937, -5.624871700594833435 ) ) ;
#24640 = ORIENTED_EDGE ( 'NONE', *, *, #9276, .F. ) ;
#24641 = CARTESIAN_POINT ( 'NONE',  ( -10.00000000000000000, 0.000000000000000000, 0.000000000000000000 ) ) ;
#24642 = VERTEX_POINT ( 'NONE', #26517 ) ;
#24643 = CARTESIAN_POINT ( 'NONE',  ( 0.000000000000000000, -25.61928775981012762, -45.25098998563503727 ) ) ;
#24644 = CARTESIAN_POINT ( 'NONE',  ( -1.974796425974089331, 40.00000000000000000, 29.60085432090885149 ) ) ;
#24645 = CARTESIAN_POINT ( 'NONE',  ( 18.00000000000000355, 0.000000000000000000, 0.000000000000000000 ) ) ;
#24646 = CARTESIAN_POINT ( 'NONE',  ( 17.99999999999999645, -31.94619804602776725, 16.59639811537345366 ) ) ;
#24647 = LINE ( 'NONE', #7376, #19964 ) ;
#24648 = ORIENTED_EDGE ( 'NONE', *, *, #8211, .F. ) ;
#24650 = CARTESIAN_POINT ( 'NONE',  ( 3.522875095019493141, -2.820352903225631369, -3.598441714920572299 ) ) ;
#24649 = DIRECTION ( 'NONE',  ( 1.000000000000000000, 0.000000000000000000, 0.000000000000000000 ) ) ;
#24651 = EDGE_CURVE ( 'NONE', #9154, #42975, #36311, .T. ) ;
#24652 = ORIENTED_EDGE ( 'NONE', *, *, #11673, .F. ) ;
#24653 = CONICAL_SURFACE ( 'NONE', #14894, 4.000000000000000000, 0.8911886515913786111 ) ;
#24654 = DIRECTION ( 'NONE',  ( 1.000000000000000000, 0.000000000000000000, 0.000000000000000000 ) ) ;
#24655 = DIRECTION ( 'NONE',  ( 0.000000000000000000, 0.000000000000000000, -1.000000000000000000 ) ) ;
#24656 = CARTESIAN_POINT ( 'NONE',  ( 24.63052733448982323, 31.00000000000000355, -3.251868155982907904 ) ) ;
#24657 = EDGE_LOOP ( 'NONE', ( #11759, #6437, #4312, #6664 ) ) ;
#24658 = CYLINDRICAL_SURFACE ( 'NONE', #30857, 116.0000000000000000 ) ;
#24659 = DIRECTION ( 'NONE',  ( 0.000000000000000000, 0.000000000000000000, 1.000000000000000000 ) ) ;
#24660 = CONTEXT_DEPENDENT_SHAPE_REPRESENTATION ( #234, #18361 ) ;
#24661 = ADVANCED_FACE ( 'NONE', ( #16510 ), #9919, .T. ) ;
#24662 = DIRECTION ( 'NONE',  ( -1.000000000000000000, 0.000000000000000000, 0.000000000000000000 ) ) ;
#24663 = CARTESIAN_POINT ( 'NONE',  ( 75.74279358916429317, 31.00000000000000000, -37.35102017232331661 ) ) ;
#24664 = AXIS2_PLACEMENT_3D ( 'NONE', #40688, #10838, #20913 ) ;
#24665 = ORIENTED_EDGE ( 'NONE', *, *, #26802, .T. ) ;
#24666 = CARTESIAN_POINT ( 'NONE',  ( -19.43072497042362556, 31.00000000000000355, 56.92208038676059800 ) ) ;
#24667 = EDGE_CURVE ( 'NONE', #21935, #27712, #26989, .T. ) ;
#24668 = CARTESIAN_POINT ( 'NONE',  ( 61.87885091699251916, 39.99999999999999289, -70.55635664373320992 ) ) ;
#24669 = VERTEX_POINT ( 'NONE', #30607 ) ;
#24670 = DIRECTION ( 'NONE',  ( 0.000000000000000000, 0.8477344278896721264, -0.5304209081197406306 ) ) ;
#24671 = CYLINDRICAL_SURFACE ( 'NONE', #35400, 25.00000000000002132 ) ;
#24672 = CIRCLE ( 'NONE', #27448, 31.49899999999999523 ) ;
#24673 = CARTESIAN_POINT ( 'NONE',  ( 17.99999999999999645, -11.41303419185048185, 111.6154788735835410 ) ) ;
#24674 = AXIS2_PLACEMENT_3D ( 'NONE', #29562, #25676, #32394 ) ;
#24676 = VERTEX_POINT ( 'NONE', #14035 ) ;
#24675 = CARTESIAN_POINT ( 'NONE',  ( -91.96080130434573618, -35.35525454449571470, 14.45886780445633946 ) ) ;
#24677 = CARTESIAN_POINT ( 'NONE',  ( 17.99999999999999645, -66.49630760163661591, 90.36876423295966276 ) ) ;
#24678 = CARTESIAN_POINT ( 'NONE',  ( -10.00000000000000000, 0.000000000000000000, 0.000000000000000000 ) ) ;
#24679 = AXIS2_PLACEMENT_3D ( 'NONE', #39475, #39682, #15971 ) ;
#24680 = VERTEX_POINT ( 'NONE', #40594 ) ;
#24681 = CARTESIAN_POINT ( 'NONE',  ( 65.10416666562252885, 39.99999999999999289, 4.254240043327690124 ) ) ;
#24682 = FACE_OUTER_BOUND ( 'NONE', #20450, .T. ) ;
#24683 = EDGE_CURVE ( 'NONE', #10297, #31034, #2566, .T. ) ;
#24684 = EDGE_LOOP ( 'NONE', ( #38850, #17071 ) ) ;
#24685 = EDGE_CURVE ( 'NONE', #31744, #10857, #12921, .T. ) ;
#24686 = FACE_OUTER_BOUND ( 'NONE', #20392, .T. ) ;
#24687 = DIRECTION ( 'NONE',  ( 0.000000000000000000, 0.000000000000000000, 1.000000000000000000 ) ) ;
#24688 = ORIENTED_EDGE ( 'NONE', *, *, #7875, .T. ) ;
#24689 = CARTESIAN_POINT ( 'NONE',  ( 17.99999999999999645, 0.000000000000000000, 0.000000000000000000 ) ) ;
#24690 = ORIENTED_EDGE ( 'NONE', *, *, #22140, .T. ) ;
#24691 = CARTESIAN_POINT ( 'NONE',  ( 17.99999999999999645, -29.02167576844032482, -108.3790330702172611 ) ) ;
#24692 = VECTOR ( 'NONE', #32189, 1000.000000000000227 ) ;
#24693 = ORIENTED_EDGE ( 'NONE', *, *, #24174, .F. ) ;
#24694 = LINE ( 'NONE', #18375, #36938 ) ;
#24695 = CARTESIAN_POINT ( 'NONE',  ( 31.77777543000702565, 31.00000000000000355, 93.95825142778512884 ) ) ;
#24696 = VERTEX_POINT ( 'NONE', #36437 ) ;
#24697 = DIRECTION ( 'NONE',  ( 0.000000000000000000, -0.7980172272802447120, 0.6026346363792492999 ) ) ;
#24698 = CARTESIAN_POINT ( 'NONE',  ( 18.00000000000000355, -42.60732521687585006, 19.80331771201644031 ) ) ;
#24699 = ORIENTED_EDGE ( 'NONE', *, *, #7349, .F. ) ;
#24700 = CARTESIAN_POINT ( 'NONE',  ( 17.99999999999999645, -116.4607004671430417, 30.94182036827165660 ) ) ;
#24701 = EDGE_CURVE ( 'NONE', #42903, #35448, #15997, .T. ) ;
#24702 = DIRECTION ( 'NONE',  ( 0.000000000000000000, -0.8993121301712141413, -0.4373073204588656671 ) ) ;
#24703 = ORIENTED_EDGE ( 'NONE', *, *, #2791, .T. ) ;
#24704 = CARTESIAN_POINT ( 'NONE',  ( 17.99999999999999645, 0.000000000000000000, 0.000000000000000000 ) ) ;
#24705 = AXIS2_PLACEMENT_3D ( 'NONE', #29677, #42951, #35748 ) ;
#24706 = DIRECTION ( 'NONE',  ( 0.000000000000000000, -0.9826841245925227453, 0.1852887240871045338 ) ) ;
#24707 = ORIENTED_EDGE ( 'NONE', *, *, #27373, .F. ) ;
#24708 = PRODUCT_CONTEXT ( 'NONE', #3559, 'mechanical' ) ;
#24709 = EDGE_CURVE ( 'NONE', #27433, #29671, #24842, .T. ) ;
#24711 = CIRCLE ( 'NONE', #30255, 59.00000000000000711 ) ;
#24710 = CARTESIAN_POINT ( 'NONE',  ( 9.000000000000001776, -12.30077720129062868, -50.52416135122093976 ) ) ;
#24712 = CARTESIAN_POINT ( 'NONE',  ( 48.77780477658175329, 31.00000000000000355, -24.05648398140741406 ) ) ;
#24713 = ORIENTED_EDGE ( 'NONE', *, *, #34794, .F. ) ;
#24715 = LINE ( 'NONE', #1100, #20613 ) ;
#24714 = FACE_OUTER_BOUND ( 'NONE', #38979, .T. ) ;
#24716 = EDGE_CURVE ( 'NONE', #6315, #23930, #19351, .T. ) ;
#24717 = DIRECTION ( 'NONE',  ( -1.000000000000000000, 0.000000000000000000, -0.000000000000000000 ) ) ;
#24718 = ORIENTED_EDGE ( 'NONE', *, *, #31071, .F. ) ;
#24719 = EDGE_CURVE ( 'NONE', #8862, #13944, #11577, .T. ) ;
#24720 = CARTESIAN_POINT ( 'NONE',  ( -10.00000000000000000, 0.000000000000000000, 0.000000000000000000 ) ) ;
#24721 = CARTESIAN_POINT ( 'NONE',  ( 57.76613438074698337, 39.99999999999999289, -28.48799604501563110 ) ) ;
#24722 = AXIS2_PLACEMENT_3D ( 'NONE', #22093, #42090, #25570 ) ;
#24723 = CARTESIAN_POINT ( 'NONE',  ( -53.12901929299007975, 40.00000000000000000, 30.56653509229933263 ) ) ;
#24724 = CIRCLE ( 'NONE', #30262, 51.99999999999999289 ) ;
#24725 = DIRECTION ( 'NONE',  ( 1.000000000000000000, -1.373900992973641868E-15, -6.546126324440886161E-16 ) ) ;
#24726 = CARTESIAN_POINT ( 'NONE',  ( 0.000000000000000000, -114.8812324315174038, -16.07179003769265080 ) ) ;
#24727 = FACE_OUTER_BOUND ( 'NONE', #28094, .T. ) ;
#24728 = AXIS2_PLACEMENT_3D ( 'NONE', #24691, #37948, #34689 ) ;
#24729 = CARTESIAN_POINT ( 'NONE',  ( 17.99999999999999645, 0.000000000000000000, 0.000000000000000000 ) ) ;
#24730 = AXIS2_PLACEMENT_3D ( 'NONE', #1955, #28810, #35335 ) ;
#24731 = ORIENTED_EDGE ( 'NONE', *, *, #9813, .F. ) ;
#24732 = CARTESIAN_POINT ( 'NONE',  ( -29.44516979616424024, 40.00000000000000000, -7.879824757621473275 ) ) ;
#24733 = ORIENTED_EDGE ( 'NONE', *, *, #12084, .T. ) ;
#24734 = CARTESIAN_POINT ( 'NONE',  ( 0.000000000000000000, 8.053585752062561554, -46.81126742072013514 ) ) ;
#24735 = CYLINDRICAL_SURFACE ( 'NONE', #2593, 13.59999999999999787 ) ;
#24736 = VECTOR ( 'NONE', #41999, 1000.000000000000000 ) ;
#24737 = EDGE_CURVE ( 'NONE', #43113, #18362, #17163, .T. ) ;
#24738 = ORIENTED_EDGE ( 'NONE', *, *, #31738, .T. ) ;
#24739 = ADVANCED_FACE ( 'NONE', ( #29719 ), #2410, .F. ) ;
#24740 = CARTESIAN_POINT ( 'NONE',  ( -0.2142857142857142738, -10.49781318335647917, -1.199999999999999956 ) ) ;
#24741 = EDGE_CURVE ( 'NONE', #23020, #25565, #6072, .T. ) ;
#24742 = EDGE_CURVE ( 'NONE', #40515, #17655, #22845, .T. ) ;
#24743 = CIRCLE ( 'NONE', #5875, 20.00000000000001066 ) ;
#24744 = DIRECTION ( 'NONE',  ( 0.000000000000000000, 0.000000000000000000, 1.000000000000000000 ) ) ;
#24745 = ORIENTED_EDGE ( 'NONE', *, *, #7125, .T. ) ;
#24746 = CARTESIAN_POINT ( 'NONE',  ( 0.2500000000000002220, 0.000000000000000000, 0.000000000000000000 ) ) ;
#24747 = ORIENTED_EDGE ( 'NONE', *, *, #26192, .F. ) ;
#24748 = CIRCLE ( 'NONE', #3044, 116.0000000000000000 ) ;
#24749 = ORIENTED_EDGE ( 'NONE', *, *, #17198, .F. ) ;
#24750 = CARTESIAN_POINT ( 'NONE',  ( 17.99999999999999645, -35.78484819117709748, 110.3423972910431701 ) ) ;
#24751 = CARTESIAN_POINT ( 'NONE',  ( 47.76959191294547225, 31.00000000000000355, 62.44753968350421047 ) ) ;
#24752 = VERTEX_POINT ( 'NONE', #3276 ) ;
#24753 = CARTESIAN_POINT ( 'NONE',  ( -10.00000000000000000, 0.000000000000000000, 0.000000000000000000 ) ) ;
#24754 = DIRECTION ( 'NONE',  ( -1.000000000000000000, 0.000000000000000000, 0.000000000000000000 ) ) ;
#24755 = ORIENTED_EDGE ( 'NONE', *, *, #4094, .F. ) ;
#24756 = VERTEX_POINT ( 'NONE', #22552 ) ;
#24758 = AXIS2_PLACEMENT_3D ( 'NONE', #11223, #28244, #18029 ) ;
#24757 = DIRECTION ( 'NONE',  ( -1.000000000000000000, 0.000000000000000000, 0.000000000000000000 ) ) ;
#24759 = ORIENTED_EDGE ( 'NONE', *, *, #9139, .F. ) ;
#24760 = CARTESIAN_POINT ( 'NONE',  ( 96.17895579825814423, 39.99999999999999289, -12.55124642863780338 ) ) ;
#24761 = CARTESIAN_POINT ( 'NONE',  ( -101.9001375415117963, 40.00000000000000711, 6.549163350515033066 ) ) ;
#24763 = PLANE ( 'NONE',  #15187 ) ;
#24762 = CARTESIAN_POINT ( 'NONE',  ( 0.000000000000000000, 97.19627249181192497, -71.22763238166385236 ) ) ;
#24764 = CARTESIAN_POINT ( 'NONE',  ( 18.00000000000000355, 38.92705108641732892, 27.21837053747810842 ) ) ;
#24765 = DIRECTION ( 'NONE',  ( -3.009274222672345096E-17, -1.000000000000000000, 2.455023325076454960E-18 ) ) ;
#24766 = CIRCLE ( 'NONE', #17090, 120.5010000000000332 ) ;
#24767 = EDGE_LOOP ( 'NONE', ( #4332, #699, #38744, #21499 ) ) ;
#24768 = EDGE_CURVE ( 'NONE', #39935, #16661, #28411, .T. ) ;
#24769 = ORIENTED_EDGE ( 'NONE', *, *, #26411, .T. ) ;
#24770 = CIRCLE ( 'NONE', #6577, 10.49999999999999467 ) ;
#24771 = CARTESIAN_POINT ( 'NONE',  ( 0.000000000000000000, -30.74337109795225942, 8.695908345466005329 ) ) ;
#24772 = CARTESIAN_POINT ( 'NONE',  ( -89.22528799552154055, 31.00000000000000711, 43.99828826784794700 ) ) ;
#24773 = EDGE_CURVE ( 'NONE', #6952, #30129, #39503, .T. ) ;
#24774 = DIRECTION ( 'NONE',  ( -0.000000000000000000, -0.000000000000000000, 1.000000000000000000 ) ) ;
#24775 = ORIENTED_EDGE ( 'NONE', *, *, #4245, .T. ) ;
#24776 = AXIS2_PLACEMENT_3D ( 'NONE', #4715, #1646, #18732 ) ;
#24777 = CARTESIAN_POINT ( 'NONE',  ( -7.793954689940647995, 40.00000000000000000, 28.94896179907301459 ) ) ;
#24778 = VERTEX_POINT ( 'NONE', #35791 ) ;
#24779 = ORIENTED_EDGE ( 'NONE', *, *, #16506, .T. ) ;
#24780 = FACE_OUTER_BOUND ( 'NONE', #25715, .T. ) ;
#24781 = CARTESIAN_POINT ( 'NONE',  ( 17.99999999999999645, 0.000000000000000000, 0.000000000000000000 ) ) ;
#24782 = DIRECTION ( 'NONE',  ( -1.770125995894701942E-16, 1.000000000000000000, 0.000000000000000000 ) ) ;
#24783 = DIRECTION ( 'NONE',  ( 1.000000000000000000, 0.000000000000000000, 0.000000000000000000 ) ) ;
#24784 = AXIS2_PLACEMENT_3D ( 'NONE', #38245, #28670, #8151 ) ;
#24785 = ORIENTED_EDGE ( 'NONE', *, *, #3638, .F. ) ;
#24786 = DIRECTION ( 'NONE',  ( -1.000000000000000000, -0.000000000000000000, 0.000000000000000000 ) ) ;
#24787 = ORIENTED_EDGE ( 'NONE', *, *, #6249, .T. ) ;
#24788 = CARTESIAN_POINT ( 'NONE',  ( 18.00000000000000355, -17.08890430202718491, -43.76671000081963570 ) ) ;
#24789 = DIRECTION ( 'NONE',  ( 1.000000000000000000, 0.000000000000000000, 0.000000000000000000 ) ) ;
#24790 = EDGE_CURVE ( 'NONE', #23539, #39668, #19280, .T. ) ;
#24791 = CARTESIAN_POINT ( 'NONE',  ( 18.00000000000000355, -13.85708833599999856, 45.43276465116660745 ) ) ;
#24792 = EDGE_CURVE ( 'NONE', #18000, #30690, #2838, .T. ) ;
#24793 = ADVANCED_FACE ( 'NONE', ( #39277 ), #35592, .T. ) ;
#24794 = AXIS2_PLACEMENT_3D ( 'NONE', #21554, #14762, #11476 ) ;
#24795 = DIRECTION ( 'NONE',  ( 1.000000000000000000, 0.000000000000000000, 0.000000000000000000 ) ) ;
#24796 = VERTEX_POINT ( 'NONE', #5712 ) ;
#24797 = AXIS2_PLACEMENT_3D ( 'NONE', #2800, #32089, #12883 ) ;
#24798 = EDGE_LOOP ( 'NONE', ( #23150, #13091 ) ) ;
#24799 = CYLINDRICAL_SURFACE ( 'NONE', #41195, 116.0000000000000000 ) ;
#24800 = CIRCLE ( 'NONE', #22025, 36.00000000000000000 ) ;
#24801 = DIRECTION ( 'NONE',  ( -1.000000000000000000, 1.373900992973642263E-15, 0.000000000000000000 ) ) ;
#24802 = EDGE_CURVE ( 'NONE', #9440, #36558, #40811, .T. ) ;
#24803 = ORIENTED_EDGE ( 'NONE', *, *, #8126, .T. ) ;
#24804 = AXIS2_PLACEMENT_3D ( 'NONE', #25321, #24903, #32256 ) ;
#24806 = ORIENTED_EDGE ( 'NONE', *, *, #32788, .T. ) ;
#24805 = CARTESIAN_POINT ( 'NONE',  ( 18.00000000000000355, 5.667686777402355602, -46.64153600743599526 ) ) ;
#24807 = CARTESIAN_POINT ( 'NONE',  ( -2.829072032612243159, 31.00000000000000355, -44.39959014221899025 ) ) ;
#24808 = AXIS2_PLACEMENT_3D ( 'NONE', #23839, #30361, #1270 ) ;
#24809 = CARTESIAN_POINT ( 'NONE',  ( 0.000000000000000000, 11.49545354908979888, -29.80986809967247453 ) ) ;
#24810 = AXIS2_PLACEMENT_3D ( 'NONE', #30434, #30652, #13431 ) ;
#24812 = LINE ( 'NONE', #11916, #5220 ) ;
#24811 = FACE_OUTER_BOUND ( 'NONE', #30971, .T. ) ;
#24813 = VECTOR ( 'NONE', #8383, 1000.000000000000000 ) ;
#24814 = ORIENTED_EDGE ( 'NONE', *, *, #39936, .F. ) ;
#24815 = CYLINDRICAL_SURFACE ( 'NONE', #32453, 20.00000000000000711 ) ;
#24816 = CARTESIAN_POINT ( 'NONE',  ( -62.09442273004785307, 40.00000000000000711, -4.163950221635984938 ) ) ;
#24817 = DIRECTION ( 'NONE',  ( 1.000000000000000000, -1.373900992973642263E-15, -3.996523416598957436E-16 ) ) ;
#24818 = CARTESIAN_POINT ( 'NONE',  ( 0.000000000000000000, -29.68570942776479527, 10.53307442156924267 ) ) ;
#24819 = ORIENTED_EDGE ( 'NONE', *, *, #20817, .T. ) ;
#24820 = CARTESIAN_POINT ( 'NONE',  ( 17.99999999999999645, 56.51398178981952469, -96.92493144647394843 ) ) ;
#24821 = ORIENTED_EDGE ( 'NONE', *, *, #21003, .F. ) ;
#24822 = VECTOR ( 'NONE', #18876, 1000.000000000000000 ) ;
#24823 = CARTESIAN_POINT ( 'NONE',  ( 0.000000000000000000, 25.52601536738592358, 19.21447964122706509 ) ) ;
#24824 = DIRECTION ( 'NONE',  ( -1.000000000000000000, 0.000000000000000000, 0.000000000000000000 ) ) ;
#24825 = CARTESIAN_POINT ( 'NONE',  ( 42.05404839982585941, 31.00000000000000355, -47.95475229022623864 ) ) ;
#24826 = CYLINDRICAL_SURFACE ( 'NONE', #24664, 20.00000000000000355 ) ;
#24827 = AXIS2_PLACEMENT_3D ( 'NONE', #17135, #5076, #8782 ) ;
#24828 = ORIENTED_EDGE ( 'NONE', *, *, #12294, .F. ) ;
#24829 = VECTOR ( 'NONE', #41818, 1000.000000000000000 ) ;
#24830 = EDGE_CURVE ( 'NONE', #35106, #4068, #16204, .T. ) ;
#24831 = AXIS2_PLACEMENT_3D ( 'NONE', #36884, #6989, #26653 ) ;
#24832 = AXIS2_PLACEMENT_3D ( 'NONE', #21466, #4601, #14026 ) ;
#24833 = CYLINDRICAL_SURFACE ( 'NONE', #27515, 120.5010000000000190 ) ;
#24834 = VECTOR ( 'NONE', #27226, 1000.000000000000000 ) ;
#24835 = VERTEX_POINT ( 'NONE', #19699 ) ;
#24837 = VECTOR ( 'NONE', #36999, 1000.000000000000000 ) ;
#24836 = CARTESIAN_POINT ( 'NONE',  ( 17.99999999999999645, 120.3696465864706227, 5.624871700596478341 ) ) ;
#24838 = LINE ( 'NONE', #38092, #36629 ) ;
#24839 = CARTESIAN_POINT ( 'NONE',  ( 27.50146173783093317, 31.00000000000000355, -80.63904244945182143 ) ) ;
#24841 = CARTESIAN_POINT ( 'NONE',  ( 5.650912336215121456, 40.00000000000000000, -84.59266001511657862 ) ) ;
#24840 = CIRCLE ( 'NONE', #5971, 158.4999999999992042 ) ;
#24842 = CIRCLE ( 'NONE', #5972, 58.99999999999999289 ) ;
#24843 = DIRECTION ( 'NONE',  ( 1.000000000000000000, 0.000000000000000000, 0.000000000000000000 ) ) ;
#24844 = VECTOR ( 'NONE', #6716, 1000.000000000000000 ) ;
#24845 = ORIENTED_EDGE ( 'NONE', *, *, #26157, .T. ) ;
#24846 = DIRECTION ( 'NONE',  ( -1.000000000000000000, -0.000000000000000000, 0.000000000000000000 ) ) ;
#24847 = ORIENTED_EDGE ( 'NONE', *, *, #36023, .F. ) ;
#24848 = FACE_OUTER_BOUND ( 'NONE', #6701, .T. ) ;
#24849 = DIRECTION ( 'NONE',  ( 1.000000000000000000, 0.000000000000000000, 0.000000000000000000 ) ) ;
#24851 = ORIENTED_EDGE ( 'NONE', *, *, #41388, .F. ) ;
#24850 = DIRECTION ( 'NONE',  ( -1.000000000000000000, -0.000000000000000000, -0.000000000000000000 ) ) ;
#24852 = EDGE_CURVE ( 'NONE', #26713, #42086, #32966, .T. ) ;
#24853 = DIRECTION ( 'NONE',  ( 0.3211947320043963550, 0.000000000000000000, -0.9470131699890049770 ) ) ;
#24854 = EDGE_LOOP ( 'NONE', ( #41737, #34339, #14925, #27956 ) ) ;
#24855 = CARTESIAN_POINT ( 'NONE',  ( 17.99999999999999645, 0.000000000000000000, 0.000000000000000000 ) ) ;
#24856 = EDGE_CURVE ( 'NONE', #24796, #35008, #14382, .T. ) ;
#24857 = CARTESIAN_POINT ( 'NONE',  ( -65.18298466990795248, 40.00000000000000711, 74.32329070269128124 ) ) ;
#24858 = CARTESIAN_POINT ( 'NONE',  ( -147.8500000000000227, -5.254679414958916394E-13, 10.00000000000000000 ) ) ;
#24859 = EDGE_LOOP ( 'NONE', ( #33654, #25552, #31720, #10980 ) ) ;
#24860 = DIRECTION ( 'NONE',  ( -1.000000000000000000, 0.000000000000000000, 0.000000000000000000 ) ) ;
#24861 = FACE_OUTER_BOUND ( 'NONE', #6576, .T. ) ;
#24862 = AXIS2_PLACEMENT_3D ( 'NONE', #9048, #22401, #19123 ) ;
#24863 = CIRCLE ( 'NONE', #35939, 20.00000000000000711 ) ;
#24864 = AXIS2_PLACEMENT_3D ( 'NONE', #21868, #2356, #35117 ) ;
#24865 = EDGE_CURVE ( 'NONE', #40994, #18274, #30413, .T. ) ;
#24866 = AXIS2_PLACEMENT_3D ( 'NONE', #38305, #31781, #994 ) ;
#24868 = DIRECTION ( 'NONE',  ( 0.000000000000000000, -0.2113826236296114103, -0.9774033898178695612 ) ) ;
#24867 = CARTESIAN_POINT ( 'NONE',  ( 17.99999999999999645, 0.000000000000000000, 0.000000000000000000 ) ) ;
#24869 = ORIENTED_EDGE ( 'NONE', *, *, #5045, .F. ) ;
#24870 = CARTESIAN_POINT ( 'NONE',  ( 0.000000000000000000, 0.000000000000000000, 0.000000000000000000 ) ) ;
#24871 = VERTEX_POINT ( 'NONE', #30358 ) ;
#24872 = CARTESIAN_POINT ( 'NONE',  ( 17.99999999999999645, -52.19040376560366923, -99.31985817764231683 ) ) ;
#24873 = CARTESIAN_POINT ( 'NONE',  ( 31.41502175087570947, 40.00000000000000000, -18.07270130326806523 ) ) ;
#24874 = AXIS2_PLACEMENT_3D ( 'NONE', #41741, #8371, #11885 ) ;
#24875 = DIRECTION ( 'NONE',  ( -1.000000000000000000, 0.000000000000000000, 0.000000000000000000 ) ) ;
#24876 = ADVANCED_FACE ( 'NONE', ( #26868 ), #13803, .T. ) ;
#24877 = CIRCLE ( 'NONE', #32479, 25.00000000000002132 ) ;
#24878 = CIRCLE ( 'NONE', #6687, 116.0000000000000000 ) ;
#24879 = CARTESIAN_POINT ( 'NONE',  ( 0.000000000000000000, 0.000000000000000000, -25.03750572909317285 ) ) ;
#24880 = CIRCLE ( 'NONE', #15782, 139.5000000000000000 ) ;
#24881 = DIRECTION ( 'NONE',  ( 0.000000000000000000, 0.000000000000000000, 1.000000000000000000 ) ) ;
#24882 = ORIENTED_EDGE ( 'NONE', *, *, #7080, .F. ) ;
#24884 = CARTESIAN_POINT ( 'NONE',  ( 0.5276280594147412240, -4.314175951381924889, -3.320322319201654881 ) ) ;
#24883 = CARTESIAN_POINT ( 'NONE',  ( 9.000000000000001776, 0.6819280456829140968, 115.9979955608738749 ) ) ;
#24885 = ORIENTED_EDGE ( 'NONE', *, *, #1250, .F. ) ;
#24886 = DIRECTION ( 'NONE',  ( -3.614007241618348771E-16, 1.000000000000000000, 0.000000000000000000 ) ) ;
#24887 = CYLINDRICAL_SURFACE ( 'NONE', #21999, 51.99999999999999289 ) ;
#24888 = CARTESIAN_POINT ( 'NONE',  ( 3.579113344806025054, 31.00000000000000355, 27.11441211503905535 ) ) ;
#24889 = ORIENTED_EDGE ( 'NONE', *, *, #17424, .F. ) ;
#24890 = FACE_OUTER_BOUND ( 'NONE', #9109, .T. ) ;
#24891 =( BOUNDED_SURFACE ( )  B_SPLINE_SURFACE ( 3, 2, ( 
 ( #15041, #1265, #34861 ),
 ( #24884, #22027, #34646 ),
 ( #4976, #18547, #37694 ),
 ( #5407, #41387, #28351 ),
 ( #38343, #11321, #24650 ),
 ( #37906, #21398, #18775 ) ),
 .UNSPECIFIED., .F., .F., .F. ) 
 B_SPLINE_SURFACE_WITH_KNOTS ( ( 4, 2, 4 ),
 ( 3, 3 ),
 ( 0.02032853247518126918, 0.02278863295364821906, 0.02524873343211517240 ),
 ( 0.000000000000000000, 1.000000000000000000 ),
 .UNSPECIFIED. ) 
 GEOMETRIC_REPRESENTATION_ITEM ( )  RATIONAL_B_SPLINE_SURFACE ( (
 ( 1.000000000000000000, 0.8047781615896837382, 1.000000000000000000),
 ( 1.000000000000000000, 0.8123767586289252218, 1.000000000000000000),
 ( 1.000000000000000000, 0.8190662415564388121, 1.000000000000000000),
 ( 1.000000000000000000, 0.8192361015669026303, 1.000000000000000000),
 ( 1.000000000000000000, 0.8126135807103900266, 1.000000000000000000),
 ( 1.000000000000000000, 0.8047712338318593339, 1.000000000000000000) ) ) 
 REPRESENTATION_ITEM ( '' )  SURFACE ( )  );
#24892 = CARTESIAN_POINT ( 'NONE',  ( 42.80287614962796994, -12.05525454449572464, 69.29271901957280022 ) ) ;
#24893 = CARTESIAN_POINT ( 'NONE',  ( 63.16980243745005907, 31.00000000000000000, -55.41789732285823078 ) ) ;
#24895 = ORIENTED_EDGE ( 'NONE', *, *, #28715, .T. ) ;
#24894 = AXIS2_PLACEMENT_3D ( 'NONE', #20102, #6510, #29087 ) ;
#24896 = CARTESIAN_POINT ( 'NONE',  ( 7.664524495375376389, 31.00000000000000355, 58.91906827746952757 ) ) ;
#24897 = CARTESIAN_POINT ( 'NONE',  ( 52.74436945453300041, 40.00000000000000000, 68.73989242669851762 ) ) ;
#24898 = AXIS2_PLACEMENT_3D ( 'NONE', #601, #17898, #31174 ) ;
#24899 = ORIENTED_EDGE ( 'NONE', *, *, #8717, .T. ) ;
#24900 = AXIS2_PLACEMENT_3D ( 'NONE', #17095, #13598, #34283 ) ;
#24901 = DIRECTION ( 'NONE',  ( 0.000000000000000000, 0.000000000000000000, 1.000000000000000000 ) ) ;
#24902 = DIRECTION ( 'NONE',  ( 1.000000000000000000, 0.000000000000000000, 0.000000000000000000 ) ) ;
#24903 = DIRECTION ( 'NONE',  ( -1.000000000000000000, 0.000000000000000000, 0.000000000000000000 ) ) ;
#24904 = CIRCLE ( 'NONE', #6038, 18.77999999999999048 ) ;
#24906 = EDGE_LOOP ( 'NONE', ( #8415, #30621, #23232, #35329 ) ) ;
#24905 = CARTESIAN_POINT ( 'NONE',  ( 17.99999999999999645, 0.000000000000000000, 0.000000000000000000 ) ) ;
#24907 = EDGE_CURVE ( 'NONE', #28617, #4417, #406, .T. ) ;
#24908 = CARTESIAN_POINT ( 'NONE',  ( 9.000000000000001776, -101.8011932243951634, 55.61040422519296555 ) ) ;
#24909 = DIRECTION ( 'NONE',  ( -1.000000000000000000, 0.000000000000000000, 0.000000000000000000 ) ) ;
#24910 = EDGE_CURVE ( 'NONE', #27725, #40723, #32484, .T. ) ;
#24911 = CIRCLE ( 'NONE', #17933, 59.00000000000000000 ) ;
#24912 = ORIENTED_EDGE ( 'NONE', *, *, #42382, .F. ) ;
#24913 = CARTESIAN_POINT ( 'NONE',  ( -46.07128526072433772, 40.00000000000000000, -40.40198152342698990 ) ) ;
#24914 = DIRECTION ( 'NONE',  ( 0.000000000000000000, 0.8951632913550604531, 0.4457383557765420834 ) ) ;
#24915 = AXIS2_PLACEMENT_3D ( 'NONE', #2056, #1415, #28293 ) ;
#24916 = ORIENTED_EDGE ( 'NONE', *, *, #15991, .T. ) ;
#24917 = LINE ( 'NONE', #28385, #14809 ) ;
#24918 = DIRECTION ( 'NONE',  ( -1.000000000000000000, 0.000000000000000000, -0.000000000000000000 ) ) ;
#24919 = ORIENTED_EDGE ( 'NONE', *, *, #13122, .T. ) ;
#24920 = DIRECTION ( 'NONE',  ( 0.000000000000000000, 0.4817536741017162116, -0.8763066800438631399 ) ) ;
#24921 = ORIENTED_EDGE ( 'NONE', *, *, #26069, .T. ) ;
#24922 = ADVANCED_FACE ( 'NONE', ( #33831, #3488 ), #6787, .T. ) ;
#24923 = DIRECTION ( 'NONE',  ( -1.000000000000000000, 0.000000000000000000, 0.000000000000000000 ) ) ;
#24924 = ORIENTED_EDGE ( 'NONE', *, *, #35237, .F. ) ;
#24925 = CYLINDRICAL_SURFACE ( 'NONE', #36240, 31.49899999999999878 ) ;
#24926 = DIRECTION ( 'NONE',  ( -0.000000000000000000, -0.000000000000000000, 1.000000000000000000 ) ) ;
#24927 = EDGE_CURVE ( 'NONE', #39541, #39644, #23454, .T. ) ;
#24928 = VECTOR ( 'NONE', #40288, 1000.000000000000000 ) ;
#24929 = CARTESIAN_POINT ( 'NONE',  ( -10.00000000000000000, 0.000000000000000000, 0.000000000000000000 ) ) ;
#24930 = CARTESIAN_POINT ( 'NONE',  ( 22.90854556226710415, -40.05525454449572464, -74.83297477053821467 ) ) ;
#24931 = ORIENTED_EDGE ( 'NONE', *, *, #2403, .F. ) ;
#24932 = AXIS2_PLACEMENT_3D ( 'NONE', #34987, #14733, #28040 ) ;
#24933 = DIRECTION ( 'NONE',  ( 0.000000000000000000, 0.000000000000000000, 1.000000000000000000 ) ) ;
#24934 = CIRCLE ( 'NONE', #40176, 59.00000000000000000 ) ;
#24936 = CARTESIAN_POINT ( 'NONE',  ( 18.00000000000000355, 44.25018368420742831, 27.31155879685195842 ) ) ;
#24935 = AXIS2_PLACEMENT_3D ( 'NONE', #30979, #5388, #18957 ) ;
#24937 = ORIENTED_EDGE ( 'NONE', *, *, #3080, .T. ) ;
#24938 = CARTESIAN_POINT ( 'NONE',  ( -1.600000000000000089, -12.75000000000000000, -1.199999999999999956 ) ) ;
#24939 = CIRCLE ( 'NONE', #34630, 20.00000000000000000 ) ;
#24940 = DIRECTION ( 'NONE',  ( 0.000000000000000000, 0.9574220383620062336, -0.2886919473396183933 ) ) ;
#24941 = DIRECTION ( 'NONE',  ( -4.329780281177428835E-17, 1.000000000000000000, 4.329780281177504023E-17 ) ) ;
#24942 = DIRECTION ( 'NONE',  ( 0.000000000000000000, 0.000000000000000000, 1.000000000000000000 ) ) ;
#24943 = CARTESIAN_POINT ( 'NONE',  ( -46.94946386092573221, 31.00000000000000355, 15.94926099647653928 ) ) ;
#24944 = EDGE_CURVE ( 'NONE', #28703, #11424, #23627, .T. ) ;
#24945 = ORIENTED_EDGE ( 'NONE', *, *, #35297, .F. ) ;
#24947 = CARTESIAN_POINT ( 'NONE',  ( 9.000000000000000000, 34.78944633786279184, 9.257128253673750251 ) ) ;
#24946 = DIRECTION ( 'NONE',  ( 0.000000000000000000, 0.000000000000000000, 1.000000000000000000 ) ) ;
#24948 = AXIS2_PLACEMENT_3D ( 'NONE', #18667, #31060, #7702 ) ;
#24949 = EDGE_CURVE ( 'NONE', #20926, #16254, #13696, .T. ) ;
#24950 = ORIENTED_EDGE ( 'NONE', *, *, #34726, .F. ) ;
#24951 = CARTESIAN_POINT ( 'NONE',  ( 0.000000000000000000, -72.00556975657644898, -86.04342158279462183 ) ) ;
#24952 = CARTESIAN_POINT ( 'NONE',  ( 44.56294422764113250, 40.00000000000000000, 34.17917587534974189 ) ) ;
#24953 = CARTESIAN_POINT ( 'NONE',  ( -23.74678488968044832, 40.00000000000000000, -48.36925102894097961 ) ) ;
#24954 = CARTESIAN_POINT ( 'NONE',  ( 42.80287614962723808, -35.35525454449572180, 69.29271901957299917 ) ) ;
#24955 = DIRECTION ( 'NONE',  ( -1.000000000000000000, 0.000000000000000000, 0.000000000000000000 ) ) ;
#24956 = CIRCLE ( 'NONE', #27701, 2.055000000000000160 ) ;
#24957 = CYLINDRICAL_SURFACE ( 'NONE', #26168, 13.59999999999999964 ) ;
#24958 = CARTESIAN_POINT ( 'NONE',  ( 15.62097837807030842, 31.00000000000000355, -17.81927981957692353 ) ) ;
#24959 = CIRCLE ( 'NONE', #33968, 20.00000000000000711 ) ;
#24960 = EDGE_CURVE ( 'NONE', #22923, #15394, #16470, .T. ) ;
#24961 = CIRCLE ( 'NONE', #20061, 120.5010000000000332 ) ;
#24962 = ORIENTED_EDGE ( 'NONE', *, *, #43104, .F. ) ;
#24963 = CARTESIAN_POINT ( 'NONE',  ( -2.454369252093152376, 40.00000000000000000, 37.60416666486730009 ) ) ;
#24964 = VERTEX_POINT ( 'NONE', #33407 ) ;
#24965 = CIRCLE ( 'NONE', #30694, 59.00000000000000711 ) ;
#24966 = DIRECTION ( 'NONE',  ( -1.000000000000000000, 0.000000000000000000, 0.000000000000000000 ) ) ;
#24967 = CARTESIAN_POINT ( 'NONE',  ( -2.725741868435985094, 3.045094352034055429, -3.220599429844047012 ) ) ;
#24968 = AXIS2_PLACEMENT_3D ( 'NONE', #42639, #23488, #42856 ) ;
#24969 = VECTOR ( 'NONE', #5109, 1000.000000000000000 ) ;
#24970 = ORIENTED_EDGE ( 'NONE', *, *, #31719, .T. ) ;
#24971 = DIRECTION ( 'NONE',  ( 1.000000000000000000, 0.000000000000000000, 0.000000000000000000 ) ) ;
#24972 = DIRECTION ( 'NONE',  ( -1.000000000000000000, 0.000000000000000000, 0.000000000000000000 ) ) ;
#24973 = ORIENTED_EDGE ( 'NONE', *, *, #1595, .T. ) ;
#24974 = CARTESIAN_POINT ( 'NONE',  ( 0.000000000000000000, 115.0622509503832589, 14.72000021165183803 ) ) ;
#24975 = ORIENTED_EDGE ( 'NONE', *, *, #28898, .T. ) ;
#24976 = ADVANCED_FACE ( 'NONE', ( #7205 ), #37317, .T. ) ;
#24977 = ORIENTED_EDGE ( 'NONE', *, *, #12137, .F. ) ;
#24978 = DIRECTION ( 'NONE',  ( -1.000000000000000000, 0.000000000000000000, 0.000000000000000000 ) ) ;
#24979 = CIRCLE ( 'NONE', #41641, 13.60000000000000142 ) ;
#24980 = CARTESIAN_POINT ( 'NONE',  ( -69.31868535681203980, 31.00000000000000711, 18.45717643660088214 ) ) ;
#24981 = EDGE_CURVE ( 'NONE', #3009, #3818, #204, .T. ) ;
#24982 = ORIENTED_EDGE ( 'NONE', *, *, #17492, .F. ) ;
#24983 = DIRECTION ( 'NONE',  ( 0.000000000000000000, 0.000000000000000000, 1.000000000000000000 ) ) ;
#24984 = CYLINDRICAL_SURFACE ( 'NONE', #17124, 59.00000000000000000 ) ;
#24985 = ORIENTED_EDGE ( 'NONE', *, *, #25866, .F. ) ;
#24986 = DIRECTION ( 'NONE',  ( 0.000000000000000000, 0.7865515558026395793, 0.6175246149461957046 ) ) ;
#24987 = PRODUCT_DEFINITION_SHAPE ( 'NONE', 'NONE',  #43208 ) ;
#24988 = EDGE_LOOP ( 'NONE', ( #10154, #43137, #412, #37886 ) ) ;
#24989 = CARTESIAN_POINT ( 'NONE',  ( -86.84058463553202500, 40.00000000000000711, 29.36381822872188607 ) ) ;
#24990 = CARTESIAN_POINT ( 'NONE',  ( -66.59699903142620769, 40.00000000000000711, 75.74378954611491110 ) ) ;
#24991 = CIRCLE ( 'NONE', #36069, 47.49900000000000233 ) ;
#24993 = DIRECTION ( 'NONE',  ( 1.000000000000000000, -0.000000000000000000, 0.000000000000000000 ) ) ;
#24992 = DIRECTION ( 'NONE',  ( 1.000000000000000000, 0.000000000000000000, 0.000000000000000000 ) ) ;
#24994 = CARTESIAN_POINT ( 'NONE',  ( 17.99999999999999645, -30.74337109795225942, 8.695908345466005329 ) ) ;
#24995 = CYLINDRICAL_SURFACE ( 'NONE', #4768, 36.00000000000000000 ) ;
#24996 = VECTOR ( 'NONE', #3890, 1000.000000000000000 ) ;
#24997 = ORIENTED_EDGE ( 'NONE', *, *, #1593, .F. ) ;
#24998 = AXIS2_PLACEMENT_3D ( 'NONE', #190, #30985, #1073 ) ;
#24999 = DIRECTION ( 'NONE',  ( 0.000000000000000000, 0.000000000000000000, -1.000000000000000000 ) ) ;
#25000 = ORIENTED_EDGE ( 'NONE', *, *, #23425, .F. ) ;
#25001 = CARTESIAN_POINT ( 'NONE',  ( 0.000000000000000000, 0.000000000000000000, 0.000000000000000000 ) ) ;
#25002 = CARTESIAN_POINT ( 'NONE',  ( -74.47060461443528823, 31.00000000000000711, 65.33029858165178894 ) ) ;
#25003 = EDGE_CURVE ( 'NONE', #16220, #35443, #24880, .T. ) ;
#25004 = DIRECTION ( 'NONE',  ( 0.000000000000000000, 0.000000000000000000, 1.000000000000000000 ) ) ;
#25006 = VERTEX_POINT ( 'NONE', #20351 ) ;
#25005 = VECTOR ( 'NONE', #40123, 1000.000000000000000 ) ;
#25007 = EDGE_CURVE ( 'NONE', #41335, #42394, #11609, .T. ) ;
#25008 = CARTESIAN_POINT ( 'NONE',  ( -1.974796425974089331, 40.00000000000000000, 29.60085432090885149 ) ) ;
#25009 = ORIENTED_EDGE ( 'NONE', *, *, #16561, .F. ) ;
#25010 = ORIENTED_EDGE ( 'NONE', *, *, #18406, .T. ) ;
#25011 = LINE ( 'NONE', #18686, #35280 ) ;
#25012 = DIRECTION ( 'NONE',  ( 0.000000000000000000, 0.000000000000000000, 1.000000000000000000 ) ) ;
#25013 = DIRECTION ( 'NONE',  ( -1.000000000000000000, 0.000000000000000000, 0.000000000000000000 ) ) ;
#25014 = AXIS2_PLACEMENT_3D ( 'NONE', #15418, #1202, #24594 ) ;
#25015 = FACE_BOUND ( 'NONE', #2847, .T. ) ;
#25016 = ADVANCED_FACE ( 'NONE', ( #20146 ), #7646, .T. ) ;
#25017 = EDGE_CURVE ( 'NONE', #25282, #35178, #6006, .T. ) ;
#25018 = ORIENTED_EDGE ( 'NONE', *, *, #10243, .T. ) ;
#25019 = CARTESIAN_POINT ( 'NONE',  ( 0.000000000000000000, -46.87740477351715640, -3.172455868805708956 ) ) ;
#25020 = EDGE_LOOP ( 'NONE', ( #40208, #3964, #25219, #791 ) ) ;
#25021 = CARTESIAN_POINT ( 'NONE',  ( 0.000000000000000000, -28.57802095670097131, 14.28532136906662586 ) ) ;
#25022 = DIRECTION ( 'NONE',  ( 0.000000000000000000, 0.000000000000000000, 1.000000000000000000 ) ) ;
#25023 = AXIS2_PLACEMENT_3D ( 'NONE', #24257, #17936, #28153 ) ;
#25024 = DIRECTION ( 'NONE',  ( -1.000000000000000000, -0.000000000000000000, -0.000000000000000000 ) ) ;
#25025 = DIRECTION ( 'NONE',  ( 0.000000000000000000, -0.8477344278896755680, 0.5304209081197351905 ) ) ;
#25026 = ORIENTED_EDGE ( 'NONE', *, *, #1706, .T. ) ;
#25027 = ORIENTED_EDGE ( 'NONE', *, *, #38337, .T. ) ;
#25028 = CARTESIAN_POINT ( 'NONE',  ( 9.000000000000001776, -31.08872492059985859, 41.68322423723089543 ) ) ;
#25029 = AXIS2_PLACEMENT_3D ( 'NONE', #42051, #2332, #39000 ) ;
#25030 = CARTESIAN_POINT ( 'NONE',  ( 17.99999999999999645, -83.49789599728724454, -86.88263557826851979 ) ) ;
#25031 = ADVANCED_FACE ( 'NONE', ( #33614 ), #27754, .F. ) ;
#25032 = VECTOR ( 'NONE', #12715, 1000.000000000000000 ) ;
#25033 = ORIENTED_EDGE ( 'NONE', *, *, #15432, .T. ) ;
#25035 = VERTEX_POINT ( 'NONE', #25349 ) ;
#25034 = DIRECTION ( 'NONE',  ( 0.000000000000000000, 0.000000000000000000, 1.000000000000000000 ) ) ;
#25036 = CARTESIAN_POINT ( 'NONE',  ( 36.58905133582347702, 31.00000000000000355, -27.97030060560319953 ) ) ;
#25037 = EDGE_CURVE ( 'NONE', #28849, #29751, #18589, .T. ) ;
#25038 = ORIENTED_EDGE ( 'NONE', *, *, #36356, .T. ) ;
#25039 = CARTESIAN_POINT ( 'NONE',  ( -91.96080130434573618, -34.05525454449571043, 14.45886780445633946 ) ) ;
#25041 = CYLINDRICAL_SURFACE ( 'NONE', #35171, 13.60000000000000142 ) ;
#25040 = CARTESIAN_POINT ( 'NONE',  ( -17.44537629401976275, 17.11489954122026447, 4.261559264950522063 ) ) ;
#25042 = ORIENTED_EDGE ( 'NONE', *, *, #1862, .F. ) ;
#25043 = DIRECTION ( 'NONE',  ( 0.000000000000000000, 0.7705132427757861446, 0.6374239897486934092 ) ) ;
#25044 = CARTESIAN_POINT ( 'NONE',  ( 41.67488199336423804, 40.00000000000000000, 54.49293397273886086 ) ) ;
#25045 = DIRECTION ( 'NONE',  ( 0.000000000000000000, 0.000000000000000000, 1.000000000000000000 ) ) ;
#25046 = LINE ( 'NONE', #43056, #15036 ) ;
#25047 = ORIENTED_EDGE ( 'NONE', *, *, #28812, .T. ) ;
#25048 = DIRECTION ( 'NONE',  ( -1.058513553088275437E-16, -1.000000000000000000, 8.813324511995299047E-17 ) ) ;
#25049 = VERTEX_POINT ( 'NONE', #18384 ) ;
#25050 = SHAPE_REPRESENTATION_RELATIONSHIP ( 'NONE' , 'NONE' ,  #19391, #21924 ) ;
#25051 = CARTESIAN_POINT ( 'NONE',  ( 17.99999999999999645, -41.62036691425453228, -113.0850832732718914 ) ) ;
#25052 = CARTESIAN_POINT ( 'NONE',  ( 106.4195705685734623, 106.4195705685780524, 10.00000000000025402 ) ) ;
#25053 = EDGE_CURVE ( 'NONE', #5216, #36925, #17957, .T. ) ;
#25054 = CARTESIAN_POINT ( 'NONE',  ( -17.60292107714122878, 31.00000000000000355, 65.74579412301164894 ) ) ;
#25056 = EDGE_CURVE ( 'NONE', #41792, #37428, #42898, .T. ) ;
#25055 = VECTOR ( 'NONE', #10036, 1000.000000000000000 ) ;
#25057 = CARTESIAN_POINT ( 'NONE',  ( 17.99999999999999645, -86.84764344322910290, -76.89919913989835720 ) ) ;
#25058 = AXIS2_PLACEMENT_3D ( 'NONE', #43143, #39212, #42698 ) ;
#25059 = VERTEX_POINT ( 'NONE', #18175 ) ;
#25060 = EDGE_CURVE ( 'NONE', #28014, #5537, #5298, .T. ) ;
#25061 = EDGE_CURVE ( 'NONE', #27792, #41792, #35249, .T. ) ;
#25062 = VECTOR ( 'NONE', #33641, 1000.000000000000000 ) ;
#25063 = FACE_OUTER_BOUND ( 'NONE', #40953, .T. ) ;
#25064 = ORIENTED_EDGE ( 'NONE', *, *, #12384, .T. ) ;
#25065 = DIRECTION ( 'NONE',  ( -1.000000000000000000, -0.000000000000000000, 0.000000000000000000 ) ) ;
#25066 = DIRECTION ( 'NONE',  ( 0.000000000000000000, 0.000000000000000000, 1.000000000000000000 ) ) ;
#25067 = CARTESIAN_POINT ( 'NONE',  ( -79.74759331938361129, 31.00000000000000711, -21.47736420602193519 ) ) ;
#25068 = CARTESIAN_POINT ( 'NONE',  ( -37.02054590706428172, 40.00000000000000000, -75.34311506435015815 ) ) ;
#25069 = CARTESIAN_POINT ( 'NONE',  ( 0.000000000000000000, -61.59243992711397198, -93.77976230226100540 ) ) ;
#25070 = VERTEX_POINT ( 'NONE', #15522 ) ;
#25071 = CARTESIAN_POINT ( 'NONE',  ( 3.679171394226031122, 2.494631558665830973, -0.3503314178412474389 ) ) ;
#25072 = ORIENTED_EDGE ( 'NONE', *, *, #40596, .T. ) ;
#25073 = CYLINDRICAL_SURFACE ( 'NONE', #13043, 31.49899999999999878 ) ;
#25074 = DIRECTION ( 'NONE',  ( 0.000000000000000000, 0.000000000000000000, 1.000000000000000000 ) ) ;
#25076 = EDGE_LOOP ( 'NONE', ( #10069, #14459 ) ) ;
#25075 = CARTESIAN_POINT ( 'NONE',  ( 42.80287614962790599, -14.05525454449571932, 69.29271901957253021 ) ) ;
#25077 = DIRECTION ( 'NONE',  ( -1.000000000000000000, 0.000000000000000000, -0.000000000000000000 ) ) ;
#25078 = VERTEX_POINT ( 'NONE', #31230 ) ;
#25079 = DIRECTION ( 'NONE',  ( 0.000000000000000000, 0.000000000000000000, 1.000000000000000000 ) ) ;
#25080 = CARTESIAN_POINT ( 'NONE',  ( 17.99999999999999645, -21.55123232222554464, 118.5581519187671660 ) ) ;
#25081 = ORIENTED_EDGE ( 'NONE', *, *, #39376, .T. ) ;
#25082 = FACE_OUTER_BOUND ( 'NONE', #8737, .T. ) ;
#25083 = AXIS2_PLACEMENT_3D ( 'NONE', #20022, #40016, #33291 ) ;
#25084 = CARTESIAN_POINT ( 'NONE',  ( 0.000000000000000000, 111.1352304691229733, -15.40237066878481720 ) ) ;
#25085 = EDGE_CURVE ( 'NONE', #21881, #30236, #31093, .T. ) ;
#25086 = AXIS2_PLACEMENT_3D ( 'NONE', #31259, #20829, #14904 ) ;
#25088 = DIRECTION ( 'NONE',  ( 1.000000000000000000, 0.000000000000000000, 0.000000000000000000 ) ) ;
#25087 = CARTESIAN_POINT ( 'NONE',  ( 17.99999999999999645, -57.69704296431110890, -105.7900857083235451 ) ) ;
#25089 = ORIENTED_EDGE ( 'NONE', *, *, #24737, .F. ) ;
#25090 = CARTESIAN_POINT ( 'NONE',  ( 17.99999999999999645, -16.86122981692000167, -27.13802899033310112 ) ) ;
#25091 = VERTEX_POINT ( 'NONE', #11591 ) ;
#25092 = DIRECTION ( 'NONE',  ( 0.000000000000000000, -0.5528000653612000770, 0.8333139190825106235 ) ) ;
#25093 = CARTESIAN_POINT ( 'NONE',  ( 17.75583184595346964, 40.00000000000000000, -30.63479189996225216 ) ) ;
#25094 = DIRECTION ( 'NONE',  ( -1.000000000000000000, -0.000000000000000000, -0.000000000000000000 ) ) ;
#25095 = CARTESIAN_POINT ( 'NONE',  ( 2.500000000000000888, 3.061616997868384127E-16, -4.974599999999998801 ) ) ;
#25096 = CARTESIAN_POINT ( 'NONE',  ( 0.000000000000000000, -29.68570942776464960, -10.53307442156965656 ) ) ;
#25097 = ORIENTED_EDGE ( 'NONE', *, *, #17909, .T. ) ;
#25098 = FACE_OUTER_BOUND ( 'NONE', #1255, .T. ) ;
#25099 = ORIENTED_EDGE ( 'NONE', *, *, #23206, .T. ) ;
#25100 = CARTESIAN_POINT ( 'NONE',  ( 0.2500000000000002220, 5.204748896376250699E-16, -4.250000000000000000 ) ) ;
#25101 = DIRECTION ( 'NONE',  ( 0.000000000000000000, 0.000000000000000000, -1.000000000000000000 ) ) ;
#25102 = CARTESIAN_POINT ( 'NONE',  ( 5.583751958424166162, 31.00000000000000355, -42.43436172917101601 ) ) ;
#25103 = VERTEX_POINT ( 'NONE', #24936 ) ;
#25104 = DIRECTION ( 'NONE',  ( -1.000000000000000000, -0.000000000000000000, -0.000000000000000000 ) ) ;
#25105 = ADVANCED_FACE ( 'NONE', ( #8725 ), #31873, .F. ) ;
#25106 = ADVANCED_FACE ( 'NONE', ( #12034 ), #22080, .T. ) ;
#25107 = EDGE_CURVE ( 'NONE', #39162, #41904, #15097, .T. ) ;
#25108 = DIRECTION ( 'NONE',  ( 1.000000000000000000, -0.000000000000000000, 0.000000000000000000 ) ) ;
#25109 = CARTESIAN_POINT ( 'NONE',  ( 74.72486387243833406, 31.00000000000000000, 9.837939412698395003 ) ) ;
#25110 = AXIS2_PLACEMENT_3D ( 'NONE', #1901, #35693, #15889 ) ;
#25111 = AXIS2_PLACEMENT_3D ( 'NONE', #18908, #22595, #42812 ) ;
#25112 = ORIENTED_EDGE ( 'NONE', *, *, #26286, .F. ) ;
#25113 = CARTESIAN_POINT ( 'NONE',  ( 33.95200755730775199, 31.00000000000000355, -44.10258293179329314 ) ) ;
#25114 = CARTESIAN_POINT ( 'NONE',  ( 84.66040299356156140, 39.99999999999999289, 11.14692016787551765 ) ) ;
#25115 = AXIS2_PLACEMENT_3D ( 'NONE', #30565, #20987, #21200 ) ;
#25116 = ORIENTED_EDGE ( 'NONE', *, *, #11109, .T. ) ;
#25117 = DIRECTION ( 'NONE',  ( -1.000000000000000000, -0.000000000000000000, 0.000000000000000000 ) ) ;
#25118 = ADVANCED_FACE ( 'NONE', ( #41225 ), #5026, .T. ) ;
#25119 = DIRECTION ( 'NONE',  ( -1.000000000000000000, -0.000000000000000000, -0.000000000000000000 ) ) ;
#25120 = DIRECTION ( 'NONE',  ( 1.000000000000000000, 0.000000000000000000, 0.000000000000000000 ) ) ;
#25122 = VERTEX_POINT ( 'NONE', #5237 ) ;
#25121 = CARTESIAN_POINT ( 'NONE',  ( 9.000000000000001776, 51.85248208264523129, -3.914090171285650843 ) ) ;
#25123 = CARTESIAN_POINT ( 'NONE',  ( 0.000000000000000000, -111.2559044912527355, 32.83479428644638887 ) ) ;
#25124 = DIRECTION ( 'NONE',  ( -1.000000000000000000, 0.000000000000000000, 0.000000000000000000 ) ) ;
#25125 = ORIENTED_EDGE ( 'NONE', *, *, #34593, .T. ) ;
#25126 = CARTESIAN_POINT ( 'NONE',  ( 40.54457361686378647, 40.00000000000000000, 52.83773991529862712 ) ) ;
#25127 = DIRECTION ( 'NONE',  ( -1.000000000000000000, -0.000000000000000000, 0.000000000000000000 ) ) ;
#25128 = ORIENTED_EDGE ( 'NONE', *, *, #5504, .T. ) ;
#25129 = DIRECTION ( 'NONE',  ( 0.000000000000000000, 0.000000000000000000, 1.000000000000000000 ) ) ;
#25130 = CARTESIAN_POINT ( 'NONE',  ( 17.99999999999999645, 101.1403355683153933, -56.80345518653383152 ) ) ;
#25131 = CARTESIAN_POINT ( 'NONE',  ( -101.9145453900124068, 17.11489954122026447, -1.407535261550463268 ) ) ;
#25132 = VERTEX_POINT ( 'NONE', #28405 ) ;
#25133 = EDGE_LOOP ( 'NONE', ( #33611, #24629, #13434, #806 ) ) ;
#25134 = CARTESIAN_POINT ( 'NONE',  ( 17.99999999999999645, 110.3490479609629489, 20.28201389785587949 ) ) ;
#25136 = ORIENTED_EDGE ( 'NONE', *, *, #5876, .T. ) ;
#25135 = CIRCLE ( 'NONE', #5561, 13.59999999999999964 ) ;
#25137 = CARTESIAN_POINT ( 'NONE',  ( 2.500000000000000000, -1.178949249685214307, 2.042000000000001592 ) ) ;
#25138 = DIRECTION ( 'NONE',  ( -1.000000000000000000, 0.000000000000000000, 0.000000000000000000 ) ) ;
#25139 = CYLINDRICAL_SURFACE ( 'NONE', #24730, 59.00000000000000000 ) ;
#25140 = CYLINDRICAL_SURFACE ( 'NONE', #24864, 59.00000000000000000 ) ;
#25141 = VERTEX_POINT ( 'NONE', #14874 ) ;
#25142 = FACE_OUTER_BOUND ( 'NONE', #13619, .T. ) ;
#25143 = CYLINDRICAL_SURFACE ( 'NONE', #826, 59.00000000000000000 ) ;
#25144 = ORIENTED_EDGE ( 'NONE', *, *, #43102, .T. ) ;
#25145 = LINE ( 'NONE', #14663, #29464 ) ;
#25146 = EDGE_CURVE ( 'NONE', #38699, #15576, #34474, .T. ) ;
#25147 = CARTESIAN_POINT ( 'NONE',  ( 17.99999999999999645, 106.6051926090971023, 45.73109345704855855 ) ) ;
#25148 = DIRECTION ( 'NONE',  ( -1.000000000000000000, -6.123233995736766036E-17, 7.044195017643634285E-15 ) ) ;
#25149 = CARTESIAN_POINT ( 'NONE',  ( 17.99999999999999645, 95.38615066514064722, -59.07414607872728141 ) ) ;
#25150 = CARTESIAN_POINT ( 'NONE',  ( -29.60425243605831724, 31.00000000000000355, 38.59963703562669934 ) ) ;
#25151 = VERTEX_POINT ( 'NONE', #28819 ) ;
#25153 = DIRECTION ( 'NONE',  ( 0.000000000000000000, 0.9826841245925203028, 0.1852887240871181618 ) ) ;
#25152 = FACE_OUTER_BOUND ( 'NONE', #4043, .T. ) ;
#25154 = AXIS2_PLACEMENT_3D ( 'NONE', #41447, #8085, #31233 ) ;
#25155 = VERTEX_POINT ( 'NONE', #18605 ) ;
#25156 = EDGE_CURVE ( 'NONE', #31728, #3775, #11331, .T. ) ;
#25157 = CARTESIAN_POINT ( 'NONE',  ( 28.40420691229738281, 40.00000000000000000, 49.17333623205379922 ) ) ;
#25158 = ADVANCED_FACE ( 'NONE', ( #11819 ), #25143, .F. ) ;
#25159 = CIRCLE ( 'NONE', #25825, 59.00000000000000000 ) ;
#25160 = VECTOR ( 'NONE', #11470, 1000.000000000000000 ) ;
#25161 = CARTESIAN_POINT ( 'NONE',  ( 9.000000000000001776, 23.85344185397347161, -113.5209818126988779 ) ) ;
#25162 = ADVANCED_FACE ( 'NONE', ( #34701 ), #8513, .T. ) ;
#25163 = CARTESIAN_POINT ( 'NONE',  ( 17.99999999999999645, 119.7318547011701497, 13.59315897125768124 ) ) ;
#25164 = AXIS2_PLACEMENT_3D ( 'NONE', #6726, #9996, #30096 ) ;
#25165 = VECTOR ( 'NONE', #26630, 1000.000000000000000 ) ;
#25166 = CARTESIAN_POINT ( 'NONE',  ( 17.99999999999999645, 31.80866420683990725, 2.997093558041416195 ) ) ;
#25167 = CARTESIAN_POINT ( 'NONE',  ( -2.924622967158192921, 31.00000000000000355, -22.14664255385889291 ) ) ;
#25168 = ORIENTED_EDGE ( 'NONE', *, *, #12659, .T. ) ;
#25169 = CARTESIAN_POINT ( 'NONE',  ( -14.08558183832706234, 40.00000000000000000, -28.55406316770863739 ) ) ;
#25170 = ORIENTED_EDGE ( 'NONE', *, *, #27134, .T. ) ;
#25171 = DIRECTION ( 'NONE',  ( -1.000000000000000000, 0.000000000000000000, -0.000000000000000000 ) ) ;
#25172 = CARTESIAN_POINT ( 'NONE',  ( -0.6640947660597427138, 4.471078309994878985, -3.602146406945963442 ) ) ;
#25173 = ORIENTED_EDGE ( 'NONE', *, *, #17913, .F. ) ;
#25174 = DIRECTION ( 'NONE',  ( 0.000000000000000000, 0.000000000000000000, 1.000000000000000000 ) ) ;
#25175 = DIRECTION ( 'NONE',  ( -1.000000000000000000, -0.000000000000000000, -0.000000000000000000 ) ) ;
#25176 = ORIENTED_EDGE ( 'NONE', *, *, #280, .T. ) ;
#25177 = CARTESIAN_POINT ( 'NONE',  ( 0.000000000000000000, 0.000000000000000000, -25.00000000000000000 ) ) ;
#25178 = ORIENTED_EDGE ( 'NONE', *, *, #13297, .T. ) ;
#25179 = EDGE_CURVE ( 'NONE', #2427, #2530, #19869, .T. ) ;
#25180 = EDGE_CURVE ( 'NONE', #16988, #12470, #42620, .T. ) ;
#25181 = EDGE_LOOP ( 'NONE', ( #43096, #1984, #41050, #16139 ) ) ;
#25182 = CARTESIAN_POINT ( 'NONE',  ( 22.90854556226710415, -40.05525454449572464, -74.83297477053821467 ) ) ;
#25184 = AXIS2_PLACEMENT_3D ( 'NONE', #23152, #13321, #16611 ) ;
#25183 = CARTESIAN_POINT ( 'NONE',  ( -81.27520743792995006, 31.00000000000000711, 10.59408403752164851 ) ) ;
#25185 = ORIENTED_EDGE ( 'NONE', *, *, #20974, .T. ) ;
#25186 = CARTESIAN_POINT ( 'NONE',  ( 0.000000000000000000, -54.09091620264652533, -102.6166301549523467 ) ) ;
#25187 = DIRECTION ( 'NONE',  ( 0.000000000000000000, -0.9618256431728219313, 0.2736629900720728981 ) ) ;
#25188 = VERTEX_POINT ( 'NONE', #29455 ) ;
#25189 = CYLINDRICAL_SURFACE ( 'NONE', #27304, 51.99999999999999289 ) ;
#25190 = CARTESIAN_POINT ( 'NONE',  ( -26.02152878260477564, 40.00000000000000000, 96.68563202207252516 ) ) ;
#25191 = VECTOR ( 'NONE', #19797, 1000.000000000000000 ) ;
#25192 = AXIS2_PLACEMENT_3D ( 'NONE', #2678, #16040, #12338 ) ;
#25193 = CARTESIAN_POINT ( 'NONE',  ( -18.31940394017777507, 31.00000000000000355, -14.05611420671224288 ) ) ;
#25194 = VECTOR ( 'NONE', #24875, 1000.000000000000000 ) ;
#25196 = CARTESIAN_POINT ( 'NONE',  ( -129.9999999999994884, 1.161927740252948949E-12, 369.6955262170048400 ) ) ;
#25195 = CARTESIAN_POINT ( 'NONE',  ( -2.500000000000000888, 0.000000000000000000, -4.974599999999998801 ) ) ;
#25197 = AXIS2_PLACEMENT_3D ( 'NONE', #42491, #12636, #32899 ) ;
#25198 = DIRECTION ( 'NONE',  ( 0.000000000000000000, 0.000000000000000000, 1.000000000000000000 ) ) ;
#25199 = CARTESIAN_POINT ( 'NONE',  ( 53.80287614962789178, -40.05525454449572464, 69.29271901957253021 ) ) ;
#25200 = EDGE_CURVE ( 'NONE', #25141, #12154, #16924, .T. ) ;
#25201 = ORIENTED_EDGE ( 'NONE', *, *, #33457, .T. ) ;
#25202 =( LENGTH_UNIT ( ) NAMED_UNIT ( * ) SI_UNIT ( .MILLI., .METRE. ) );
#25203 = DIRECTION ( 'NONE',  ( 0.000000000000000000, 0.000000000000000000, -1.000000000000000000 ) ) ;
#25204 = CIRCLE ( 'NONE', #12652, 2.649999999999993694 ) ;
#25205 = VERTEX_POINT ( 'NONE', #2365 ) ;
#25206 = DIRECTION ( 'NONE',  ( 0.000000000000000000, -0.1837495178165777232, 0.9829730996839003421 ) ) ;
#25207 = CARTESIAN_POINT ( 'NONE',  ( -65.18298466990795248, 31.00000000000000711, 74.32329070269128124 ) ) ;
#25208 = DIRECTION ( 'NONE',  ( 0.000000000000000000, 0.000000000000000000, 1.000000000000000000 ) ) ;
#25209 = ORIENTED_EDGE ( 'NONE', *, *, #22326, .T. ) ;
#25210 = CARTESIAN_POINT ( 'NONE',  ( -6.237032369604346371, 40.00000000000000000, -23.31551866006812901 ) ) ;
#25211 = EDGE_CURVE ( 'NONE', #9900, #30604, #25278, .T. ) ;
#25212 = VERTEX_POINT ( 'NONE', #16606 ) ;
#25213 = EDGE_LOOP ( 'NONE', ( #42264, #19865, #29811, #4680 ) ) ;
#25214 = FACE_BOUND ( 'NONE', #14054, .T. ) ;
#25215 = CARTESIAN_POINT ( 'NONE',  ( -19.85879968743109458, -2.055254544495720648, 67.01652747270929922 ) ) ;
#25216 = DIRECTION ( 'NONE',  ( 0.000000000000000000, 0.000000000000000000, 1.000000000000000000 ) ) ;
#25217 = CARTESIAN_POINT ( 'NONE',  ( 0.000000000000000000, 18.42432724429473012, 30.92804820216009176 ) ) ;
#25218 = LINE ( 'NONE', #26042, #23003 ) ;
#25219 = ORIENTED_EDGE ( 'NONE', *, *, #41343, .T. ) ;
#25220 = CYLINDRICAL_SURFACE ( 'NONE', #36762, 1.000000000000000666 ) ;
#25221 = ORIENTED_EDGE ( 'NONE', *, *, #40574, .F. ) ;
#25222 = DIRECTION ( 'NONE',  ( 1.000000000000000000, 0.000000000000000000, 0.000000000000000000 ) ) ;
#25223 = AXIS2_PLACEMENT_3D ( 'NONE', #41323, #8603, #8829 ) ;
#25224 = CARTESIAN_POINT ( 'NONE',  ( 0.000000000000000000, 0.000000000000000000, 0.000000000000000000 ) ) ;
#25225 = AXIS2_PLACEMENT_3D ( 'NONE', #39068, #35782, #6136 ) ;
#25226 = DIRECTION ( 'NONE',  ( -1.000000000000000000, 0.000000000000000000, -0.000000000000000000 ) ) ;
#25227 = VECTOR ( 'NONE', #28102, 1000.000000000000000 ) ;
#25228 = FACE_OUTER_BOUND ( 'NONE', #285, .T. ) ;
#25229 = VERTEX_POINT ( 'NONE', #35547 ) ;
#25230 = ORIENTED_EDGE ( 'NONE', *, *, #38694, .F. ) ;
#25231 = CYLINDRICAL_SURFACE ( 'NONE', #15877, 120.5010000000000190 ) ;
#25232 = EDGE_CURVE ( 'NONE', #13405, #42589, #15520, .T. ) ;
#25233 = VECTOR ( 'NONE', #30947, 1000.000000000000000 ) ;
#25234 = ORIENTED_EDGE ( 'NONE', *, *, #3555, .F. ) ;
#25236 = ORIENTED_EDGE ( 'NONE', *, *, #38015, .F. ) ;
#25235 = FACE_OUTER_BOUND ( 'NONE', #15321, .T. ) ;
#25237 = CARTESIAN_POINT ( 'NONE',  ( -6.590854309045712789, 31.00000000000000355, 49.37518673228670707 ) ) ;
#25239 = ADVANCED_FACE ( 'NONE', ( #22946 ), #42084, .F. ) ;
#25238 = VERTEX_POINT ( 'NONE', #19023 ) ;
#25240 = DIRECTION ( 'NONE',  ( -1.000000000000000000, -0.000000000000000000, 0.000000000000000000 ) ) ;
#25242 = FILL_AREA_STYLE_COLOUR ( '', #40734 ) ;
#25241 = DIRECTION ( 'NONE',  ( -1.000000000000000000, 0.000000000000000000, -0.000000000000000000 ) ) ;
#25243 = ORIENTED_EDGE ( 'NONE', *, *, #12106, .F. ) ;
#25244 = CARTESIAN_POINT ( 'NONE',  ( -70.06919973880852126, 40.00000000000000711, -18.87919424805731339 ) ) ;
#25245 = CARTESIAN_POINT ( 'NONE',  ( 17.99999999999999645, 75.03166794516924654, -94.29071961951432002 ) ) ;
#25246 = DIRECTION ( 'NONE',  ( 0.000000000000000000, 0.000000000000000000, -1.000000000000000000 ) ) ;
#25247 = ORIENTED_EDGE ( 'NONE', *, *, #6928, .T. ) ;
#25248 = DIRECTION ( 'NONE',  ( 1.000000000000000000, -0.000000000000000000, -0.000000000000000000 ) ) ;
#25249 = ORIENTED_EDGE ( 'NONE', *, *, #17703, .F. ) ;
#25250 = FACE_OUTER_BOUND ( 'NONE', #29980, .T. ) ;
#25251 = DIRECTION ( 'NONE',  ( 0.000000000000000000, -0.9714298932647074114, -0.2373266998711250908 ) ) ;
#25252 = CIRCLE ( 'NONE', #35654, 116.0000000000000000 ) ;
#25253 = CARTESIAN_POINT ( 'NONE',  ( -60.02123122004734768, 31.00000000000000711, 34.66859033927303813 ) ) ;
#25254 = CARTESIAN_POINT ( 'NONE',  ( 0.000000000000000000, 0.000000000000000000, 0.000000000000000000 ) ) ;
#25255 = ORIENTED_EDGE ( 'NONE', *, *, #35351, .F. ) ;
#25256 = CYLINDRICAL_SURFACE ( 'NONE', #24776, 116.0000000000000000 ) ;
#25257 = EDGE_CURVE ( 'NONE', #5449, #38358, #34980, .T. ) ;
#25258 = AXIS2_PLACEMENT_3D ( 'NONE', #22342, #39504, #42131 ) ;
#25259 = VERTEX_POINT ( 'NONE', #5872 ) ;
#25260 = DIRECTION ( 'NONE',  ( 1.000000000000000000, -0.000000000000000000, -0.000000000000000000 ) ) ;
#25261 = ADVANCED_FACE ( 'NONE', ( #39670 ), #9796, .F. ) ;
#25262 = DIRECTION ( 'NONE',  ( 0.000000000000000000, 0.000000000000000000, 1.000000000000000000 ) ) ;
#25263 = CARTESIAN_POINT ( 'NONE',  ( 74.83201185292551827, 31.00000000000000000, -43.08100868842220166 ) ) ;
#25264 = CARTESIAN_POINT ( 'NONE',  ( 28.55926749299792178, 40.00000000000000000, 84.46800049165049984 ) ) ;
#25265 = CARTESIAN_POINT ( 'NONE',  ( 17.99999999999999645, 28.57802095670086828, 14.28532136906683370 ) ) ;
#25266 = ADVANCED_FACE ( 'NONE', ( #42515 ), #12237, .T. ) ;
#25267 = ORIENTED_EDGE ( 'NONE', *, *, #3351, .F. ) ;
#25268 = CARTESIAN_POINT ( 'NONE',  ( -10.00000000000000000, 0.000000000000000000, 0.000000000000000000 ) ) ;
#25269 = ORIENTED_EDGE ( 'NONE', *, *, #19564, .T. ) ;
#25270 = DIRECTION ( 'NONE',  ( -1.000000000000000000, -0.000000000000000000, -0.000000000000000000 ) ) ;
#25271 = CARTESIAN_POINT ( 'NONE',  ( 17.99999999999999645, 29.03409033315581667, 12.21509719675401051 ) ) ;
#25273 = ORIENTED_EDGE ( 'NONE', *, *, #27266, .T. ) ;
#25272 = LINE ( 'NONE', #1661, #13750 ) ;
#25274 = LINE ( 'NONE', #8644, #17800 ) ;
#25275 = ORIENTED_EDGE ( 'NONE', *, *, #17549, .F. ) ;
#25276 = DIRECTION ( 'NONE',  ( 0.000000000000000000, 0.000000000000000000, 1.000000000000000000 ) ) ;
#25277 = CARTESIAN_POINT ( 'NONE',  ( 9.000000000000001776, -30.03615769709762517, 42.44795908868979240 ) ) ;
#25278 = CIRCLE ( 'NONE', #41252, 59.00000000000000711 ) ;
#25279 = CYLINDRICAL_SURFACE ( 'NONE', #27131, 2.649999999999971934 ) ;
#25280 = AXIS2_PLACEMENT_3D ( 'NONE', #35120, #10946, #18174 ) ;
#25281 = AXIS2_PLACEMENT_3D ( 'NONE', #30043, #13465, #40027 ) ;
#25282 = VERTEX_POINT ( 'NONE', #36186 ) ;
#25283 = EDGE_CURVE ( 'NONE', #13787, #12118, #42718, .T. ) ;
#25284 = DIRECTION ( 'NONE',  ( 0.000000000000000000, 0.3612416661871471479, 0.9324722294043580328 ) ) ;
#25285 = ADVANCED_FACE ( 'NONE', ( #38821 ), #19230, .F. ) ;
#25286 = FACE_OUTER_BOUND ( 'NONE', #1908, .T. ) ;
#25287 = EDGE_CURVE ( 'NONE', #3675, #719, #36395, .T. ) ;
#25288 = EDGE_CURVE ( 'NONE', #27234, #9752, #37062, .T. ) ;
#25289 = AXIS2_PLACEMENT_3D ( 'NONE', #1940, #15305, #25129 ) ;
#25291 = CARTESIAN_POINT ( 'NONE',  ( 0.000000000000000000, 46.90537658765334328, -2.727856614653797251 ) ) ;
#25290 = DIRECTION ( 'NONE',  ( 1.000000000000000000, 0.000000000000000000, 0.000000000000000000 ) ) ;
#25292 = ORIENTED_EDGE ( 'NONE', *, *, #33609, .F. ) ;
#25293 = DIRECTION ( 'NONE',  ( -1.000000000000000000, -0.000000000000000000, -0.000000000000000000 ) ) ;
#25294 = VERTEX_POINT ( 'NONE', #9153 ) ;
#25295 = CARTESIAN_POINT ( 'NONE',  ( 2.500000000000000000, 0.000000000000000000, 0.000000000000000000 ) ) ;
#25296 = CARTESIAN_POINT ( 'NONE',  ( -26.44890248586417414, 40.00000000000000000, -34.59877114778964113 ) ) ;
#25297 = CARTESIAN_POINT ( 'NONE',  ( 0.000000000000000000, -111.2721026680461733, 14.38025178762581469 ) ) ;
#25298 = DIRECTION ( 'NONE',  ( -0.000000000000000000, -0.000000000000000000, 1.000000000000000000 ) ) ;
#25299 = LINE ( 'NONE', #25724, #2516 ) ;
#25300 = VERTEX_POINT ( 'NONE', #22506 ) ;
#25301 = CARTESIAN_POINT ( 'NONE',  ( 17.99999999999999645, 11.58753559615527529, -29.77419532459249751 ) ) ;
#25302 = ORIENTED_EDGE ( 'NONE', *, *, #28694, .T. ) ;
#25303 = DIRECTION ( 'NONE',  ( 0.000000000000000000, 0.000000000000000000, 1.000000000000000000 ) ) ;
#25304 = CYLINDRICAL_SURFACE ( 'NONE', #31022, 59.00000000000000000 ) ;
#25305 = CARTESIAN_POINT ( 'NONE',  ( 22.24487986055951083, 31.00000000000000355, 28.98451114863597766 ) ) ;
#25306 = VERTEX_POINT ( 'NONE', #15951 ) ;
#25307 =( NAMED_UNIT ( * ) SI_UNIT ( $, .STERADIAN. ) SOLID_ANGLE_UNIT ( ) );
#25308 = ITEM_DEFINED_TRANSFORMATION ( 'NONE', 'NONE', #27462,  #13552 ) ;
#25309 = DIRECTION ( 'NONE',  ( -1.000000000000000000, -0.000000000000000000, -0.000000000000000000 ) ) ;
#25310 = EDGE_CURVE ( 'NONE', #7190, #21257, #18311, .T. ) ;
#25311 = AXIS2_PLACEMENT_3D ( 'NONE', #15476, #28774, #25513 ) ;
#25312 = CARTESIAN_POINT ( 'NONE',  ( -68.69954721042445556, 31.00000000000000711, 39.68009708086182741 ) ) ;
#25313 = ORIENTED_EDGE ( 'NONE', *, *, #23158, .F. ) ;
#25314 = CARTESIAN_POINT ( 'NONE',  ( 54.79583221319987985, 31.00000000000000355, -14.58025558542526490 ) ) ;
#25315 = AXIS2_PLACEMENT_3D ( 'NONE', #31160, #28755, #32015 ) ;
#25316 = CARTESIAN_POINT ( 'NONE',  ( -68.67288961433401084, 40.00000000000000711, -60.22678404055071155 ) ) ;
#25317 = ORIENTED_EDGE ( 'NONE', *, *, #1184, .F. ) ;
#25318 = AXIS2_PLACEMENT_3D ( 'NONE', #8036, #18556, #4774 ) ;
#25319 = DIRECTION ( 'NONE',  ( 0.000000000000000000, 0.000000000000000000, 1.000000000000000000 ) ) ;
#25320 = CARTESIAN_POINT ( 'NONE',  ( 17.99999999999999645, -117.6086855750636460, 26.24286718912065552 ) ) ;
#25321 = CARTESIAN_POINT ( 'NONE',  ( 17.99999999999999645, 84.77518783075095143, 73.49448960231384831 ) ) ;
#25323 = EDGE_LOOP ( 'NONE', ( #20832, #23557 ) ) ;
#25322 = DIRECTION ( 'NONE',  ( -1.000000000000000000, -0.000000000000000000, -0.000000000000000000 ) ) ;
#25324 = DIRECTION ( 'NONE',  ( 0.000000000000000000, 0.000000000000000000, 1.000000000000000000 ) ) ;
#25325 = CARTESIAN_POINT ( 'NONE',  ( 0.6507732100473444525, -4.243078065514795050, -0.2236248678334952777 ) ) ;
#25326 = ORIENTED_EDGE ( 'NONE', *, *, #4376, .F. ) ;
#25327 = CARTESIAN_POINT ( 'NONE',  ( -60.02123122004734768, 40.00000000000000711, 34.66859033927303813 ) ) ;
#25328 = CARTESIAN_POINT ( 'NONE',  ( 17.99999999999999645, 18.35539002514530793, -110.6858262410707994 ) ) ;
#25329 = VERTEX_POINT ( 'NONE', #32710 ) ;
#25330 = ADVANCED_FACE ( 'NONE', ( #12874 ), #26182, .F. ) ;
#25331 = CARTESIAN_POINT ( 'NONE',  ( 18.00000000000000355, 6.109652351742432153, -46.58570277113501845 ) ) ;
#25332 = DIRECTION ( 'NONE',  ( -0.000000000000000000, -0.000000000000000000, 1.000000000000000000 ) ) ;
#25333 = EDGE_CURVE ( 'NONE', #35630, #5342, #27329, .T. ) ;
#25334 = EDGE_CURVE ( 'NONE', #27883, #31415, #21114, .T. ) ;
#25335 = DIRECTION ( 'NONE',  ( -1.000000000000000000, 0.000000000000000000, -0.000000000000000000 ) ) ;
#25336 = VERTEX_POINT ( 'NONE', #40527 ) ;
#25337 = EDGE_CURVE ( 'NONE', #2405, #16540, #33361, .T. ) ;
#25338 = AXIS2_PLACEMENT_3D ( 'NONE', #1860, #28298, #28076 ) ;
#25339 = ORIENTED_EDGE ( 'NONE', *, *, #29962, .F. ) ;
#25340 = DIRECTION ( 'NONE',  ( 1.000000000000000000, -0.000000000000000000, -0.000000000000000000 ) ) ;
#25341 = ORIENTED_EDGE ( 'NONE', *, *, #1347, .F. ) ;
#25342 = DIRECTION ( 'NONE',  ( 1.000000000000000000, -0.000000000000000000, 0.000000000000000000 ) ) ;
#25343 = LINE ( 'NONE', #25765, #23486 ) ;
#25344 = DIRECTION ( 'NONE',  ( -1.000000000000000000, 0.000000000000000000, 0.000000000000000000 ) ) ;
#25345 = CARTESIAN_POINT ( 'NONE',  ( 17.99999999999999645, -3.803237743092135581, 31.26855263151013276 ) ) ;
#25346 = ORIENTED_EDGE ( 'NONE', *, *, #2370, .F. ) ;
#25347 = CYLINDRICAL_SURFACE ( 'NONE', #4979, 11.00000000000000000 ) ;
#25348 = VECTOR ( 'NONE', #2952, 1000.000000000000000 ) ;
#25349 = CARTESIAN_POINT ( 'NONE',  ( 0.000000000000000000, -47.22458491092822896, 5.098390039074067737 ) ) ;
#25350 = ADVANCED_FACE ( 'NONE', ( #10452 ), #6948, .T. ) ;
#25351 = ORIENTED_EDGE ( 'NONE', *, *, #6718, .T. ) ;
#25352 = CARTESIAN_POINT ( 'NONE',  ( 18.00000000000000355, -22.43957647427189528, 41.27978878573620847 ) ) ;
#25353 = CYLINDRICAL_SURFACE ( 'NONE', #19557, 120.5010000000000190 ) ;
#25354 = B_SPLINE_CURVE_WITH_KNOTS ( 'NONE', 3,
 ( #22659, #9741, #23092, #35906, #19593, #42246, #32440, #25723 ),
 .UNSPECIFIED., .F., .F.,
 ( 4, 2, 2, 4 ),
 ( 0.000000000000000000, 0.002450665683189820997, 0.003675998524784731495, 0.004901331366379641993 ),
 .UNSPECIFIED. ) ;
#25355 = SHAPE_DEFINITION_REPRESENTATION ( #23169, #37437 ) ;
#25356 = LINE ( 'NONE', #21668, #4404 ) ;
#25357 = CARTESIAN_POINT ( 'NONE',  ( 15.14372185054182651, 31.00000000000000355, 44.57714859939663654 ) ) ;
#25358 = ORIENTED_EDGE ( 'NONE', *, *, #7894, .T. ) ;
#25359 = CARTESIAN_POINT ( 'NONE',  ( 17.99999999999999645, -89.07460286905796920, -81.15544420875052367 ) ) ;
#25360 = ORIENTED_EDGE ( 'NONE', *, *, #38687, .T. ) ;
#25361 = CIRCLE ( 'NONE', #12110, 116.0000000000000000 ) ;
#25362 = EDGE_CURVE ( 'NONE', #15430, #26216, #5727, .T. ) ;
#25363 = CARTESIAN_POINT ( 'NONE',  ( -58.48566925782336057, 40.00000000000000711, -15.65830181329500803 ) ) ;
#25364 = AXIS2_PLACEMENT_3D ( 'NONE', #29472, #19465, #32939 ) ;
#25365 = LINE ( 'NONE', #27776, #22123 ) ;
#25366 = DIRECTION ( 'NONE',  ( 0.000000000000000000, 0.000000000000000000, -1.000000000000000000 ) ) ;
#25367 = DIRECTION ( 'NONE',  ( 1.000000000000000000, 0.000000000000000000, 0.000000000000000000 ) ) ;
#25368 = CARTESIAN_POINT ( 'NONE',  ( -19.76500330823589735, 31.00000000000000355, -5.286999072153966139 ) ) ;
#25369 = MECHANICAL_DESIGN_GEOMETRIC_PRESENTATION_REPRESENTATION (  '', ( #220 ), #2995 ) ;
#25370 = ORIENTED_EDGE ( 'NONE', *, *, #27374, .F. ) ;
#25371 = CARTESIAN_POINT ( 'NONE',  ( 25.50046184691807483, 40.00000000000000000, -22.37655979312362931 ) ) ;
#25372 = ORIENTED_EDGE ( 'NONE', *, *, #42405, .T. ) ;
#25373 = DIRECTION ( 'NONE',  ( 1.000000000000000000, 0.000000000000000000, 0.000000000000000000 ) ) ;
#25374 = AXIS2_PLACEMENT_3D ( 'NONE', #29359, #8414, #35029 ) ;
#25375 = CARTESIAN_POINT ( 'NONE',  ( 0.000000000000000000, 40.47821179127715396, 32.64221760512772619 ) ) ;
#25376 = ORIENTED_EDGE ( 'NONE', *, *, #24225, .F. ) ;
#25377 = CARTESIAN_POINT ( 'NONE',  ( 17.99999999999999645, -112.5120133921104753, -43.14554256761131512 ) ) ;
#25378 = EDGE_CURVE ( 'NONE', #10354, #42137, #26643, .T. ) ;
#25379 = EDGE_LOOP ( 'NONE', ( #33817, #19707, #15585, #7068 ) ) ;
#25380 = DIRECTION ( 'NONE',  ( 0.000000000000000000, -0.3140767120219556952, 0.9493976084683790617 ) ) ;
#25381 = EDGE_LOOP ( 'NONE', ( #13884, #19403, #38061, #6372 ) ) ;
#25382 = AXIS2_PLACEMENT_3D ( 'NONE', #39962, #478, #10325 ) ;
#25383 = ORIENTED_EDGE ( 'NONE', *, *, #27523, .T. ) ;
#25384 = DIRECTION ( 'NONE',  ( -3.892440008040322386E-16, 2.658563593772947863E-15, 1.000000000000000000 ) ) ;
#25385 = CARTESIAN_POINT ( 'NONE',  ( -81.90010630563853056, 31.00000000000000711, 5.248159452637419342 ) ) ;
#25386 = ORIENTED_EDGE ( 'NONE', *, *, #19582, .F. ) ;
#25387 = CARTESIAN_POINT ( 'NONE',  ( 53.80287614962789178, -40.05525454449572464, 69.29271901957253021 ) ) ;
#25388 = CIRCLE ( 'NONE', #30933, 31.49899999999999523 ) ;
#25389 = DIRECTION ( 'NONE',  ( -1.000000000000000000, 0.000000000000000000, 0.000000000000000000 ) ) ;
#25390 = ORIENTED_EDGE ( 'NONE', *, *, #22872, .T. ) ;
#25391 = ADVANCED_FACE ( 'NONE', ( #30104 ), #13317, .F. ) ;
#25392 = CARTESIAN_POINT ( 'NONE',  ( 0.000000000000000000, -7.749090474611287860, -30.53094492177221397 ) ) ;
#25393 = AXIS2_PLACEMENT_3D ( 'NONE', #13546, #29918, #8486 ) ;
#25394 = CARTESIAN_POINT ( 'NONE',  ( -66.59699903142620769, 40.00000000000000711, 75.74378954611491110 ) ) ;
#25395 = CARTESIAN_POINT ( 'NONE',  ( 8.075107282080610460, 31.00000000000000355, -23.73893940452553508 ) ) ;
#25396 = ADVANCED_FACE ( 'NONE', ( #37054 ), #37492, .T. ) ;
#25398 = CARTESIAN_POINT ( 'NONE',  ( 22.90854556226722138, -2.055254544495723756, -74.83297477053847047 ) ) ;
#25397 = PLANE ( 'NONE',  #37071 ) ;
#25399 = DIRECTION ( 'NONE',  ( 0.000000000000000000, -1.000000000000000000, 5.297542245118643184E-16 ) ) ;
#25400 = DIRECTION ( 'NONE',  ( 1.000000000000000000, -0.000000000000000000, -0.000000000000000000 ) ) ;
#25401 = PRODUCT_DEFINITION_FORMATION_WITH_SPECIFIED_SOURCE ( 'ANY', '', #16177, .NOT_KNOWN. ) ;
#25402 = ORIENTED_EDGE ( 'NONE', *, *, #14546, .T. ) ;
#25403 =( LENGTH_UNIT ( ) NAMED_UNIT ( * ) SI_UNIT ( .MILLI., .METRE. ) );
#25404 = DIRECTION ( 'NONE',  ( -1.000000000000000000, -0.000000000000000000, 0.000000000000000000 ) ) ;
#25405 = ORIENTED_EDGE ( 'NONE', *, *, #5102, .T. ) ;
#25406 = DIRECTION ( 'NONE',  ( -1.000000000000000000, -0.000000000000000000, -0.000000000000000000 ) ) ;
#25407 = CARTESIAN_POINT ( 'NONE',  ( 25.17870271038170316, 31.00000000000000355, 93.97695291299892517 ) ) ;
#25408 = CARTESIAN_POINT ( 'NONE',  ( -10.00000000000000000, 0.000000000000000000, 0.000000000000000000 ) ) ;
#25409 = ORIENTED_EDGE ( 'NONE', *, *, #35787, .T. ) ;
#25410 = CARTESIAN_POINT ( 'NONE',  ( -25.30796725786148826, 40.00000000000000000, 14.62256337265529815 ) ) ;
#25411 = CIRCLE ( 'NONE', #6540, 59.00000000000000000 ) ;
#25412 = CARTESIAN_POINT ( 'NONE',  ( 17.12248163736668261, 40.00000000000000000, 34.87662400048956357 ) ) ;
#25413 = ORIENTED_EDGE ( 'NONE', *, *, #32604, .F. ) ;
#25414 = AXIS2_PLACEMENT_3D ( 'NONE', #39153, #19358, #38948 ) ;
#25415 = EDGE_LOOP ( 'NONE', ( #10328, #40559, #6507, #28652 ) ) ;
#25416 = DIRECTION ( 'NONE',  ( -1.000000000000000000, -0.000000000000000000, -0.000000000000000000 ) ) ;
#25417 = CARTESIAN_POINT ( 'NONE',  ( 9.000000000000001776, -51.85248208264514602, -3.914090171286729980 ) ) ;
#25418 = DIRECTION ( 'NONE',  ( 1.000000000000000000, -1.373900992973642066E-15, -3.979293995072266947E-16 ) ) ;
#25419 = AXIS2_PLACEMENT_3D ( 'NONE', #30698, #40691, #10404 ) ;
#25420 = DIRECTION ( 'NONE',  ( 0.000000000000000000, 0.000000000000000000, 1.000000000000000000 ) ) ;
#25421 = DIRECTION ( 'NONE',  ( -3.996523416598930318E-16, 2.658563593772947863E-15, 1.000000000000000000 ) ) ;
#25422 = CIRCLE ( 'NONE', #12176, 59.00000000000000711 ) ;
#25423 = ORIENTED_EDGE ( 'NONE', *, *, #12603, .F. ) ;
#25424 = CARTESIAN_POINT ( 'NONE',  ( 9.000000000000001776, 36.06787431788731624, -37.45808914225450081 ) ) ;
#25425 = ORIENTED_EDGE ( 'NONE', *, *, #8884, .F. ) ;
#25426 = DIRECTION ( 'NONE',  ( 1.000000000000000000, 0.000000000000000000, 0.000000000000000000 ) ) ;
#25427 = CARTESIAN_POINT ( 'NONE',  ( 17.99999999999999645, 114.6488492393084613, -37.09625815499892809 ) ) ;
#25428 = CARTESIAN_POINT ( 'NONE',  ( 0.000000000000000000, 0.000000000000000000, 0.000000000000000000 ) ) ;
#25429 = EDGE_CURVE ( 'NONE', #2013, #3440, #34216, .T. ) ;
#25430 = CARTESIAN_POINT ( 'NONE',  ( 18.00000000000000355, 36.34385289850631295, -29.77717097092038756 ) ) ;
#25431 = ORIENTED_EDGE ( 'NONE', *, *, #12995, .T. ) ;
#25432 = VERTEX_POINT ( 'NONE', #26609 ) ;
#25433 = EDGE_CURVE ( 'NONE', #10114, #6869, #20306, .T. ) ;
#25434 = LINE ( 'NONE', #41966, #32568 ) ;
#25435 = CIRCLE ( 'NONE', #6565, 116.0000000000000000 ) ;
#25436 = VERTEX_POINT ( 'NONE', #33570 ) ;
#25438 = ORIENTED_EDGE ( 'NONE', *, *, #35351, .T. ) ;
#25437 = CARTESIAN_POINT ( 'NONE',  ( -105.0363123600777442, 17.11489954122026447, -2.692529638013756887 ) ) ;
#25439 = CARTESIAN_POINT ( 'NONE',  ( 38.48770111205617894, 31.00000000000000355, 44.02435964457617956 ) ) ;
#25440 = VERTEX_POINT ( 'NONE', #20101 ) ;
#25441 = CARTESIAN_POINT ( 'NONE',  ( 0.000000000000000000, 0.000000000000000000, 0.000000000000000000 ) ) ;
#25442 = CIRCLE ( 'NONE', #22671, 20.00000000000000711 ) ;
#25443 = EDGE_CURVE ( 'NONE', #32065, #3164, #4317, .T. ) ;
#25444 = LINE ( 'NONE', #25040, #2837 ) ;
#25445 = ORIENTED_EDGE ( 'NONE', *, *, #29851, .F. ) ;
#25446 = CARTESIAN_POINT ( 'NONE',  ( -67.85934734800838442, 40.00000000000000711, 22.92939687791763248 ) ) ;
#25447 = CIRCLE ( 'NONE', #27511, 47.49900000000000233 ) ;
#25448 = EDGE_CURVE ( 'NONE', #13710, #38742, #7383, .T. ) ;
#25449 = CARTESIAN_POINT ( 'NONE',  ( 17.99999999999999645, -120.2856157092986393, -7.201503623198056481 ) ) ;
#25450 = AXIS2_PLACEMENT_3D ( 'NONE', #25463, #12779, #22207 ) ;
#25451 = CYLINDRICAL_SURFACE ( 'NONE', #38686, 51.99999999999999289 ) ;
#25452 = EDGE_LOOP ( 'NONE', ( #23051, #41325, #12638, #9327 ) ) ;
#25453 = CARTESIAN_POINT ( 'NONE',  ( -142.5000000000000284, 1.627194001049074632E-13, 6.999999999999945821 ) ) ;
#25454 = ORIENTED_EDGE ( 'NONE', *, *, #5762, .T. ) ;
#25455 = PRESENTATION_STYLE_ASSIGNMENT (( #9052 ) ) ;
#25456 = AXIS2_PLACEMENT_3D ( 'NONE', #4443, #27837, #37615 ) ;
#25457 = DIRECTION ( 'NONE',  ( -1.000000000000000000, -0.000000000000000000, -0.000000000000000000 ) ) ;
#25458 = CARTESIAN_POINT ( 'NONE',  ( -91.96080130434583566, -12.05525454449572109, 14.45886780445738395 ) ) ;
#25459 = CARTESIAN_POINT ( 'NONE',  ( -8.856203846296160975, 31.00000000000000355, 67.27320953167645712 ) ) ;
#25461 = DIRECTION ( 'NONE',  ( 0.000000000000000000, 0.000000000000000000, 1.000000000000000000 ) ) ;
#25460 = DIRECTION ( 'NONE',  ( 0.000000000000000000, 0.000000000000000000, 1.000000000000000000 ) ) ;
#25462 = VERTEX_POINT ( 'NONE', #43162 ) ;
#25463 = CARTESIAN_POINT ( 'NONE',  ( 18.00000000000000355, -5.667686777401384823, -46.64153600743609474 ) ) ;
#25464 = EDGE_CURVE ( 'NONE', #287, #21478, #10005, .T. ) ;
#25465 = ORIENTED_EDGE ( 'NONE', *, *, #25813, .T. ) ;
#25466 = CARTESIAN_POINT ( 'NONE',  ( 0.000000000000000000, 0.000000000000000000, 0.000000000000000000 ) ) ;
#25467 = EDGE_CURVE ( 'NONE', #40494, #1834, #3870, .T. ) ;
#25468 = FACE_OUTER_BOUND ( 'NONE', #951, .T. ) ;
#25469 = CARTESIAN_POINT ( 'NONE',  ( 52.26791824981292223, 31.00000000000000355, -67.94187691988643962 ) ) ;
#25470 = CARTESIAN_POINT ( 'NONE',  ( 27.50146173784981229, 40.00000000000000000, -80.63904244945182143 ) ) ;
#25471 = CIRCLE ( 'NONE', #34489, 47.49899999999999523 ) ;
#25472 = CARTESIAN_POINT ( 'NONE',  ( 17.99999999999999645, -9.484061862024134371, 30.03730300138978038 ) ) ;
#25473 = CIRCLE ( 'NONE', #3098, 116.0000000000000000 ) ;
#25474 = VERTEX_POINT ( 'NONE', #20741 ) ;
#25475 = CARTESIAN_POINT ( 'NONE',  ( 17.99999999999999645, 0.000000000000000000, 0.000000000000000000 ) ) ;
#25476 = VERTEX_POINT ( 'NONE', #26820 ) ;
#25477 = DIRECTION ( 'NONE',  ( 0.000000000000000000, 0.000000000000000000, 1.000000000000000000 ) ) ;
#25478 = AXIS2_PLACEMENT_3D ( 'NONE', #28583, #31843, #1712 ) ;
#25479 = AXIS2_PLACEMENT_3D ( 'NONE', #30008, #40431, #6855 ) ;
#25481 = EDGE_LOOP ( 'NONE', ( #2456, #5642, #34268, #17084 ) ) ;
#25480 = CARTESIAN_POINT ( 'NONE',  ( 18.00000000000000355, 0.000000000000000000, 0.000000000000000000 ) ) ;
#25482 = CARTESIAN_POINT ( 'NONE',  ( 0.000000000000000000, 0.000000000000000000, 0.000000000000000000 ) ) ;
#25483 = VERTEX_POINT ( 'NONE', #4093 ) ;
#25484 = CARTESIAN_POINT ( 'NONE',  ( 0.000000000000000000, -91.65951123222531294, 71.09524597798055368 ) ) ;
#25485 = EDGE_CURVE ( 'NONE', #2881, #9347, #12761, .T. ) ;
#25486 = LINE ( 'NONE', #22231, #31157 ) ;
#25487 = AXIS2_PLACEMENT_3D ( 'NONE', #19102, #8590, #2449 ) ;
#25488 = DIRECTION ( 'NONE',  ( 1.000000000000000000, 0.000000000000000000, -6.546126324440850663E-16 ) ) ;
#25489 = ORIENTED_EDGE ( 'NONE', *, *, #13223, .T. ) ;
#25490 = CARTESIAN_POINT ( 'NONE',  ( 24.91045342551303321, 31.00000000000000355, 12.31387362277163433 ) ) ;
#25491 = CARTESIAN_POINT ( 'NONE',  ( 17.99999999999999645, -97.19627249181047546, -71.22763238166585609 ) ) ;
#25492 = EDGE_CURVE ( 'NONE', #28980, #8515, #23895, .T. ) ;
#25494 = CARTESIAN_POINT ( 'NONE',  ( 17.99999999999999645, -5.456439917445724319, 112.0647122740741963 ) ) ;
#25493 = CARTESIAN_POINT ( 'NONE',  ( 17.99999999999999645, 101.1403355683146117, 56.80345518653518866 ) ) ;
#25495 = ORIENTED_EDGE ( 'NONE', *, *, #25813, .F. ) ;
#25496 = DIRECTION ( 'NONE',  ( 1.000000000000000000, -0.000000000000000000, 0.000000000000000000 ) ) ;
#25497 = CARTESIAN_POINT ( 'NONE',  ( -3.355112389629170799, 2.681727112203152963, -0.2256878752776689534 ) ) ;
#25499 = AXIS2_PLACEMENT_3D ( 'NONE', #28875, #39288, #32557 ) ;
#25498 = CARTESIAN_POINT ( 'NONE',  ( -2.829072032612394594, 40.00000000000000000, -44.39959014221900446 ) ) ;
#25500 = LINE ( 'NONE', #22242, #38376 ) ;
#25501 = EDGE_CURVE ( 'NONE', #27165, #508, #35290, .T. ) ;
#25502 = AXIS2_PLACEMENT_3D ( 'NONE', #27200, #7756, #34153 ) ;
#25503 = DIRECTION ( 'NONE',  ( -1.000000000000000000, -0.000000000000000000, 0.000000000000000000 ) ) ;
#25504 = CIRCLE ( 'NONE', #24096, 52.00000000000000000 ) ;
#25505 = AXIS2_PLACEMENT_3D ( 'NONE', #19454, #28828, #16163 ) ;
#25506 = CYLINDRICAL_SURFACE ( 'NONE', #40833, 20.00000000000000355 ) ;
#25508 = ORIENTED_EDGE ( 'NONE', *, *, #18917, .T. ) ;
#25507 = CIRCLE ( 'NONE', #24831, 116.0000000000000000 ) ;
#25509 = CARTESIAN_POINT ( 'NONE',  ( 0.000000000000000000, 0.000000000000000000, 0.000000000000000000 ) ) ;
#25510 = CIRCLE ( 'NONE', #6642, 120.5010000000000190 ) ;
#25511 = VERTEX_POINT ( 'NONE', #4770 ) ;
#25512 = VECTOR ( 'NONE', #21795, 1000.000000000000000 ) ;
#25513 = DIRECTION ( 'NONE',  ( 0.000000000000000000, 0.000000000000000000, 1.000000000000000000 ) ) ;
#25514 = DIRECTION ( 'NONE',  ( 1.000000000000000000, 0.000000000000000000, -0.000000000000000000 ) ) ;
#25515 = AXIS2_PLACEMENT_3D ( 'NONE', #17414, #37432, #17196 ) ;
#25516 = CARTESIAN_POINT ( 'NONE',  ( 34.28525303991722240, 31.00000000000000355, 9.176237600273646322 ) ) ;
#25517 = ORIENTED_EDGE ( 'NONE', *, *, #13797, .F. ) ;
#25518 = DIRECTION ( 'NONE',  ( 1.000000000000000000, 0.000000000000000000, 0.000000000000000000 ) ) ;
#25520 = ORIENTED_EDGE ( 'NONE', *, *, #7153, .F. ) ;
#25519 = STYLED_ITEM ( 'NONE', ( #26836 ), #28157 ) ;
#25522 = CIRCLE ( 'NONE', #15753, 116.0000000000000000 ) ;
#25521 = CARTESIAN_POINT ( 'NONE',  ( -0.2999999999999999889, -14.69693845669906906, -1.199999999999999956 ) ) ;
#25523 = CARTESIAN_POINT ( 'NONE',  ( -87.52616871875942195, 31.00000000000000711, -23.43677886868077209 ) ) ;
#25524 = EDGE_CURVE ( 'NONE', #25059, #10533, #1909, .T. ) ;
#25525 = EDGE_LOOP ( 'NONE', ( #25341, #6076, #10017, #32746 ) ) ;
#25526 = CARTESIAN_POINT ( 'NONE',  ( -46.12092335262209986, 31.00000000000000355, 22.64177125690870795 ) ) ;
#25527 = EDGE_CURVE ( 'NONE', #20683, #22786, #34322, .T. ) ;
#25528 = CARTESIAN_POINT ( 'NONE',  ( -86.71682804797315214, 40.00000000000000711, 23.23408344657299196 ) ) ;
#25529 = VERTEX_POINT ( 'NONE', #38550 ) ;
#25530 = DIRECTION ( 'NONE',  ( 1.000000000000000000, 0.000000000000000000, 0.000000000000000000 ) ) ;
#25531 = DIRECTION ( 'NONE',  ( -1.000000000000000000, 0.000000000000000000, 0.000000000000000000 ) ) ;
#25532 = DIRECTION ( 'NONE',  ( 0.000000000000000000, -1.000000000000000000, 5.297542245118643184E-16 ) ) ;
#25533 = VECTOR ( 'NONE', #40422, 1000.000000000000000 ) ;
#25535 = ORIENTED_EDGE ( 'NONE', *, *, #21243, .F. ) ;
#25534 = CARTESIAN_POINT ( 'NONE',  ( 0.000000000000000000, 116.4607004671432406, -30.94182036827089632 ) ) ;
#25536 = CIRCLE ( 'NONE', #16457, 15.99999999999998934 ) ;
#25537 = DIRECTION ( 'NONE',  ( -1.000000000000000000, -0.000000000000000000, -0.000000000000000000 ) ) ;
#25538 = CIRCLE ( 'NONE', #9488, 120.5010000000000190 ) ;
#25539 = FACE_OUTER_BOUND ( 'NONE', #41909, .T. ) ;
#25540 = AXIS2_PLACEMENT_3D ( 'NONE', #36570, #572, #10409 ) ;
#25541 = ORIENTED_EDGE ( 'NONE', *, *, #21175, .F. ) ;
#25542 = CARTESIAN_POINT ( 'NONE',  ( -77.03666156126601550, 40.00000000000000711, 20.64125776147949409 ) ) ;
#25543 = DIRECTION ( 'NONE',  ( -0.000000000000000000, -0.000000000000000000, 1.000000000000000000 ) ) ;
#25544 = ORIENTED_EDGE ( 'NONE', *, *, #15080, .F. ) ;
#25545 = AXIS2_PLACEMENT_3D ( 'NONE', #18285, #31550, #8411 ) ;
#25546 = DIRECTION ( 'NONE',  ( -1.000000000000000000, -0.000000000000000000, -0.000000000000000000 ) ) ;
#25547 = VECTOR ( 'NONE', #16330, 1000.000000000000000 ) ;
#25548 = AXIS2_PLACEMENT_3D ( 'NONE', #867, #3923, #24281 ) ;
#25549 = ORIENTED_EDGE ( 'NONE', *, *, #21940, .F. ) ;
#25550 = CIRCLE ( 'NONE', #42214, 126.0000000000000284 ) ;
#25551 = EDGE_CURVE ( 'NONE', #26402, #4469, #10630, .T. ) ;
#25552 = ORIENTED_EDGE ( 'NONE', *, *, #3259, .F. ) ;
#25553 = CARTESIAN_POINT ( 'NONE',  ( 0.000000000000000000, 0.000000000000000000, -6.000000000000000000 ) ) ;
#25554 = VERTEX_POINT ( 'NONE', #11776 ) ;
#25555 = DIRECTION ( 'NONE',  ( 0.000000000000000000, -0.7705132427757949154, 0.6374239897486827511 ) ) ;
#25556 = CARTESIAN_POINT ( 'NONE',  ( 17.99999999999999645, 93.26762629039428987, 76.29967815892386795 ) ) ;
#25557 = EDGE_CURVE ( 'NONE', #21131, #4386, #31562, .T. ) ;
#25558 = DIRECTION ( 'NONE',  ( -1.000000000000000000, -0.000000000000000000, -0.000000000000000000 ) ) ;
#25559 = PLANE ( 'NONE',  #398 ) ;
#25560 = ORIENTED_EDGE ( 'NONE', *, *, #8717, .F. ) ;
#25561 = DIRECTION ( 'NONE',  ( -1.000000000000000000, -0.000000000000000000, -0.000000000000000000 ) ) ;
#25562 = ORIENTED_EDGE ( 'NONE', *, *, #27668, .T. ) ;
#25563 = DIRECTION ( 'NONE',  ( -1.000000000000000000, 0.000000000000000000, -0.000000000000000000 ) ) ;
#25565 = VERTEX_POINT ( 'NONE', #28567 ) ;
#25564 = AXIS2_PLACEMENT_3D ( 'NONE', #7920, #11870, #25198 ) ;
#25566 = CARTESIAN_POINT ( 'NONE',  ( 0.000000000000000000, -95.38615066513943930, -59.07414607872924250 ) ) ;
#25567 = VECTOR ( 'NONE', #39276, 1000.000000000000000 ) ;
#25568 = DIRECTION ( 'NONE',  ( 1.000000000000000000, 0.000000000000000000, 0.000000000000000000 ) ) ;
#25569 = VECTOR ( 'NONE', #26759, 1000.000000000000000 ) ;
#25570 = DIRECTION ( 'NONE',  ( 4.329780281177519431E-17, 1.000000000000000000, 4.329780281177414044E-17 ) ) ;
#25571 = DIRECTION ( 'NONE',  ( 1.000000000000000000, 0.000000000000000000, 0.000000000000000000 ) ) ;
#25572 = CARTESIAN_POINT ( 'NONE',  ( -49.46937513889707105, 31.00000000000000355, 6.524320044134898744 ) ) ;
#25573 = ORIENTED_EDGE ( 'NONE', *, *, #36398, .T. ) ;
#25574 = MECHANICAL_DESIGN_GEOMETRIC_PRESENTATION_REPRESENTATION (  '', ( #2525 ), #17230 ) ;
#25575 = DIRECTION ( 'NONE',  ( -1.000000000000000000, 1.577021341797063787E-16, 0.000000000000000000 ) ) ;
#25576 = ADVANCED_FACE ( 'NONE', ( #1034 ), #15279, .F. ) ;
#25577 = EDGE_CURVE ( 'NONE', #15863, #39379, #14141, .T. ) ;
#25578 = ORIENTED_EDGE ( 'NONE', *, *, #19036, .T. ) ;
#25579 = AXIS2_PLACEMENT_3D ( 'NONE', #41802, #15644, #18746 ) ;
#25580 = EDGE_CURVE ( 'NONE', #40340, #13758, #19042, .T. ) ;
#25581 = ADVANCED_FACE ( 'NONE', ( #11542 ), #8260, .F. ) ;
#25582 = CARTESIAN_POINT ( 'NONE',  ( 38.75409931461306456, 40.00000000000000000, -50.52625141960567134 ) ) ;
#25583 = CIRCLE ( 'NONE', #42250, 2.649999999999957723 ) ;
#25584 = LINE ( 'NONE', #27014, #8840 ) ;
#25585 = DIRECTION ( 'NONE',  ( 0.000000000000000000, 0.000000000000000000, 1.000000000000000000 ) ) ;
#25586 = AXIS2_PLACEMENT_3D ( 'NONE', #9907, #40429, #6629 ) ;
#25587 = DIRECTION ( 'NONE',  ( 1.058513553088275437E-16, 1.000000000000000000, -8.813324511995299047E-17 ) ) ;
#25588 = CARTESIAN_POINT ( 'NONE',  ( 2.164352920501968783E-14, -1.058809993658035131E-13, -39.99999999999997868 ) ) ;
#25589 = PRODUCT_DEFINITION_SHAPE ( 'NONE', 'NONE',  #43204 ) ;
#25590 = VERTEX_POINT ( 'NONE', #25100 ) ;
#25591 = CARTESIAN_POINT ( 'NONE',  ( 30.80114556864472775, 40.00000000000000000, -15.19345985420777190 ) ) ;
#25592 = EDGE_LOOP ( 'NONE', ( #10591, #40713, #39591, #40683 ) ) ;
#25593 = DIRECTION ( 'NONE',  ( 0.000000000000000000, 0.000000000000000000, 1.000000000000000000 ) ) ;
#25594 = CARTESIAN_POINT ( 'NONE',  ( 17.99999999999999645, 0.000000000000000000, 0.000000000000000000 ) ) ;
#25595 = ORIENTED_EDGE ( 'NONE', *, *, #41477, .T. ) ;
#25596 = AXIS2_PLACEMENT_3D ( 'NONE', #38105, #8231, #21589 ) ;
#25597 = LINE ( 'NONE', #38635, #1259 ) ;
#25598 = EDGE_LOOP ( 'NONE', ( #28443, #25948, #31184, #34124 ) ) ;
#25599 = CARTESIAN_POINT ( 'NONE',  ( 18.00000000000000355, -12.30077720129062868, -50.52416135122093976 ) ) ;
#25600 = ORIENTED_EDGE ( 'NONE', *, *, #34353, .F. ) ;
#25601 = AXIS2_PLACEMENT_3D ( 'NONE', #40644, #21527, #4219 ) ;
#25602 = ORIENTED_EDGE ( 'NONE', *, *, #9276, .T. ) ;
#25603 = CIRCLE ( 'NONE', #6063, 58.99999999999999289 ) ;
#25604 = CARTESIAN_POINT ( 'NONE',  ( 17.99999999999999645, 24.22031524826126514, -109.5520369638034879 ) ) ;
#25605 = CARTESIAN_POINT ( 'NONE',  ( -20.82795069773117547, 31.00000000000000355, 77.32795358076221248 ) ) ;
#25606 = ORIENTED_EDGE ( 'NONE', *, *, #4961, .F. ) ;
#25607 = CARTESIAN_POINT ( 'NONE',  ( 17.99999999999999645, -115.5737863835462917, 9.934782381633276316 ) ) ;
#25608 = AXIS2_PLACEMENT_3D ( 'NONE', #40232, #36966, #526 ) ;
#25609 = DIRECTION ( 'NONE',  ( 0.000000000000000000, 0.000000000000000000, 1.000000000000000000 ) ) ;
#25610 = ORIENTED_EDGE ( 'NONE', *, *, #31463, .F. ) ;
#25611 = DIRECTION ( 'NONE',  ( -1.000000000000000000, -0.000000000000000000, -0.000000000000000000 ) ) ;
#25612 = CARTESIAN_POINT ( 'NONE',  ( -50.38378093996033869, 40.00000000000000711, 87.00968337440519917 ) ) ;
#25613 = CARTESIAN_POINT ( 'NONE',  ( -20.42974159057666483, 31.00000000000000355, -10.07157319949386753 ) ) ;
#25615 = DIRECTION ( 'NONE',  ( 0.000000000000000000, 0.9968120070307504577, -0.07978610555307977248 ) ) ;
#25614 = LINE ( 'NONE', #22990, #16905 ) ;
#25616 = FACE_OUTER_BOUND ( 'NONE', #27352, .T. ) ;
#25617 = DIRECTION ( 'NONE',  ( 0.000000000000000000, 0.000000000000000000, 1.000000000000000000 ) ) ;
#25618 = EDGE_LOOP ( 'NONE', ( #22520, #41001, #5895, #5631 ) ) ;
#25619 = FILL_AREA_STYLE_COLOUR ( '', #35946 ) ;
#25620 = ORIENTED_EDGE ( 'NONE', *, *, #6280, .F. ) ;
#25621 = DIRECTION ( 'NONE',  ( 1.000000000000000000, 0.000000000000000000, 0.000000000000000000 ) ) ;
#25622 = CARTESIAN_POINT ( 'NONE',  ( 0.000000000000000000, 106.5605152861902951, 56.26142179985861702 ) ) ;
#25623 = AXIS2_PLACEMENT_3D ( 'NONE', #34133, #18048, #37614 ) ;
#25624 = EDGE_LOOP ( 'NONE', ( #13180, #22848 ) ) ;
#25625 = EDGE_CURVE ( 'NONE', #17206, #1617, #18336, .T. ) ;
#25626 = ADVANCED_FACE ( 'NONE', ( #28355 ), #8465, .F. ) ;
#25627 = CARTESIAN_POINT ( 'NONE',  ( 2.127120017302678523, 40.00000000000000000, -32.60416666460785962 ) ) ;
#25628 = AXIS2_PLACEMENT_3D ( 'NONE', #29052, #24955, #25585 ) ;
#25629 = CARTESIAN_POINT ( 'NONE',  ( -2.197745971917953511, 40.00000000000000000, -34.39891587002171747 ) ) ;
#25630 = AXIS2_PLACEMENT_3D ( 'NONE', #22118, #35577, #15762 ) ;
#25631 = EDGE_CURVE ( 'NONE', #22284, #32317, #5049, .T. ) ;
#25632 = AXIS2_PLACEMENT_3D ( 'NONE', #785, #8225, #20705 ) ;
#25633 = ORIENTED_EDGE ( 'NONE', *, *, #4116, .F. ) ;
#25634 = AXIS2_PLACEMENT_3D ( 'NONE', #26055, #6392, #12542 ) ;
#25635 = VERTEX_POINT ( 'NONE', #41622 ) ;
#25636 = DIRECTION ( 'NONE',  ( -1.000000000000000000, -0.000000000000000000, -0.000000000000000000 ) ) ;
#25637 = DIRECTION ( 'NONE',  ( -1.000000000000000000, 0.000000000000000000, 0.000000000000000000 ) ) ;
#25638 = DIRECTION ( 'NONE',  ( 1.000000000000000000, 0.000000000000000000, 0.000000000000000000 ) ) ;
#25639 = AXIS2_PLACEMENT_3D ( 'NONE', #8537, #21482, #31472 ) ;
#25640 = DIRECTION ( 'NONE',  ( 0.000000000000000000, 0.000000000000000000, 1.000000000000000000 ) ) ;
#25641 = EDGE_CURVE ( 'NONE', #23944, #31256, #11323, .T. ) ;
#25642 = CARTESIAN_POINT ( 'NONE',  ( -10.00000000000000000, 0.000000000000000000, 0.000000000000000000 ) ) ;
#25643 = EDGE_LOOP ( 'NONE', ( #29876, #31038, #34307, #22110 ) ) ;
#25644 = CYLINDRICAL_SURFACE ( 'NONE', #38853, 142.5000000000000284 ) ;
#25645 = ORIENTED_EDGE ( 'NONE', *, *, #2272, .F. ) ;
#25646 = CARTESIAN_POINT ( 'NONE',  ( 17.99999999999999645, 0.000000000000000000, 0.000000000000000000 ) ) ;
#25647 = FACE_BOUND ( 'NONE', #10572, .T. ) ;
#25648 = CIRCLE ( 'NONE', #36739, 13.60000000000000142 ) ;
#25649 = EDGE_CURVE ( 'NONE', #32279, #14258, #1692, .T. ) ;
#25650 = DIRECTION ( 'NONE',  ( -3.996523416598930318E-16, 2.658563593772947863E-15, 1.000000000000000000 ) ) ;
#25651 = DIRECTION ( 'NONE',  ( -1.058513553088275437E-16, -1.000000000000000000, 8.813324511995299047E-17 ) ) ;
#25652 = EDGE_LOOP ( 'NONE', ( #24348, #30753, #11168, #42238 ) ) ;
#25653 = CARTESIAN_POINT ( 'NONE',  ( -85.90019077458921970, 40.00000000000000711, -29.16093118951848240 ) ) ;
#25654 = ORIENTED_EDGE ( 'NONE', *, *, #10934, .F. ) ;
#25655 = CARTESIAN_POINT ( 'NONE',  ( 17.99999999999999645, -117.6086855750632765, -26.24286718912224003 ) ) ;
#25656 = VERTEX_POINT ( 'NONE', #17904 ) ;
#25658 = ORIENTED_EDGE ( 'NONE', *, *, #26290, .F. ) ;
#25657 = CARTESIAN_POINT ( 'NONE',  ( 9.000000000000001776, -41.60679253225688967, -108.2814610871950265 ) ) ;
#25659 = CARTESIAN_POINT ( 'NONE',  ( -52.09564885853935579, 31.00000000000000355, -3.498939618562641574 ) ) ;
#25660 = VERTEX_POINT ( 'NONE', #31180 ) ;
#25661 = LINE ( 'NONE', #29340, #21711 ) ;
#25662 = VECTOR ( 'NONE', #5952, 1000.000000000000000 ) ;
#25663 = AXIS2_PLACEMENT_3D ( 'NONE', #20977, #34442, #404 ) ;
#25664 = DIRECTION ( 'NONE',  ( 0.000000000000000000, 0.000000000000000000, 1.000000000000000000 ) ) ;
#25665 = ORIENTED_EDGE ( 'NONE', *, *, #6525, .T. ) ;
#25666 = CIRCLE ( 'NONE', #40243, 58.99999999999997868 ) ;
#25667 = CARTESIAN_POINT ( 'NONE',  ( -18.22940504111446458, 40.00000000000000000, 67.64968002090884625 ) ) ;
#25668 = AXIS2_PLACEMENT_3D ( 'NONE', #680, #14041, #40824 ) ;
#25670 = CARTESIAN_POINT ( 'NONE',  ( 0.000000000000000000, 78.18175027177430536, 85.69488855493025881 ) ) ;
#25669 = LINE ( 'NONE', #36494, #2850 ) ;
#25671 = CARTESIAN_POINT ( 'NONE',  ( 17.99999999999999645, -24.70533337038204635, -26.18485254986720179 ) ) ;
#25672 = VERTEX_POINT ( 'NONE', #1269 ) ;
#25673 = CARTESIAN_POINT ( 'NONE',  ( 150.0000507999999968, 9.184850993605147944E-16, -7.500000000000000000 ) ) ;
#25674 = EDGE_LOOP ( 'NONE', ( #261, #12499, #25823 ) ) ;
#25675 = APPLICATION_CONTEXT ( 'automotive_design' ) ;
#25676 = DIRECTION ( 'NONE',  ( 1.000000000000000000, 0.000000000000000000, 0.000000000000000000 ) ) ;
#25677 = CARTESIAN_POINT ( 'NONE',  ( 18.00000000000000355, 0.000000000000000000, 0.000000000000000000 ) ) ;
#25678 = VECTOR ( 'NONE', #20676, 1000.000000000000000 ) ;
#25679 = CARTESIAN_POINT ( 'NONE',  ( 48.10206620145878276, 31.00000000000000355, -42.20136231105875879 ) ) ;
#25681 = CARTESIAN_POINT ( 'NONE',  ( 0.000000000000000000, 79.94368240339424858, 90.16373242487935613 ) ) ;
#25680 = DIRECTION ( 'NONE',  ( -1.058513553088275437E-16, -1.000000000000000000, 8.813324511995299047E-17 ) ) ;
#25682 = ORIENTED_EDGE ( 'NONE', *, *, #27484, .F. ) ;
#25683 = ADVANCED_FACE ( 'NONE', ( #15046 ), #14613, .F. ) ;
#25684 = CARTESIAN_POINT ( 'NONE',  ( 9.000000000000001776, -52.88069566989388903, -103.2454939717374032 ) ) ;
#25685 = ORIENTED_EDGE ( 'NONE', *, *, #36752, .T. ) ;
#25686 = DIRECTION ( 'NONE',  ( 0.000000000000000000, 0.8951632913550634507, -0.4457383557765359217 ) ) ;
#25687 = CARTESIAN_POINT ( 'NONE',  ( -101.9145453900123641, 40.00000000000000000, -1.407535261550449501 ) ) ;
#25688 = AXIS2_PLACEMENT_3D ( 'NONE', #8977, #21899, #22535 ) ;
#25689 = CARTESIAN_POINT ( 'NONE',  ( 97.09201668843397215, 31.00000000000000000, 6.474068422258194566 ) ) ;
#25690 = CARTESIAN_POINT ( 'NONE',  ( 12.51314706078825090, 40.00000000000000000, -94.07914177280382262 ) ) ;
#25691 = EDGE_CURVE ( 'NONE', #20648, #33175, #7851, .T. ) ;
#25692 = DIRECTION ( 'NONE',  ( 0.000000000000000000, 0.000000000000000000, 1.000000000000000000 ) ) ;
#25693 = CIRCLE ( 'NONE', #31928, 0.7500000000000006661 ) ;
#25694 = EDGE_CURVE ( 'NONE', #7587, #39801, #32920, .T. ) ;
#25695 = EDGE_LOOP ( 'NONE', ( #4396, #21368, #20711, #43025 ) ) ;
#25696 = CARTESIAN_POINT ( 'NONE',  ( -10.00000000000000000, 0.000000000000000000, 0.000000000000000000 ) ) ;
#25697 = AXIS2_PLACEMENT_3D ( 'NONE', #7921, #17786, #31063 ) ;
#25698 = ORIENTED_EDGE ( 'NONE', *, *, #13590, .T. ) ;
#25699 = VECTOR ( 'NONE', #16690, 1000.000000000000000 ) ;
#25700 = DIRECTION ( 'NONE',  ( 1.000000000000000000, 0.000000000000000000, 0.000000000000000000 ) ) ;
#25701 = EDGE_CURVE ( 'NONE', #20343, #33862, #19600, .T. ) ;
#25702 = CIRCLE ( 'NONE', #31253, 2.649999999999979039 ) ;
#25704 = ORIENTED_EDGE ( 'NONE', *, *, #12557, .T. ) ;
#25703 = FACE_OUTER_BOUND ( 'NONE', #23390, .T. ) ;
#25705 = DIRECTION ( 'NONE',  ( 1.000000000000000000, 0.000000000000000000, 0.000000000000000000 ) ) ;
#25706 = EDGE_LOOP ( 'NONE', ( #32949, #5926, #38756, #24749 ) ) ;
#25707 = LINE ( 'NONE', #32008, #15470 ) ;
#25708 = DIRECTION ( 'NONE',  ( 0.000000000000000000, 0.000000000000000000, 1.000000000000000000 ) ) ;
#25709 = FACE_OUTER_BOUND ( 'NONE', #21084, .T. ) ;
#25710 = EDGE_LOOP ( 'NONE', ( #24278, #23580, #33025, #19447 ) ) ;
#25711 = CARTESIAN_POINT ( 'NONE',  ( 14.33709021557830887, 31.00000000000000355, 24.89380824183666263 ) ) ;
#25712 = FACE_OUTER_BOUND ( 'NONE', #41037, .T. ) ;
#25713 = EDGE_CURVE ( 'NONE', #1487, #18549, #28983, .T. ) ;
#25715 = EDGE_LOOP ( 'NONE', ( #10471, #14216 ) ) ;
#25714 = CARTESIAN_POINT ( 'NONE',  ( 18.00000000000000355, 42.41764978026607480, -20.20639853260305685 ) ) ;
#25716 = ORIENTED_EDGE ( 'NONE', *, *, #717, .T. ) ;
#25717 = DIRECTION ( 'NONE',  ( -1.000000000000000000, 0.000000000000000000, -0.000000000000000000 ) ) ;
#25718 = ADVANCED_FACE ( 'NONE', ( #13050 ), #23100, .F. ) ;
#25719 = CARTESIAN_POINT ( 'NONE',  ( 17.99999999999999645, 35.78425302087538995, 3.935382540232922111 ) ) ;
#25720 = CARTESIAN_POINT ( 'NONE',  ( -12.95950413119146205, 40.00000000000000000, 37.95406330258916938 ) ) ;
#25721 = FACE_OUTER_BOUND ( 'NONE', #8468, .T. ) ;
#25722 = EDGE_CURVE ( 'NONE', #287, #41800, #13452, .T. ) ;
#25723 = CARTESIAN_POINT ( 'NONE',  ( 1.411581201560190495E-15, 4.862606272033091592, -3.745885042887436622 ) ) ;
#25724 = CARTESIAN_POINT ( 'NONE',  ( 8.999999999999998224, 68.63002662989747193, 93.51962064069530811 ) ) ;
#25725 = VERTEX_POINT ( 'NONE', #6255 ) ;
#25726 = CONICAL_SURFACE ( 'NONE', #18774, 2.055000000000000160, 0.7853981633974639331 ) ;
#25727 = FACE_OUTER_BOUND ( 'NONE', #16245, .T. ) ;
#25728 = ORIENTED_EDGE ( 'NONE', *, *, #36157, .F. ) ;
#25729 = DIRECTION ( 'NONE',  ( -1.000000000000000000, 0.000000000000000000, 0.000000000000000000 ) ) ;
#25730 = DIRECTION ( 'NONE',  ( 0.000000000000000000, 0.000000000000000000, 1.000000000000000000 ) ) ;
#25731 = CARTESIAN_POINT ( 'NONE',  ( 16.30133787010129254, 31.00000000000000355, 33.04822796959624753 ) ) ;
#25732 = ORIENTED_EDGE ( 'NONE', *, *, #10869, .F. ) ;
#25733 = CARTESIAN_POINT ( 'NONE',  ( -91.96080130434580724, -12.05525454449571043, 14.45886780445738218 ) ) ;
#25734 = EDGE_LOOP ( 'NONE', ( #5099, #38124, #7949, #29144 ) ) ;
#25735 = EDGE_CURVE ( 'NONE', #15816, #21731, #5760, .T. ) ;
#25736 = CARTESIAN_POINT ( 'NONE',  ( 17.99999999999999645, 0.000000000000000000, 0.000000000000000000 ) ) ;
#25737 = CARTESIAN_POINT ( 'NONE',  ( -5.726861599740728614, 31.00000000000000355, 87.60416666588449175 ) ) ;
#25738 = DIRECTION ( 'NONE',  ( 1.000000000000000000, 1.836909530733573776E-16, 0.000000000000000000 ) ) ;
#25739 = ORIENTED_EDGE ( 'NONE', *, *, #3326, .T. ) ;
#25740 = CARTESIAN_POINT ( 'NONE',  ( 58.81396797841471624, 31.00000000000000355, 34.08301911901634895 ) ) ;
#25741 = CARTESIAN_POINT ( 'NONE',  ( 34.31975892712151222, 40.00000000000000000, 59.64049725130580271 ) ) ;
#25742 = CARTESIAN_POINT ( 'NONE',  ( 94.89583333399441756, 39.99999999999999289, -6.217735451874103703 ) ) ;
#25743 = ADVANCED_FACE ( 'NONE', ( #26354 ), #6045, .F. ) ;
#25744 = ORIENTED_EDGE ( 'NONE', *, *, #26488, .F. ) ;
#25745 = CARTESIAN_POINT ( 'NONE',  ( 17.99999999999999645, -28.62203781742993414, -14.19692359621484989 ) ) ;
#25746 = DIRECTION ( 'NONE',  ( 0.000000000000000000, 0.000000000000000000, 1.000000000000000000 ) ) ;
#25747 = CARTESIAN_POINT ( 'NONE',  ( 9.000000000000001776, 115.9387338813862129, -3.769613505534868736 ) ) ;
#25748 = AXIS2_PLACEMENT_3D ( 'NONE', #31799, #35264, #38959 ) ;
#25750 = ORIENTED_EDGE ( 'NONE', *, *, #9336, .T. ) ;
#25749 = DIRECTION ( 'NONE',  ( -1.000000000000000000, -0.000000000000000000, -0.000000000000000000 ) ) ;
#25751 = CARTESIAN_POINT ( 'NONE',  ( 17.99999999999999645, -90.81729652456213842, 72.16798910853589177 ) ) ;
#25752 = FACE_BOUND ( 'NONE', #13198, .T. ) ;
#25753 = VECTOR ( 'NONE', #10976, 1000.000000000000000 ) ;
#25754 = VERTEX_POINT ( 'NONE', #26132 ) ;
#25755 = CARTESIAN_POINT ( 'NONE',  ( 10.12401712103624263, 40.00000000000000000, 76.79210772277129138 ) ) ;
#25756 = CARTESIAN_POINT ( 'NONE',  ( -147.8500000000000227, -5.254679414958916394E-13, 9.999999999999998224 ) ) ;
#25757 = ORIENTED_EDGE ( 'NONE', *, *, #11418, .T. ) ;
#25758 = DIRECTION ( 'NONE',  ( 1.000000000000000000, -3.469446951953616038E-17, 0.000000000000000000 ) ) ;
#25759 = EDGE_LOOP ( 'NONE', ( #5603, #22808, #39067, #1397 ) ) ;
#25760 = ORIENTED_EDGE ( 'NONE', *, *, #35616, .F. ) ;
#25761 = CARTESIAN_POINT ( 'NONE',  ( 17.99999999999999645, 63.24564713401792204, 102.5693868539697178 ) ) ;
#25763 = ORIENTED_EDGE ( 'NONE', *, *, #1091, .T. ) ;
#25762 = EDGE_CURVE ( 'NONE', #28377, #21277, #33631, .T. ) ;
#25764 = CARTESIAN_POINT ( 'NONE',  ( 0.000000000000000000, 0.000000000000000000, 0.000000000000000000 ) ) ;
#25765 = CARTESIAN_POINT ( 'NONE',  ( 17.99999999999999645, -10.40101730206288444, -120.0512800434972149 ) ) ;
#25766 = EDGE_CURVE ( 'NONE', #12374, #38848, #28091, .T. ) ;
#25767 = CARTESIAN_POINT ( 'NONE',  ( 17.99999999999999645, 31.94619804602764290, 16.59639811537368814 ) ) ;
#25768 = DIRECTION ( 'NONE',  ( 1.000000000000000000, 0.000000000000000000, 0.000000000000000000 ) ) ;
#25769 = ORIENTED_EDGE ( 'NONE', *, *, #34628, .T. ) ;
#25770 = CARTESIAN_POINT ( 'NONE',  ( 0.000000000000000000, -34.03046037009278280, 33.13733193845793323 ) ) ;
#25771 = VERTEX_POINT ( 'NONE', #18980 ) ;
#25772 = DIRECTION ( 'NONE',  ( 0.000000000000000000, 0.1253332335642974305, 0.9921147013144787641 ) ) ;
#25773 = EDGE_LOOP ( 'NONE', ( #18116, #12065 ) ) ;
#25774 = AXIS2_PLACEMENT_3D ( 'NONE', #16084, #39377, #29384 ) ;
#25775 = DIRECTION ( 'NONE',  ( 0.000000000000000000, 0.000000000000000000, 1.000000000000000000 ) ) ;
#25776 = FACE_OUTER_BOUND ( 'NONE', #18936, .T. ) ;
#25777 = AXIS2_PLACEMENT_3D ( 'NONE', #26846, #42741, #3250 ) ;
#25778 = CONTEXT_DEPENDENT_SHAPE_REPRESENTATION ( #515, #489 ) ;
#25779 = ADVANCED_FACE ( 'NONE', ( #39621, #42672 ), #12822, .F. ) ;
#25780 = DIRECTION ( 'NONE',  ( 0.000000000000000000, 0.3140767120219428166, 0.9493976084683832806 ) ) ;
#25781 = CARTESIAN_POINT ( 'NONE',  ( -48.53848235557606472, 31.00000000000000355, -37.22912483484027035 ) ) ;
#25782 = ORIENTED_EDGE ( 'NONE', *, *, #17212, .T. ) ;
#25783 = DIRECTION ( 'NONE',  ( 1.000000000000000000, 0.000000000000000000, 0.000000000000000000 ) ) ;
#25784 = ORIENTED_EDGE ( 'NONE', *, *, #32188, .F. ) ;
#25785 = CARTESIAN_POINT ( 'NONE',  ( -43.59452257625678584, 40.00000000000000000, -56.81327804312699925 ) ) ;
#25786 = ADVANCED_FACE ( 'NONE', ( #25927 ), #5410, .F. ) ;
#25787 = CARTESIAN_POINT ( 'NONE',  ( 0.000000000000000000, -59.47573314508669284, -99.59235496188668435 ) ) ;
#25788 = DIRECTION ( 'NONE',  ( 0.000000000000000000, 0.000000000000000000, 1.000000000000000000 ) ) ;
#25789 = EDGE_CURVE ( 'NONE', #34731, #1340, #16950, .T. ) ;
#25790 = DIRECTION ( 'NONE',  ( 1.000000000000000000, 1.836909530733573776E-16, 0.000000000000000000 ) ) ;
#25791 = CARTESIAN_POINT ( 'NONE',  ( 17.99999999999999645, -11.58753559615464290, -29.77419532459275331 ) ) ;
#25792 = ORIENTED_EDGE ( 'NONE', *, *, #34243, .T. ) ;
#25793 = CARTESIAN_POINT ( 'NONE',  ( 21.71086051706764763, 40.00000000000000000, -37.60982366119799991 ) ) ;
#25794 = DIRECTION ( 'NONE',  ( 1.000000000000000000, 0.000000000000000000, 0.000000000000000000 ) ) ;
#25796 = PLANE ( 'NONE',  #33323 ) ;
#25795 = AXIS2_PLACEMENT_3D ( 'NONE', #23512, #35903, #33072 ) ;
#25797 = AXIS2_PLACEMENT_3D ( 'NONE', #22854, #6427, #29373 ) ;
#25798 = ORIENTED_EDGE ( 'NONE', *, *, #18271, .T. ) ;
#25799 = CIRCLE ( 'NONE', #43163, 10.99999999999999645 ) ;
#25800 = ADVANCED_FACE ( 'NONE', ( #9542 ), #32234, .F. ) ;
#25801 = FACE_OUTER_BOUND ( 'NONE', #6688, .T. ) ;
#25802 = LINE ( 'NONE', #5492, #10332 ) ;
#25803 = ORIENTED_EDGE ( 'NONE', *, *, #39091, .T. ) ;
#25804 = DIRECTION ( 'NONE',  ( -1.000000000000000000, 0.000000000000000000, 0.000000000000000000 ) ) ;
#25805 = ORIENTED_EDGE ( 'NONE', *, *, #32834, .T. ) ;
#25806 = VERTEX_POINT ( 'NONE', #8899 ) ;
#25807 = FACE_OUTER_BOUND ( 'NONE', #14791, .T. ) ;
#25808 = EDGE_CURVE ( 'NONE', #4714, #39379, #22253, .T. ) ;
#25809 = CARTESIAN_POINT ( 'NONE',  ( 84.58694138809386232, 31.00000000000000000, 22.77597867319729374 ) ) ;
#25810 = ORIENTED_EDGE ( 'NONE', *, *, #16704, .F. ) ;
#25811 = CARTESIAN_POINT ( 'NONE',  ( 17.99999999999999645, 0.000000000000000000, 0.000000000000000000 ) ) ;
#25812 = EDGE_CURVE ( 'NONE', #6504, #16031, #6440, .T. ) ;
#25813 = EDGE_CURVE ( 'NONE', #42312, #27034, #1585, .T. ) ;
#25814 = EDGE_CURVE ( 'NONE', #25997, #13195, #42647, .T. ) ;
#25815 = FACE_OUTER_BOUND ( 'NONE', #41317, .T. ) ;
#25816 = ORIENTED_EDGE ( 'NONE', *, *, #36981, .F. ) ;
#25817 = CARTESIAN_POINT ( 'NONE',  ( 0.000000000000000000, 119.7318547011703629, -13.59315897125607009 ) ) ;
#25818 = DIRECTION ( 'NONE',  ( 0.000000000000000000, 0.3641605752528167539, 0.9313361774523405412 ) ) ;
#25819 = CARTESIAN_POINT ( 'NONE',  ( -135.4416936590755540, -2.055254544495720648, -102.7350398871816424 ) ) ;
#25821 = CARTESIAN_POINT ( 'NONE',  ( 0.000000000000000000, 0.000000000000000000, 0.000000000000000000 ) ) ;
#25820 = DIRECTION ( 'NONE',  ( -3.996523416598930318E-16, 2.658563593772947863E-15, 1.000000000000000000 ) ) ;
#25822 = CARTESIAN_POINT ( 'NONE',  ( -8.920000000000003482, 1.836970198721029589E-15, -14.99999999999999822 ) ) ;
#25823 = ORIENTED_EDGE ( 'NONE', *, *, #14774, .F. ) ;
#25824 = CARTESIAN_POINT ( 'NONE',  ( 1.799870782497353439, 31.00000000000000355, 27.39583333577991908 ) ) ;
#25825 = AXIS2_PLACEMENT_3D ( 'NONE', #8484, #2134, #17929 ) ;
#25826 = VERTEX_POINT ( 'NONE', #7319 ) ;
#25827 = CARTESIAN_POINT ( 'NONE',  ( 17.99999999999999645, -119.8996782608630838, 12.02323392193314966 ) ) ;
#25828 = AXIS2_PLACEMENT_3D ( 'NONE', #32218, #42229, #39171 ) ;
#25829 = DIRECTION ( 'NONE',  ( 1.000000000000000000, -0.000000000000000000, -0.000000000000000000 ) ) ;
#25830 = EDGE_LOOP ( 'NONE', ( #23609, #4567, #42760, #19496 ) ) ;
#25831 = CIRCLE ( 'NONE', #38353, 59.00000000000000711 ) ;
#25832 = CARTESIAN_POINT ( 'NONE',  ( 25.04716826810500763, 40.00000000000000000, 3.293035637142270655 ) ) ;
#25833 = CARTESIAN_POINT ( 'NONE',  ( -31.99444157863030114, 40.00000000000000000, -4.262017635501984536 ) ) ;
#25834 = EDGE_CURVE ( 'NONE', #27591, #9615, #12052, .T. ) ;
#25835 = ORIENTED_EDGE ( 'NONE', *, *, #26632, .T. ) ;
#25836 = ORIENTED_EDGE ( 'NONE', *, *, #662, .F. ) ;
#25837 = DIRECTION ( 'NONE',  ( 1.000000000000000000, 0.000000000000000000, 0.000000000000000000 ) ) ;
#25838 = LINE ( 'NONE', #25417, #13754 ) ;
#25839 = EDGE_CURVE ( 'NONE', #4984, #23276, #9930, .T. ) ;
#25840 = CARTESIAN_POINT ( 'NONE',  ( -102.9608013043458072, -34.05525454449571043, 14.45886780445738218 ) ) ;
#25841 = DIRECTION ( 'NONE',  ( 0.000000000000000000, -0.6783118362696222148, 0.7347741508630616369 ) ) ;
#25842 = CARTESIAN_POINT ( 'NONE',  ( 17.99999999999999645, 30.78424799127077804, -6.672111855472861563 ) ) ;
#25843 = DIRECTION ( 'NONE',  ( -1.000000000000000000, 0.000000000000000000, 0.000000000000000000 ) ) ;
#25844 = ORIENTED_EDGE ( 'NONE', *, *, #23485, .F. ) ;
#25845 = CARTESIAN_POINT ( 'NONE',  ( 17.99999999999999645, -11.65176648920959757, -115.4133282497343487 ) ) ;
#25846 = EDGE_LOOP ( 'NONE', ( #42581, #4692, #35380, #31209 ) ) ;
#25847 = DIRECTION ( 'NONE',  ( 0.000000000000000000, 0.000000000000000000, 1.000000000000000000 ) ) ;
#25848 = CARTESIAN_POINT ( 'NONE',  ( 18.00000000000000355, 0.000000000000000000, 0.000000000000000000 ) ) ;
#25849 = VECTOR ( 'NONE', #8308, 1000.000000000000000 ) ;
#25850 = DIRECTION ( 'NONE',  ( 0.000000000000000000, 0.000000000000000000, 1.000000000000000000 ) ) ;
#25851 = DIRECTION ( 'NONE',  ( -1.000000000000000000, 0.000000000000000000, -0.000000000000000000 ) ) ;
#25852 = ORIENTED_EDGE ( 'NONE', *, *, #33387, .F. ) ;
#25853 = CARTESIAN_POINT ( 'NONE',  ( 46.76839422406115432, 39.99999999999999289, -81.00140361174831583 ) ) ;
#25854 = EDGE_LOOP ( 'NONE', ( #32174, #546, #8696, #6466 ) ) ;
#25855 = CIRCLE ( 'NONE', #6999, 59.00000000000000000 ) ;
#25856 = CARTESIAN_POINT ( 'NONE',  ( 17.99999999999999645, 95.31344542257733110, 66.11616384574480776 ) ) ;
#25857 = CIRCLE ( 'NONE', #36965, 120.5010000000000332 ) ;
#25858 = ORIENTED_EDGE ( 'NONE', *, *, #18370, .F. ) ;
#25860 = ORIENTED_EDGE ( 'NONE', *, *, #27134, .F. ) ;
#25859 = DIRECTION ( 'NONE',  ( 1.000000000000000000, 0.000000000000000000, 0.000000000000000000 ) ) ;
#25861 = CIRCLE ( 'NONE', #1430, 120.5010000000000474 ) ;
#25862 = CARTESIAN_POINT ( 'NONE',  ( 44.54779904930365575, 31.00000000000000355, -34.05916983163054113 ) ) ;
#25864 = ORIENTED_EDGE ( 'NONE', *, *, #9150, .F. ) ;
#25863 = AXIS2_PLACEMENT_3D ( 'NONE', #24217, #14818, #27691 ) ;
#25865 = LINE ( 'NONE', #26062, #11243 ) ;
#25866 = EDGE_CURVE ( 'NONE', #20175, #416, #28804, .T. ) ;
#25867 = EDGE_CURVE ( 'NONE', #7485, #17487, #17413, .T. ) ;
#25868 = CIRCLE ( 'NONE', #35566, 36.00000000000000000 ) ;
#25869 = CARTESIAN_POINT ( 'NONE',  ( 0.000000000000000000, -27.24480646643618442, 15.80846360676574669 ) ) ;
#25870 = EDGE_CURVE ( 'NONE', #25754, #37125, #42001, .T. ) ;
#25871 = ORIENTED_EDGE ( 'NONE', *, *, #8356, .F. ) ;
#25872 = CARTESIAN_POINT ( 'NONE',  ( 22.12550800842195287, 40.00000000000000000, 65.48657384633656875 ) ) ;
#25874 = LINE ( 'NONE', #15615, #42959 ) ;
#25873 = CARTESIAN_POINT ( 'NONE',  ( 17.99999999999999645, -112.5220807139882311, -28.19186676675956704 ) ) ;
#25875 = CARTESIAN_POINT ( 'NONE',  ( 17.99999999999999645, 21.55123232222629426, -118.5581519187670096 ) ) ;
#25876 = ORIENTED_EDGE ( 'NONE', *, *, #18893, .F. ) ;
#25877 = DIRECTION ( 'NONE',  ( 0.000000000000000000, -0.1062934856473723849, 0.9943348002101364269 ) ) ;
#25878 = VERTEX_POINT ( 'NONE', #23945 ) ;
#25879 =( LENGTH_UNIT ( ) NAMED_UNIT ( * ) SI_UNIT ( .MILLI., .METRE. ) );
#25880 = DIRECTION ( 'NONE',  ( -1.000000000000000000, 0.000000000000000000, -0.000000000000000000 ) ) ;
#25881 = FACE_OUTER_BOUND ( 'NONE', #20602, .T. ) ;
#25882 = EDGE_CURVE ( 'NONE', #34092, #9576, #323, .T. ) ;
#25883 = CARTESIAN_POINT ( 'NONE',  ( 5.399612364985509672, 31.00000000000000355, -82.60416666586320389 ) ) ;
#25885 = CARTESIAN_POINT ( 'NONE',  ( -19.99999999999999645, 17.11489954122026447, 1.283214542831033755 ) ) ;
#25884 = FACE_OUTER_BOUND ( 'NONE', #22652, .T. ) ;
#25886 = ORIENTED_EDGE ( 'NONE', *, *, #174, .T. ) ;
#25887 = AXIS2_PLACEMENT_3D ( 'NONE', #16052, #29558, #5768 ) ;
#25888 = CARTESIAN_POINT ( 'NONE',  ( 17.99999999999999645, 111.7974656912331426, -9.465682155094398809 ) ) ;
#25889 = CIRCLE ( 'NONE', #7039, 1.999999999999988010 ) ;
#25890 = ORIENTED_EDGE ( 'NONE', *, *, #25443, .F. ) ;
#25891 = CARTESIAN_POINT ( 'NONE',  ( 6.599999999999997868, 20.00000000000000000, 0.000000000000000000 ) ) ;
#25892 = CARTESIAN_POINT ( 'NONE',  ( 17.99999999999999645, 119.0898412705476943, -18.38751498043618682 ) ) ;
#25893 = CARTESIAN_POINT ( 'NONE',  ( 6.386360208629405122, 31.00000000000000355, 99.40013590833048340 ) ) ;
#25894 = CARTESIAN_POINT ( 'NONE',  ( -41.44813913998980581, 40.00000000000000000, -84.33308812960441969 ) ) ;
#25895 = AXIS2_PLACEMENT_3D ( 'NONE', #13449, #29817, #10145 ) ;
#25896 = DIRECTION ( 'NONE',  ( -1.000000000000000000, 0.000000000000000000, 0.000000000000000000 ) ) ;
#25897 = ORIENTED_EDGE ( 'NONE', *, *, #30981, .F. ) ;
#25898 = DIRECTION ( 'NONE',  ( 0.000000000000000000, 0.000000000000000000, 1.000000000000000000 ) ) ;
#25899 = ORIENTED_EDGE ( 'NONE', *, *, #31288, .F. ) ;
#25900 = CIRCLE ( 'NONE', #9170, 142.5000000000000284 ) ;
#25901 = CARTESIAN_POINT ( 'NONE',  ( 17.99999999999999645, 73.78980555658606022, 95.26571049922013401 ) ) ;
#25902 = FACE_OUTER_BOUND ( 'NONE', #5148, .T. ) ;
#25903 = CARTESIAN_POINT ( 'NONE',  ( 17.99999999999999645, 63.55543939553766108, 97.03971415477347762 ) ) ;
#25904 = ORIENTED_EDGE ( 'NONE', *, *, #33799, .F. ) ;
#25905 = FACE_BOUND ( 'NONE', #36124, .T. ) ;
#25906 = DIRECTION ( 'NONE',  ( 1.000000000000000000, 0.000000000000000000, 0.000000000000000000 ) ) ;
#25907 = DIRECTION ( 'NONE',  ( -1.000000000000000000, 0.000000000000000000, 0.000000000000000000 ) ) ;
#25908 = EDGE_LOOP ( 'NONE', ( #41482, #5028, #34180, #23685 ) ) ;
#25909 = CARTESIAN_POINT ( 'NONE',  ( -22.10416666678001008, 31.00000000000000355, -1.441157586896874898 ) ) ;
#25910 = DIRECTION ( 'NONE',  ( 0.000000000000000000, -2.752035887312358229E-14, -1.000000000000000000 ) ) ;
#25911 = EDGE_CURVE ( 'NONE', #6283, #19076, #10399, .T. ) ;
#25913 = VERTEX_POINT ( 'NONE', #16972 ) ;
#25912 = DIRECTION ( 'NONE',  ( 0.000000000000000000, 0.000000000000000000, 1.000000000000000000 ) ) ;
#25914 = ORIENTED_EDGE ( 'NONE', *, *, #31037, .T. ) ;
#25915 = DIRECTION ( 'NONE',  ( -1.000000000000000000, -0.000000000000000000, -0.000000000000000000 ) ) ;
#25916 = DIRECTION ( 'NONE',  ( 1.000000000000000000, 0.000000000000000000, 0.000000000000000000 ) ) ;
#25917 = CARTESIAN_POINT ( 'NONE',  ( 45.06603723658675875, 40.00000000000000000, 15.38899812202754624 ) ) ;
#25918 = CARTESIAN_POINT ( 'NONE',  ( -3.996523416598931009E-15, 2.658563593772952281E-14, 10.00000000000000178 ) ) ;
#25919 = AXIS2_PLACEMENT_3D ( 'NONE', #8890, #28342, #1681 ) ;
#25920 = DIRECTION ( 'NONE',  ( 0.000000000000000000, 0.000000000000000000, 1.000000000000000000 ) ) ;
#25921 = AXIS2_PLACEMENT_3D ( 'NONE', #27840, #11250, #4446 ) ;
#25922 = DIRECTION ( 'NONE',  ( 1.000000000000000000, 1.836909530733573776E-16, 0.000000000000000000 ) ) ;
#25923 = ORIENTED_EDGE ( 'NONE', *, *, #27894, .T. ) ;
#25924 = DIRECTION ( 'NONE',  ( 1.000000000000000000, 0.000000000000000000, 0.000000000000000000 ) ) ;
#25925 = ADVANCED_FACE ( 'NONE', ( #20250 ), #30691, .T. ) ;
#25926 = EDGE_LOOP ( 'NONE', ( #9736, #39263, #3095, #27038 ) ) ;
#25927 = FACE_OUTER_BOUND ( 'NONE', #23861, .T. ) ;
#25928 = DIRECTION ( 'NONE',  ( 0.000000000000000000, 0.000000000000000000, 1.000000000000000000 ) ) ;
#25929 = EDGE_CURVE ( 'NONE', #37461, #17463, #20471, .T. ) ;
#25930 = CARTESIAN_POINT ( 'NONE',  ( 32.71557229150619861, 31.00000000000000355, -11.11602612089219910 ) ) ;
#25931 = VERTEX_POINT ( 'NONE', #7111 ) ;
#25932 = PRODUCT_DEFINITION_SHAPE ( 'NONE', 'NONE',  #43206 ) ;
#25933 = DIRECTION ( 'NONE',  ( 0.000000000000000000, 0.9996456111234524045, 0.02662052143777824190 ) ) ;
#25934 = CARTESIAN_POINT ( 'NONE',  ( 11.43299787627070607, 31.00000000000000355, 86.72764684403134083 ) ) ;
#25935 = LINE ( 'NONE', #39195, #3130 ) ;
#25936 = EDGE_LOOP ( 'NONE', ( #41419, #153, #2541, #21631 ) ) ;
#25937 = CARTESIAN_POINT ( 'NONE',  ( 51.26988013555838819, 31.00000000000000355, 45.10883117380814866 ) ) ;
#25938 = CARTESIAN_POINT ( 'NONE',  ( -56.48168293059611500, 40.00000000000000711, 43.19841958066528065 ) ) ;
#25939 = CARTESIAN_POINT ( 'NONE',  ( 94.59594211465898184, 39.99999999999999289, 12.45590092308117569 ) ) ;
#25940 = EDGE_LOOP ( 'NONE', ( #4811, #37699, #39127, #24092 ) ) ;
#25942 = EDGE_CURVE ( 'NONE', #18762, #25931, #16255, .T. ) ;
#25941 = AXIS2_PLACEMENT_3D ( 'NONE', #32965, #36016, #18862 ) ;
#25943 = CIRCLE ( 'NONE', #12699, 19.19999999999999574 ) ;
#25944 = DIRECTION ( 'NONE',  ( -1.000000000000000000, -0.000000000000000000, -0.000000000000000000 ) ) ;
#25945 = LINE ( 'NONE', #26373, #28950 ) ;
#25946 = AXIS2_PLACEMENT_3D ( 'NONE', #26851, #23610, #40125 ) ;
#25948 = ORIENTED_EDGE ( 'NONE', *, *, #41784, .F. ) ;
#25947 = CARTESIAN_POINT ( 'NONE',  ( 0.000000000000000000, -13.56094713063537327, -50.20060470671754871 ) ) ;
#25949 = DIRECTION ( 'NONE',  ( 1.000000000000000000, -0.000000000000000000, 0.000000000000000000 ) ) ;
#25950 = DIRECTION ( 'NONE',  ( 0.000000000000000000, 0.000000000000000000, 1.000000000000000000 ) ) ;
#25951 = VERTEX_POINT ( 'NONE', #26555 ) ;
#25952 = CARTESIAN_POINT ( 'NONE',  ( 58.80104710710317306, 39.99999999999999289, -45.11949705600698479 ) ) ;
#25953 = FACE_OUTER_BOUND ( 'NONE', #42876, .T. ) ;
#25954 = EDGE_LOOP ( 'NONE', ( #21147, #31997, #28854, #530 ) ) ;
#25955 = CARTESIAN_POINT ( 'NONE',  ( -6.075999999999997847, 0.000000000000000000, 0.000000000000000000 ) ) ;
#25956 = DIRECTION ( 'NONE',  ( -1.000000000000000000, 0.000000000000000000, -0.000000000000000000 ) ) ;
#25957 = ORIENTED_EDGE ( 'NONE', *, *, #5542, .F. ) ;
#25958 = EDGE_CURVE ( 'NONE', #36617, #20671, #3670, .T. ) ;
#25959 = ORIENTED_EDGE ( 'NONE', *, *, #26195, .T. ) ;
#25960 = CYLINDRICAL_SURFACE ( 'NONE', #37917, 59.00000000000000000 ) ;
#25961 = VERTEX_POINT ( 'NONE', #9952 ) ;
#25962 = DIRECTION ( 'NONE',  ( 0.000000000000000000, 0.000000000000000000, -1.000000000000000000 ) ) ;
#25963 = DIRECTION ( 'NONE',  ( -1.000000000000000000, 0.000000000000000000, 0.000000000000000000 ) ) ;
#25964 = CARTESIAN_POINT ( 'NONE',  ( 0.000000000000000000, -103.1672962317654338, 44.09967643725834563 ) ) ;
#25965 = ORIENTED_EDGE ( 'NONE', *, *, #41422, .T. ) ;
#25966 = DIRECTION ( 'NONE',  ( 1.000000000000000000, 0.000000000000000000, 0.000000000000000000 ) ) ;
#25967 = ADVANCED_FACE ( 'NONE', ( #20044 ), #14124, .F. ) ;
#25968 = VERTEX_POINT ( 'NONE', #3168 ) ;
#25969 = VECTOR ( 'NONE', #30312, 1000.000000000000000 ) ;
#25970 = CIRCLE ( 'NONE', #31541, 20.00000000000001066 ) ;
#25971 = DIRECTION ( 'NONE',  ( 1.000000000000000000, -0.000000000000000000, 0.000000000000000000 ) ) ;
#25972 = ADVANCED_FACE ( 'NONE', ( #36554 ), #6895, .T. ) ;
#25973 = ORIENTED_EDGE ( 'NONE', *, *, #30631, .F. ) ;
#25974 = DIRECTION ( 'NONE',  ( 1.000000000000000000, 0.000000000000000000, -0.000000000000000000 ) ) ;
#25975 = CIRCLE ( 'NONE', #36403, 2.649999999999985700 ) ;
#25976 = EDGE_CURVE ( 'NONE', #9503, #22001, #39219, .T. ) ;
#25977 = CYLINDRICAL_SURFACE ( 'NONE', #6284, 31.49899999999999878 ) ;
#25978 = ITEM_DEFINED_TRANSFORMATION ( 'NONE', 'NONE', #19143,  #13552 ) ;
#25979 = DIRECTION ( 'NONE',  ( 0.000000000000000000, 0.000000000000000000, -1.000000000000000000 ) ) ;
#25980 = CARTESIAN_POINT ( 'NONE',  ( 50.09382087749727930, 31.00000000000000355, 24.69014870349942825 ) ) ;
#25981 = VECTOR ( 'NONE', #7436, 1000.000000000000000 ) ;
#25982 = DIRECTION ( 'NONE',  ( -1.000000000000000000, 0.000000000000000000, 0.000000000000000000 ) ) ;
#25983 = ORIENTED_EDGE ( 'NONE', *, *, #9764, .T. ) ;
#25984 = CARTESIAN_POINT ( 'NONE',  ( -22.00208165626505519, 31.00000000000000355, -25.16137218361809502 ) ) ;
#25985 = CARTESIAN_POINT ( 'NONE',  ( 33.41571365387085280, 40.00000000000000000, 57.85165222247763239 ) ) ;
#25986 = EDGE_CURVE ( 'NONE', #35289, #5690, #9279, .T. ) ;
#25987 = DIRECTION ( 'NONE',  ( 1.000000000000000000, 0.000000000000000000, 0.000000000000000000 ) ) ;
#25988 = LINE ( 'NONE', #39247, #40239 ) ;
#25989 = EDGE_CURVE ( 'NONE', #1619, #10863, #33662, .T. ) ;
#25990 = CARTESIAN_POINT ( 'NONE',  ( 17.99999999999999645, -110.0562500189195561, -49.07252625220223052 ) ) ;
#25991 = DIRECTION ( 'NONE',  ( -1.000000000000000000, 0.000000000000000000, -0.000000000000000000 ) ) ;
#25992 = AXIS2_PLACEMENT_3D ( 'NONE', #19182, #32447, #2535 ) ;
#25993 = EDGE_LOOP ( 'NONE', ( #5071, #19581, #22581, #21098 ) ) ;
#25994 = CARTESIAN_POINT ( 'NONE',  ( -13.53264355869793967, 40.00000000000000000, -39.83251807627727459 ) ) ;
#25995 = DIRECTION ( 'NONE',  ( -1.000000000000000000, -0.000000000000000000, -0.000000000000000000 ) ) ;
#25996 = CARTESIAN_POINT ( 'NONE',  ( 9.000000000000001776, -47.32430374665916162, -21.55018039121577544 ) ) ;
#25997 = VERTEX_POINT ( 'NONE', #41782 ) ;
#25998 = DIRECTION ( 'NONE',  ( 0.000000000000000000, 0.000000000000000000, 1.000000000000000000 ) ) ;
#25999 = DIRECTION ( 'NONE',  ( -1.000000000000000000, -0.000000000000000000, 0.000000000000000000 ) ) ;
#26000 = VERTEX_POINT ( 'NONE', #7550 ) ;
#26001 = CARTESIAN_POINT ( 'NONE',  ( 0.000000000000000000, 31.81777574834305966, -2.898764365605425830 ) ) ;
#26002 = VERTEX_POINT ( 'NONE', #17632 ) ;
#26003 = ORIENTED_EDGE ( 'NONE', *, *, #11236, .F. ) ;
#26004 = CARTESIAN_POINT ( 'NONE',  ( 18.00000000000000355, 18.53613841426788866, 48.58406706613909876 ) ) ;
#26005 = CARTESIAN_POINT ( 'NONE',  ( -79.74759331938361129, 31.00000000000000711, -21.47736420602193519 ) ) ;
#26006 = VERTEX_POINT ( 'NONE', #4259 ) ;
#26007 = DIRECTION ( 'NONE',  ( 0.000000000000000000, 0.6382441836448161654, 0.7698339834299096074 ) ) ;
#26008 = DIRECTION ( 'NONE',  ( 0.000000000000000000, 0.000000000000000000, 1.000000000000000000 ) ) ;
#26009 = DIRECTION ( 'NONE',  ( -1.000000000000000000, 0.000000000000000000, 0.000000000000000000 ) ) ;
#26010 = ORIENTED_EDGE ( 'NONE', *, *, #22592, .F. ) ;
#26011 = CYLINDRICAL_SURFACE ( 'NONE', #28691, 120.5010000000000190 ) ;
#26012 = ADVANCED_FACE ( 'NONE', ( #27643 ), #24653, .T. ) ;
#26013 = CARTESIAN_POINT ( 'NONE',  ( 17.99999999999999645, 27.83061035787113369, -117.2431154827794586 ) ) ;
#26014 = CARTESIAN_POINT ( 'NONE',  ( 17.99999999999999645, -114.1529630473446986, -38.59523323561551678 ) ) ;
#26015 = EDGE_CURVE ( 'NONE', #33247, #37148, #27394, .T. ) ;
#26017 = CARTESIAN_POINT ( 'NONE',  ( 9.000000000000000000, -34.78944633786284868, 9.257128253673498008 ) ) ;
#26016 = CARTESIAN_POINT ( 'NONE',  ( 0.000000000000000000, 0.6168405712491942250, -35.99471499692226217 ) ) ;
#26018 = CARTESIAN_POINT ( 'NONE',  ( 22.90854556226710415, -35.35525454449573601, -74.83297477053821467 ) ) ;
#26019 = ORIENTED_EDGE ( 'NONE', *, *, #25882, .F. ) ;
#26020 = CARTESIAN_POINT ( 'NONE',  ( 8.917417253944853073, 33.05525454449572464, -2.424151526724388273 ) ) ;
#26021 = AXIS2_PLACEMENT_3D ( 'NONE', #14775, #34816, #4923 ) ;
#26022 = CARTESIAN_POINT ( 'NONE',  ( 14.71924655979513297, 31.00000000000000355, -29.87007926703815741 ) ) ;
#26023 = ORIENTED_EDGE ( 'NONE', *, *, #17667, .T. ) ;
#26024 = DIRECTION ( 'NONE',  ( 1.000000000000000000, -1.373900992973641868E-15, -6.546126324440886161E-16 ) ) ;
#26025 = LINE ( 'NONE', #2219, #5135 ) ;
#26026 = ORIENTED_EDGE ( 'NONE', *, *, #7651, .F. ) ;
#26027 = DIRECTION ( 'NONE',  ( -1.000000000000000000, 0.000000000000000000, 0.000000000000000000 ) ) ;
#26028 = CARTESIAN_POINT ( 'NONE',  ( -25.29482881991252086, 40.00000000000000000, -32.96004927633274662 ) ) ;
#26029 = STYLED_ITEM ( 'NONE', ( #31121 ), #31788 ) ;
#26030 = CARTESIAN_POINT ( 'NONE',  ( 35.42814233786123879, 40.00000000000000000, -9.427541829740359702 ) ) ;
#26031 = AXIS2_PLACEMENT_3D ( 'NONE', #43117, #23735, #33521 ) ;
#26032 = VERTEX_POINT ( 'NONE', #20910 ) ;
#26033 = EDGE_CURVE ( 'NONE', #22307, #3223, #5788, .T. ) ;
#26034 = EDGE_LOOP ( 'NONE', ( #17582, #26782 ) ) ;
#26035 = DIRECTION ( 'NONE',  ( -1.000000000000000000, 0.000000000000000000, 0.000000000000000000 ) ) ;
#26036 = ADVANCED_FACE ( 'NONE', ( #38297 ), #31123, .F. ) ;
#26037 = ADVANCED_FACE ( 'NONE', ( #31765 ), #37640, .T. ) ;
#26038 = EDGE_CURVE ( 'NONE', #4027, #25070, #884, .T. ) ;
#26039 = CARTESIAN_POINT ( 'NONE',  ( 0.000000000000000000, 0.000000000000000000, 0.000000000000000000 ) ) ;
#26040 = VECTOR ( 'NONE', #14649, 1000.000000000000000 ) ;
#26041 = LINE ( 'NONE', #2657, #32890 ) ;
#26042 = CARTESIAN_POINT ( 'NONE',  ( 8.999999999999998224, 18.42432724429518487, -30.92804820215982531 ) ) ;
#26043 = ORIENTED_EDGE ( 'NONE', *, *, #30853, .F. ) ;
#26044 = CARTESIAN_POINT ( 'NONE',  ( 0.000000000000000000, -37.91532898920899441, -28.61088654061679648 ) ) ;
#26045 = ORIENTED_EDGE ( 'NONE', *, *, #19876, .F. ) ;
#26046 = CARTESIAN_POINT ( 'NONE',  ( -105.9879088449591933, 40.00000000000000000, -0.3807199291576673361 ) ) ;
#26047 = CARTESIAN_POINT ( 'NONE',  ( 0.000000000000000000, 0.000000000000000000, 0.000000000000000000 ) ) ;
#26048 = AXIS2_PLACEMENT_3D ( 'NONE', #25408, #2853, #28877 ) ;
#26049 = FACE_BOUND ( 'NONE', #29635, .T. ) ;
#26050 = CIRCLE ( 'NONE', #23265, 13.60000000000000142 ) ;
#26051 = CARTESIAN_POINT ( 'NONE',  ( 17.99999999999999645, -54.09091620264652533, -102.6166301549523467 ) ) ;
#26052 = VERTEX_POINT ( 'NONE', #25051 ) ;
#26053 = CARTESIAN_POINT ( 'NONE',  ( 17.99999999999999645, -31.81777574834303124, -2.898764365605651427 ) ) ;
#26054 = VERTEX_POINT ( 'NONE', #37431 ) ;
#26055 = CARTESIAN_POINT ( 'NONE',  ( 17.99999999999999645, 110.1579703617969130, -21.29539948940136540 ) ) ;
#26056 = CIRCLE ( 'NONE', #33689, 19.59999999999999432 ) ;
#26057 = ORIENTED_EDGE ( 'NONE', *, *, #36159, .F. ) ;
#26059 = EDGE_LOOP ( 'NONE', ( #38816, #22881, #33602, #33900 ) ) ;
#26058 = DIRECTION ( 'NONE',  ( -1.000000000000000000, 0.000000000000000000, 0.000000000000000000 ) ) ;
#26060 = CARTESIAN_POINT ( 'NONE',  ( 14.32751628686350287, 31.00000000000000355, -53.13354968560084757 ) ) ;
#26061 = ORIENTED_EDGE ( 'NONE', *, *, #7862, .F. ) ;
#26062 = CARTESIAN_POINT ( 'NONE',  ( 17.99999999999999645, 9.484061862023926537, 30.03730300138984433 ) ) ;
#26063 =( GEOMETRIC_REPRESENTATION_CONTEXT ( 3 ) GLOBAL_UNCERTAINTY_ASSIGNED_CONTEXT ( ( #13904 ) ) GLOBAL_UNIT_ASSIGNED_CONTEXT ( ( #34536, #27585, #14723 ) ) REPRESENTATION_CONTEXT ( 'NONE', 'WORKASPACE' ) );
#26064 = ORIENTED_EDGE ( 'NONE', *, *, #33751, .T. ) ;
#26065 = DIRECTION ( 'NONE',  ( -1.000000000000000000, 0.000000000000000000, 0.000000000000000000 ) ) ;
#26066 = EDGE_CURVE ( 'NONE', #36553, #7888, #36415, .T. ) ;
#26067 = ORIENTED_EDGE ( 'NONE', *, *, #27930, .F. ) ;
#26068 = CARTESIAN_POINT ( 'NONE',  ( -68.78002826189113250, 40.00000000000000711, -23.46745878763887916 ) ) ;
#26069 = EDGE_CURVE ( 'NONE', #29131, #12550, #8206, .T. ) ;
#26071 = DIRECTION ( 'NONE',  ( 0.000000000000000000, 0.000000000000000000, 1.000000000000000000 ) ) ;
#26070 = DIRECTION ( 'NONE',  ( -1.000000000000000000, 0.000000000000000000, -0.000000000000000000 ) ) ;
#26072 = CARTESIAN_POINT ( 'NONE',  ( 0.000000000000000000, 0.000000000000000000, 0.000000000000000000 ) ) ;
#26073 = ORIENTED_EDGE ( 'NONE', *, *, #7843, .T. ) ;
#26074 = DIRECTION ( 'NONE',  ( -3.009274222672345096E-17, -1.000000000000000000, 2.455023325076454960E-18 ) ) ;
#26075 = AXIS2_PLACEMENT_3D ( 'NONE', #21863, #35328, #12019 ) ;
#26076 = ORIENTED_EDGE ( 'NONE', *, *, #8555, .F. ) ;
#26077 =( NAMED_UNIT ( * ) SI_UNIT ( $, .STERADIAN. ) SOLID_ANGLE_UNIT ( ) );
#26078 = DIRECTION ( 'NONE',  ( -1.000000000000000000, -0.000000000000000000, -0.000000000000000000 ) ) ;
#26079 = CIRCLE ( 'NONE', #2364, 36.00000000000000000 ) ;
#26080 = FACE_OUTER_BOUND ( 'NONE', #8539, .T. ) ;
#26081 = CARTESIAN_POINT ( 'NONE',  ( 74.30822294231431613, 31.00000000000000000, -9.796771932235298408 ) ) ;
#26083 = CARTESIAN_POINT ( 'NONE',  ( 0.000000000000000000, -92.10690493017105496, 64.06707842432145128 ) ) ;
#26082 = CARTESIAN_POINT ( 'NONE',  ( 17.99999999999999645, 93.26762629039527042, -76.29967815892260319 ) ) ;
#26084 = EDGE_LOOP ( 'NONE', ( #24143, #35162, #35286, #35030 ) ) ;
#26085 = AXIS2_PLACEMENT_3D ( 'NONE', #19452, #33147, #25780 ) ;
#26086 = DIRECTION ( 'NONE',  ( -1.836909530733573776E-16, 1.000000000000000000, 0.000000000000000000 ) ) ;
#26087 = AXIS2_PLACEMENT_3D ( 'NONE', #35316, #32687, #2765 ) ;
#26088 = EDGE_CURVE ( 'NONE', #26682, #16913, #17681, .T. ) ;
#26089 = ORIENTED_EDGE ( 'NONE', *, *, #37709, .F. ) ;
#26090 = DIRECTION ( 'NONE',  ( -1.000000000000000000, 0.000000000000000000, 0.000000000000000000 ) ) ;
#26091 = LINE ( 'NONE', #38729, #20682 ) ;
#26092 = EDGE_CURVE ( 'NONE', #25238, #5363, #1616, .T. ) ;
#26093 = CARTESIAN_POINT ( 'NONE',  ( 96.17895579821514218, 31.00000000000000000, -12.55124642863780515 ) ) ;
#26094 = CARTESIAN_POINT ( 'NONE',  ( -61.59955500558135100, 40.00000000000000711, -70.40623950603891501 ) ) ;
#26095 = EDGE_CURVE ( 'NONE', #2698, #16742, #4375, .T. ) ;
#26096 = EDGE_CURVE ( 'NONE', #40017, #27215, #34354, .T. ) ;
#26097 = DIRECTION ( 'NONE',  ( 0.000000000000000000, 0.000000000000000000, 1.000000000000000000 ) ) ;
#26098 = PRODUCT_DEFINITION_FORMATION_WITH_SPECIFIED_SOURCE ( 'ANY', '', #26283, .NOT_KNOWN. ) ;
#26099 = EDGE_CURVE ( 'NONE', #18966, #37469, #39900, .T. ) ;
#26100 = CARTESIAN_POINT ( 'NONE',  ( 18.00000000000000355, 46.87740477351718482, -3.172455868805370560 ) ) ;
#26101 = ORIENTED_EDGE ( 'NONE', *, *, #1133, .T. ) ;
#26102 = DIRECTION ( 'NONE',  ( 0.000000000000000000, 0.000000000000000000, 1.000000000000000000 ) ) ;
#26103 = ORIENTED_EDGE ( 'NONE', *, *, #12910, .F. ) ;
#26104 = AXIS2_PLACEMENT_3D ( 'NONE', #3641, #13732, #34407 ) ;
#26105 = LINE ( 'NONE', #33279, #17960 ) ;
#26106 = DIRECTION ( 'NONE',  ( 1.000000000000000000, 0.000000000000000000, 0.000000000000000000 ) ) ;
#26107 = DIRECTION ( 'NONE',  ( 0.000000000000000000, 0.000000000000000000, -1.000000000000000000 ) ) ;
#26108 = ORIENTED_EDGE ( 'NONE', *, *, #5297, .T. ) ;
#26109 = CARTESIAN_POINT ( 'NONE',  ( 22.90854556226710415, -34.05525454449573175, -74.83297477053821467 ) ) ;
#26110 = CIRCLE ( 'NONE', #18481, 52.00000000000000000 ) ;
#26111 = LINE ( 'NONE', #42867, #26981 ) ;
#26112 = FACE_OUTER_BOUND ( 'NONE', #33223, .T. ) ;
#26114 = ORIENTED_EDGE ( 'NONE', *, *, #33421, .T. ) ;
#26113 = DIRECTION ( 'NONE',  ( 1.000000000000000000, 0.000000000000000000, 0.000000000000000000 ) ) ;
#26115 = CARTESIAN_POINT ( 'NONE',  ( -19.81637295874435978, 31.00000000000000355, -11.44243563873997793 ) ) ;
#26116 = DIRECTION ( 'NONE',  ( -1.000000000000000000, -0.000000000000000000, -0.000000000000000000 ) ) ;
#26117 = AXIS2_PLACEMENT_3D ( 'NONE', #42899, #33089, #25933 ) ;
#26119 = ORIENTED_EDGE ( 'NONE', *, *, #9450, .T. ) ;
#26118 = CARTESIAN_POINT ( 'NONE',  ( 17.99999999999999645, 110.1579703617966430, 21.29539948940285043 ) ) ;
#26120 = CIRCLE ( 'NONE', #21975, 120.5010000000000332 ) ;
#26121 = ORIENTED_EDGE ( 'NONE', *, *, #29652, .F. ) ;
#26122 = CARTESIAN_POINT ( 'NONE',  ( 17.99999999999999645, -105.7179949885870514, 37.57629584241652054 ) ) ;
#26123 = DIRECTION ( 'NONE',  ( -1.000000000000000000, 0.000000000000000000, -0.000000000000000000 ) ) ;
#26124 = CARTESIAN_POINT ( 'NONE',  ( 17.12248163736668261, 40.00000000000000000, 34.87662400048956357 ) ) ;
#26125 = LINE ( 'NONE', #39390, #14650 ) ;
#26126 = CARTESIAN_POINT ( 'NONE',  ( 17.99999999999999645, 0.000000000000000000, 0.000000000000000000 ) ) ;
#26127 = CARTESIAN_POINT ( 'NONE',  ( 0.000000000000000000, -49.65209126885774538, 15.44894276735533190 ) ) ;
#26128 = ORIENTED_EDGE ( 'NONE', *, *, #6662, .F. ) ;
#26129 = DIRECTION ( 'NONE',  ( 1.000000000000000000, 0.000000000000000000, 0.000000000000000000 ) ) ;
#26130 = CIRCLE ( 'NONE', #17082, 36.00000000000000000 ) ;
#26131 = EDGE_LOOP ( 'NONE', ( #31485, #3142, #32721, #21869 ) ) ;
#26132 = CARTESIAN_POINT ( 'NONE',  ( 17.99999999999999645, -37.07968990261553444, 109.9140418541956308 ) ) ;
#26133 = DIRECTION ( 'NONE',  ( -1.000000000000000000, 0.000000000000000000, -0.000000000000000000 ) ) ;
#26134 = CARTESIAN_POINT ( 'NONE',  ( 44.50160557815096496, 31.00000000000000355, -5.869829666507492050 ) ) ;
#26135 = ORIENTED_EDGE ( 'NONE', *, *, #28767, .F. ) ;
#26136 = AXIS2_PLACEMENT_3D ( 'NONE', #35586, #15561, #5707 ) ;
#26137 = CARTESIAN_POINT ( 'NONE',  ( 17.99999999999999645, -8.827181066045094227, -120.1772519049560231 ) ) ;
#26138 = CARTESIAN_POINT ( 'NONE',  ( -28.35539204363714205, 31.00000000000000355, 83.52787551312086123 ) ) ;
#26139 = CIRCLE ( 'NONE', #12901, 47.49900000000000944 ) ;
#26140 = CARTESIAN_POINT ( 'NONE',  ( 42.80287614962790599, -14.05525454449571932, 69.29271901957253021 ) ) ;
#26141 = VERTEX_POINT ( 'NONE', #11270 ) ;
#26142 = CARTESIAN_POINT ( 'NONE',  ( -61.89998375878432313, 31.00000000000000711, 3.952486745199417673 ) ) ;
#26143 = CARTESIAN_POINT ( 'NONE',  ( -54.47698434027259395, 40.00000000000000000, -31.57393205620729404 ) ) ;
#26144 = EDGE_CURVE ( 'NONE', #28359, #17574, #18076, .T. ) ;
#26145 = ADVANCED_FACE ( 'NONE', ( #37853 ), #7977, .F. ) ;
#26146 = CARTESIAN_POINT ( 'NONE',  ( -94.39576909109665337, 40.00000000000000711, 32.06004391471374504 ) ) ;
#26147 = EDGE_CURVE ( 'NONE', #38781, #3798, #11391, .T. ) ;
#26148 = VECTOR ( 'NONE', #26960, 1000.000000000000000 ) ;
#26149 = ORIENTED_EDGE ( 'NONE', *, *, #30930, .F. ) ;
#26150 = CARTESIAN_POINT ( 'NONE',  ( -2.742827927723112236, -3.035229711105190464, -3.433252694550595230 ) ) ;
#26151 = CYLINDRICAL_SURFACE ( 'NONE', #29164, 59.00000000000000000 ) ;
#26152 = DIRECTION ( 'NONE',  ( -1.000000000000000000, -0.000000000000000000, -0.000000000000000000 ) ) ;
#26154 = VERTEX_POINT ( 'NONE', #14992 ) ;
#26153 = CARTESIAN_POINT ( 'NONE',  ( 8.999999999999998224, 68.63002662989875091, -93.51962064069435598 ) ) ;
#26155 = CARTESIAN_POINT ( 'NONE',  ( 17.99999999999999645, 92.25992191227393846, 77.51514567967427638 ) ) ;
#26156 = FACE_BOUND ( 'NONE', #33006, .T. ) ;
#26157 = EDGE_CURVE ( 'NONE', #41075, #5519, #23952, .T. ) ;
#26158 = CARTESIAN_POINT ( 'NONE',  ( 60.46509673945340779, 39.99999999999999289, 46.37897171328766888 ) ) ;
#26159 = DIRECTION ( 'NONE',  ( -3.996523416598930318E-16, 2.658563593772947863E-15, 1.000000000000000000 ) ) ;
#26160 = VECTOR ( 'NONE', #11877, 1000.000000000000000 ) ;
#26161 = ORIENTED_EDGE ( 'NONE', *, *, #37278, .T. ) ;
#26162 = DIRECTION ( 'NONE',  ( 0.000000000000000000, 0.000000000000000000, 1.000000000000000000 ) ) ;
#26163 = DIRECTION ( 'NONE',  ( 0.000000000000000000, 0.000000000000000000, 1.000000000000000000 ) ) ;
#26164 = AXIS2_PLACEMENT_3D ( 'NONE', #18279, #4704, #5352 ) ;
#26165 = ORIENTED_EDGE ( 'NONE', *, *, #18536, .F. ) ;
#26166 = CIRCLE ( 'NONE', #7328, 47.49900000000000233 ) ;
#26167 = VECTOR ( 'NONE', #11587, 1000.000000000000000 ) ;
#26168 = AXIS2_PLACEMENT_3D ( 'NONE', #25166, #38208, #21889 ) ;
#26169 = VERTEX_POINT ( 'NONE', #29356 ) ;
#26170 = DIRECTION ( 'NONE',  ( 0.000000000000000000, 0.000000000000000000, 1.000000000000000000 ) ) ;
#26171 = ORIENTED_EDGE ( 'NONE', *, *, #22559, .F. ) ;
#26172 = AXIS2_PLACEMENT_3D ( 'NONE', #13713, #10419, #7131 ) ;
#26173 = CARTESIAN_POINT ( 'NONE',  ( 33.90854556226734218, -40.05525454449572464, -74.83297477053821467 ) ) ;
#26174 = LINE ( 'NONE', #22710, #29050 ) ;
#26175 = VECTOR ( 'NONE', #7071, 1000.000000000000114 ) ;
#26176 = CARTESIAN_POINT ( 'NONE',  ( 0.000000000000000000, 0.000000000000000000, 0.000000000000000000 ) ) ;
#26177 = DIRECTION ( 'NONE',  ( 0.000000000000000000, 0.05322217484217219019, 0.9985826956767622775 ) ) ;
#26178 = VERTEX_POINT ( 'NONE', #38500 ) ;
#26179 = DIRECTION ( 'NONE',  ( -1.000000000000000000, 0.000000000000000000, 0.000000000000000000 ) ) ;
#26181 = VERTEX_POINT ( 'NONE', #18725 ) ;
#26180 = AXIS2_PLACEMENT_3D ( 'NONE', #1179, #25851, #21749 ) ;
#26182 = CYLINDRICAL_SURFACE ( 'NONE', #3618, 120.5010000000000190 ) ;
#26183 = ORIENTED_EDGE ( 'NONE', *, *, #9795, .T. ) ;
#26184 = CARTESIAN_POINT ( 'NONE',  ( 0.000000000000000000, 35.11945359308163006, -38.34871548465977753 ) ) ;
#26185 = CARTESIAN_POINT ( 'NONE',  ( 0.000000000000000000, 79.18387647320761857, 84.76976882518788159 ) ) ;
#26186 = DIRECTION ( 'NONE',  ( -1.000000000000000000, 0.000000000000000000, 0.000000000000000000 ) ) ;
#26187 = CARTESIAN_POINT ( 'NONE',  ( -15.01009539198478748, 31.00000000000000355, 56.06562763604418365 ) ) ;
#26188 = LINE ( 'NONE', #35750, #28974 ) ;
#26190 = ORIENTED_EDGE ( 'NONE', *, *, #19807, .T. ) ;
#26189 = AXIS2_PLACEMENT_3D ( 'NONE', #18668, #15157, #4645 ) ;
#26191 = CARTESIAN_POINT ( 'NONE',  ( -14.91913624998189469, 31.00000000000000355, -30.37684071746364012 ) ) ;
#26192 = EDGE_CURVE ( 'NONE', #39703, #29060, #5111, .T. ) ;
#26193 = CARTESIAN_POINT ( 'NONE',  ( 70.67261647610648367, 39.99999999999999289, -24.00465245562410743 ) ) ;
#26194 = AXIS2_PLACEMENT_3D ( 'NONE', #39227, #9354, #33133 ) ;
#26195 = EDGE_CURVE ( 'NONE', #29429, #22119, #23921, .T. ) ;
#26196 = VECTOR ( 'NONE', #37224, 1000.000000000000000 ) ;
#26197 = CARTESIAN_POINT ( 'NONE',  ( 17.99999999999999645, -5.919241748379376666, -31.39643714728462953 ) ) ;
#26198 = CARTESIAN_POINT ( 'NONE',  ( 0.000000000000000000, 0.6505223195683064175, 51.99593080916758225 ) ) ;
#26199 = AXIS2_PLACEMENT_3D ( 'NONE', #8801, #38898, #23593 ) ;
#26200 = CIRCLE ( 'NONE', #21358, 15.00000000000000000 ) ;
#26201 = DIRECTION ( 'NONE',  ( -1.000000000000000000, -0.000000000000000000, 0.000000000000000000 ) ) ;
#26202 = DIRECTION ( 'NONE',  ( -0.000000000000000000, -0.000000000000000000, 1.000000000000000000 ) ) ;
#26203 = EDGE_CURVE ( 'NONE', #6169, #3495, #29474, .T. ) ;
#26204 = CIRCLE ( 'NONE', #31787, 52.00000000000000000 ) ;
#26205 = VERTEX_POINT ( 'NONE', #9053 ) ;
#26206 = CARTESIAN_POINT ( 'NONE',  ( 44.50160557815096496, 40.00000000000000000, -5.869829666507492050 ) ) ;
#26207 = DIRECTION ( 'NONE',  ( -1.000000000000000000, -0.000000000000000000, -0.000000000000000000 ) ) ;
#26208 = CARTESIAN_POINT ( 'NONE',  ( 104.9999999999993321, -2.293336392629658115E-13, -32.00000000000000000 ) ) ;
#26209 = EDGE_LOOP ( 'NONE', ( #14554, #3088, #20088, #22252 ) ) ;
#26210 = EDGE_CURVE ( 'NONE', #28231, #36745, #25361, .T. ) ;
#26211 = CARTESIAN_POINT ( 'NONE',  ( 0.000000000000000000, 26.29521155129873122, -17.34211205339320117 ) ) ;
#26212 = FACE_OUTER_BOUND ( 'NONE', #23005, .T. ) ;
#26213 = ORIENTED_EDGE ( 'NONE', *, *, #2954, .F. ) ;
#26214 = DIRECTION ( 'NONE',  ( 1.000000000000000000, 0.000000000000000000, 0.000000000000000000 ) ) ;
#26215 = ORIENTED_EDGE ( 'NONE', *, *, #20236, .F. ) ;
#26216 = VERTEX_POINT ( 'NONE', #38932 ) ;
#26217 = DIRECTION ( 'NONE',  ( 0.000000000000000000, 0.000000000000000000, 1.000000000000000000 ) ) ;
#26218 = CARTESIAN_POINT ( 'NONE',  ( 97.09201668843397215, 31.00000000000000000, 6.474068422258194566 ) ) ;
#26219 = EDGE_LOOP ( 'NONE', ( #18469, #9688, #30993, #17113 ) ) ;
#26220 = CARTESIAN_POINT ( 'NONE',  ( 17.99999999999999645, 18.25486108452625089, 25.66996392254279868 ) ) ;
#26221 = FACE_OUTER_BOUND ( 'NONE', #18058, .T. ) ;
#26222 = CIRCLE ( 'NONE', #30400, 2.799122904894268071 ) ;
#26223 = CYLINDRICAL_SURFACE ( 'NONE', #23405, 13.59999999999999964 ) ;
#26224 = ORIENTED_EDGE ( 'NONE', *, *, #2675, .F. ) ;
#26225 = EDGE_CURVE ( 'NONE', #42671, #35898, #35066, .T. ) ;
#26226 = DIRECTION ( 'NONE',  ( -1.000000000000000000, -0.000000000000000000, 0.000000000000000000 ) ) ;
#26227 = EDGE_CURVE ( 'NONE', #6210, #40010, #42622, .T. ) ;
#26228 = AXIS2_PLACEMENT_3D ( 'NONE', #24302, #37558, #26894 ) ;
#26229 = CARTESIAN_POINT ( 'NONE',  ( 17.99999999999999645, 31.81777574834305966, -2.898764365605425830 ) ) ;
#26230 = AXIS2_PLACEMENT_3D ( 'NONE', #12079, #5513, #6148 ) ;
#26231 = EDGE_CURVE ( 'NONE', #18907, #15552, #7911, .T. ) ;
#26233 = CARTESIAN_POINT ( 'NONE',  ( 17.99999999999999645, -3.803237743091689715, -31.26855263151018960 ) ) ;
#26232 = DIRECTION ( 'NONE',  ( 1.000000000000000000, -1.373900992973641868E-15, -3.994789077170585140E-16 ) ) ;
#26234 = AXIS2_PLACEMENT_3D ( 'NONE', #7174, #20531, #30552 ) ;
#26235 = DIRECTION ( 'NONE',  ( 0.000000000000000000, 0.000000000000000000, 1.000000000000000000 ) ) ;
#26236 = ORIENTED_EDGE ( 'NONE', *, *, #12503, .F. ) ;
#26237 = DIRECTION ( 'NONE',  ( 0.000000000000000000, 0.000000000000000000, 1.000000000000000000 ) ) ;
#26238 = AXIS2_PLACEMENT_3D ( 'NONE', #360, #7582, #33114 ) ;
#26239 = CARTESIAN_POINT ( 'NONE',  ( -12.50349052776452297, 31.00000000000000355, 25.37591446456323041 ) ) ;
#26240 = ORIENTED_EDGE ( 'NONE', *, *, #34899, .T. ) ;
#26241 = LINE ( 'NONE', #36452, #24822 ) ;
#26242 = CARTESIAN_POINT ( 'NONE',  ( 18.00000000000000355, 42.60732521687599217, -19.80331771201614544 ) ) ;
#26243 = ORIENTED_EDGE ( 'NONE', *, *, #11897, .T. ) ;
#26244 = AXIS2_PLACEMENT_3D ( 'NONE', #26507, #30650, #33262 ) ;
#26245 = CARTESIAN_POINT ( 'NONE',  ( 8.999999999999998224, 12.42760411676038146, 33.78690065568429191 ) ) ;
#26246 = CARTESIAN_POINT ( 'NONE',  ( 22.24487986055951083, 40.00000000000000000, 28.98451114863597766 ) ) ;
#26247 = ADVANCED_FACE ( 'NONE', ( #39343 ), #15840, .F. ) ;
#26248 = CARTESIAN_POINT ( 'NONE',  ( -25.29816761084670063, 40.00000000000000000, 43.63644233508315295 ) ) ;
#26249 = VERTEX_POINT ( 'NONE', #35652 ) ;
#26250 = ORIENTED_EDGE ( 'NONE', *, *, #33819, .T. ) ;
#26251 = DIRECTION ( 'NONE',  ( 3.996523416598993920E-16, 2.658563593772947074E-15, 1.000000000000000000 ) ) ;
#26252 = CYLINDRICAL_SURFACE ( 'NONE', #10945, 130.0000000000000284 ) ;
#26253 = AXIS2_PLACEMENT_3D ( 'NONE', #25075, #24626, #5154 ) ;
#26254 = CARTESIAN_POINT ( 'NONE',  ( 0.000000000000000000, 0.000000000000000000, 0.000000000000000000 ) ) ;
#26255 = CIRCLE ( 'NONE', #40142, 20.00000000000001421 ) ;
#26256 = DIRECTION ( 'NONE',  ( 0.000000000000000000, 0.000000000000000000, 1.000000000000000000 ) ) ;
#26257 = CIRCLE ( 'NONE', #10234, 13.59999999999999964 ) ;
#26258 = EDGE_CURVE ( 'NONE', #18549, #8622, #14190, .T. ) ;
#26259 = CARTESIAN_POINT ( 'NONE',  ( 0.000000000000000000, -7.162210897275391730, -51.50439529848834042 ) ) ;
#26260 = ORIENTED_EDGE ( 'NONE', *, *, #6607, .T. ) ;
#26261 = DIRECTION ( 'NONE',  ( 0.000000000000000000, 0.000000000000000000, 1.000000000000000000 ) ) ;
#26262 = ORIENTED_EDGE ( 'NONE', *, *, #42821, .T. ) ;
#26263 = LINE ( 'NONE', #23430, #7614 ) ;
#26264 = DIRECTION ( 'NONE',  ( -1.000000000000000000, 1.373900992973642066E-15, 4.525365589504737954E-16 ) ) ;
#26265 = CIRCLE ( 'NONE', #6746, 58.99999999999999289 ) ;
#26266 = EDGE_CURVE ( 'NONE', #20422, #19261, #9481, .T. ) ;
#26267 = CIRCLE ( 'NONE', #26950, 13.60000000000000320 ) ;
#26268 = DIRECTION ( 'NONE',  ( -1.000000000000000000, 0.000000000000000000, -0.000000000000000000 ) ) ;
#26269 = DIRECTION ( 'NONE',  ( -1.000000000000000000, -0.000000000000000000, -0.000000000000000000 ) ) ;
#26270 = ORIENTED_EDGE ( 'NONE', *, *, #20460, .T. ) ;
#26271 = FACE_OUTER_BOUND ( 'NONE', #20868, .T. ) ;
#26272 = ORIENTED_EDGE ( 'NONE', *, *, #20427, .T. ) ;
#26273 = DIRECTION ( 'NONE',  ( -1.000000000000000000, 0.000000000000000000, 0.000000000000000000 ) ) ;
#26274 = ORIENTED_EDGE ( 'NONE', *, *, #7152, .F. ) ;
#26276 = ORIENTED_EDGE ( 'NONE', *, *, #28685, .F. ) ;
#26275 = DIRECTION ( 'NONE',  ( 0.000000000000000000, 0.000000000000000000, 1.000000000000000000 ) ) ;
#26277 = AXIS2_PLACEMENT_3D ( 'NONE', #38289, #5350, #8608 ) ;
#26278 = CARTESIAN_POINT ( 'NONE',  ( -7.911223860809958097, 31.00000000000000355, 59.30865348673673765 ) ) ;
#26279 = ORIENTED_EDGE ( 'NONE', *, *, #8496, .F. ) ;
#26280 = DIRECTION ( 'NONE',  ( 1.000000000000000000, 0.000000000000000000, 0.000000000000000000 ) ) ;
#26281 = ORIENTED_EDGE ( 'NONE', *, *, #39576, .F. ) ;
#26282 = DIRECTION ( 'NONE',  ( -3.996523416598930318E-16, 2.658563593772947863E-15, 1.000000000000000000 ) ) ;
#26283 = PRODUCT ( 'hex flange nut gradea_iso_ISO - 4161 - M5 - N', 'hex flange nut gradea_iso_ISO - 4161 - M5 - N', '', ( #24708 ) ) ;
#26284 = EDGE_LOOP ( 'NONE', ( #38662, #32751, #14907, #2061 ) ) ;
#26285 = CARTESIAN_POINT ( 'NONE',  ( -77.35014290652780744, 40.00000000000000711, 26.14598721591455899 ) ) ;
#26286 = EDGE_CURVE ( 'NONE', #8183, #41276, #37860, .T. ) ;
#26287 = AXIS2_PLACEMENT_3D ( 'NONE', #32845, #42006, #6013 ) ;
#26289 = FACE_OUTER_BOUND ( 'NONE', #40344, .T. ) ;
#26288 = DIRECTION ( 'NONE',  ( 0.000000000000000000, 0.9980267284282712259, 0.06279051952931685721 ) ) ;
#26290 = EDGE_CURVE ( 'NONE', #33425, #35058, #6203, .T. ) ;
#26291 = FACE_OUTER_BOUND ( 'NONE', #29170, .T. ) ;
#26292 = EDGE_LOOP ( 'NONE', ( #23117, #26861, #21169, #33343 ) ) ;
#26293 = CARTESIAN_POINT ( 'NONE',  ( 17.99999999999999645, -34.03109950475805334, 115.5957406979048727 ) ) ;
#26294 = CIRCLE ( 'NONE', #2583, 120.5010000000000474 ) ;
#26295 = ORIENTED_EDGE ( 'NONE', *, *, #3396, .F. ) ;
#26296 = AXIS2_PLACEMENT_3D ( 'NONE', #29485, #12488, #25804 ) ;
#26297 = VECTOR ( 'NONE', #24846, 1000.000000000000000 ) ;
#26298 = CARTESIAN_POINT ( 'NONE',  ( 18.00000000000000355, 0.000000000000000000, 0.000000000000000000 ) ) ;
#26299 = DIRECTION ( 'NONE',  ( 0.000000000000000000, -0.3681245526846654847, -0.9297764858882564543 ) ) ;
#26300 = AXIS2_PLACEMENT_3D ( 'NONE', #2291, #20989, #17491 ) ;
#26301 = CARTESIAN_POINT ( 'NONE',  ( -20.19574676229028043, 31.00000000000000355, 75.42596061005518493 ) ) ;
#26303 = DIRECTION ( 'NONE',  ( 1.000000000000000000, 0.000000000000000000, 0.000000000000000000 ) ) ;
#26302 = DIRECTION ( 'NONE',  ( -1.000000000000000000, 0.000000000000000000, 0.000000000000000000 ) ) ;
#26305 = ORIENTED_EDGE ( 'NONE', *, *, #1041, .F. ) ;
#26304 = CIRCLE ( 'NONE', #36698, 116.0000000000000000 ) ;
#26306 = AXIS2_PLACEMENT_3D ( 'NONE', #24062, #37330, #20807 ) ;
#26307 = ADVANCED_FACE ( 'NONE', ( #25250 ), #2692, .F. ) ;
#26308 = SURFACE_SIDE_STYLE ('',( #31990 ) ) ;
#26309 = CIRCLE ( 'NONE', #11185, 2.649999999999987477 ) ;
#26310 = ORIENTED_EDGE ( 'NONE', *, *, #11365, .T. ) ;
#26311 = DIRECTION ( 'NONE',  ( -0.7071067811865364705, 8.659560562355067211E-17, -0.7071067811865584529 ) ) ;
#26312 = FACE_OUTER_BOUND ( 'NONE', #34829, .T. ) ;
#26313 = CARTESIAN_POINT ( 'NONE',  ( 93.52153384689862037, 31.00000000000000000, -24.92737483788710406 ) ) ;
#26314 = CARTESIAN_POINT ( 'NONE',  ( 42.30527206516848793, 40.00000000000000000, -85.53883208674149330 ) ) ;
#26315 = DIRECTION ( 'NONE',  ( 0.000000000000000000, 0.000000000000000000, 1.000000000000000000 ) ) ;
#26316 = EDGE_CURVE ( 'NONE', #32971, #11054, #5818, .T. ) ;
#26317 = DIRECTION ( 'NONE',  ( -1.000000000000000000, -0.000000000000000000, -0.000000000000000000 ) ) ;
#26318 = ORIENTED_EDGE ( 'NONE', *, *, #43021, .T. ) ;
#26319 = CYLINDRICAL_SURFACE ( 'NONE', #43013, 20.00000000000000355 ) ;
#26320 = VERTEX_POINT ( 'NONE', #19341 ) ;
#26321 = LINE ( 'NONE', #9923, #38826 ) ;
#26322 = EDGE_CURVE ( 'NONE', #32556, #10881, #35231, .T. ) ;
#26323 = CIRCLE ( 'NONE', #6797, 13.59999999999999964 ) ;
#26324 = CARTESIAN_POINT ( 'NONE',  ( 0.000000000000000000, -24.70533337038242294, 26.18485254986683586 ) ) ;
#26325 = FACE_OUTER_BOUND ( 'NONE', #35413, .T. ) ;
#26326 = ORIENTED_EDGE ( 'NONE', *, *, #28684, .T. ) ;
#26327 = CARTESIAN_POINT ( 'NONE',  ( 9.000000000000000000, 34.45183346761150034, -10.44371441202619621 ) ) ;
#26328 = DIRECTION ( 'NONE',  ( 0.000000000000000000, 0.000000000000000000, 1.000000000000000000 ) ) ;
#26329 = AXIS2_PLACEMENT_3D ( 'NONE', #28387, #1511, #4801 ) ;
#26330 = AXIS2_PLACEMENT_3D ( 'NONE', #16729, #30020, #29810 ) ;
#26332 = ORIENTED_EDGE ( 'NONE', *, *, #29641, .T. ) ;
#26331 = CARTESIAN_POINT ( 'NONE',  ( 109.0695705685741075, 106.4195705685767166, 10.00000000000000000 ) ) ;
#26333 = CARTESIAN_POINT ( 'NONE',  ( 18.00000000000000355, 6.109652351741791776, 46.58570277113511793 ) ) ;
#26334 = DIRECTION ( 'NONE',  ( 1.000000000000000000, 0.000000000000000000, 0.000000000000000000 ) ) ;
#26335 = ADVANCED_FACE ( 'NONE', ( #2063 ), #9262, .T. ) ;
#26336 = AXIS2_PLACEMENT_3D ( 'NONE', #14743, #31088, #34787 ) ;
#26338 = ORIENTED_EDGE ( 'NONE', *, *, #24419, .F. ) ;
#26337 = CARTESIAN_POINT ( 'NONE',  ( 9.000000000000001776, 23.85344185397197947, 113.5209818126991621 ) ) ;
#26339 = VERTEX_POINT ( 'NONE', #17966 ) ;
#26340 = DIRECTION ( 'NONE',  ( 0.000000000000000000, 0.6845471059286846183, 0.7289686274214153272 ) ) ;
#26341 = LINE ( 'NONE', #43099, #8480 ) ;
#26342 = CARTESIAN_POINT ( 'NONE',  ( 36.84045577241590763, 40.00000000000000000, -41.86038302679909151 ) ) ;
#26343 = CYLINDRICAL_SURFACE ( 'NONE', #25795, 116.0000000000000000 ) ;
#26344 = AXIS2_PLACEMENT_3D ( 'NONE', #26126, #39615, #36547 ) ;
#26345 = EDGE_CURVE ( 'NONE', #4115, #5703, #4150, .T. ) ;
#26346 = EDGE_CURVE ( 'NONE', #30436, #7181, #30220, .T. ) ;
#26347 = LINE ( 'NONE', #13255, #22201 ) ;
#26348 = EDGE_CURVE ( 'NONE', #20934, #7958, #24287, .T. ) ;
#26349 = EDGE_CURVE ( 'NONE', #7683, #25070, #40616, .T. ) ;
#26350 = DIRECTION ( 'NONE',  ( 1.000000000000000000, 0.000000000000000000, 0.000000000000000000 ) ) ;
#26351 = ORIENTED_EDGE ( 'NONE', *, *, #6640, .T. ) ;
#26352 = DIRECTION ( 'NONE',  ( 0.000000000000000000, 0.000000000000000000, 1.000000000000000000 ) ) ;
#26353 = ORIENTED_EDGE ( 'NONE', *, *, #27560, .T. ) ;
#26354 = FACE_OUTER_BOUND ( 'NONE', #5527, .T. ) ;
#26355 = CARTESIAN_POINT ( 'NONE',  ( -4.000000000000000000, -2.309401076758512694, -3.433295621305382461 ) ) ;
#26356 = CARTESIAN_POINT ( 'NONE',  ( 41.10549127292548377, 31.00000000000000355, 20.25863663968860706 ) ) ;
#26357 = CARTESIAN_POINT ( 'NONE',  ( 12.40854556226731198, -35.35525454449573601, -74.83297477053802993 ) ) ;
#26358 = VERTEX_POINT ( 'NONE', #33840 ) ;
#26359 = AXIS2_PLACEMENT_3D ( 'NONE', #19836, #33103, #20067 ) ;
#26360 = VECTOR ( 'NONE', #2274, 1000.000000000000000 ) ;
#26361 = DIRECTION ( 'NONE',  ( 0.000000000000000000, -0.1590634960190596414, -0.9872683547213465527 ) ) ;
#26362 = CARTESIAN_POINT ( 'NONE',  ( -89.89583333403318477, 31.00000000000000711, 5.890486217120591839 ) ) ;
#26363 = CIRCLE ( 'NONE', #34691, 59.00000000000000000 ) ;
#26364 = CARTESIAN_POINT ( 'NONE',  ( 0.000000000000000000, 52.19040376560566585, -99.31985817764127944 ) ) ;
#26365 = VERTEX_POINT ( 'NONE', #37326 ) ;
#26367 = CARTESIAN_POINT ( 'NONE',  ( -31.21560191380782001, 31.00000000000000355, 63.07420938637471863 ) ) ;
#26366 = CIRCLE ( 'NONE', #14545, 18.77999999999999403 ) ;
#26368 = CARTESIAN_POINT ( 'NONE',  ( 4.437437895627098783, 40.00000000000000000, 69.40004907513484511 ) ) ;
#26369 = DIRECTION ( 'NONE',  ( -0.000000000000000000, -0.000000000000000000, 1.000000000000000000 ) ) ;
#26370 = ORIENTED_EDGE ( 'NONE', *, *, #23676, .F. ) ;
#26371 = LINE ( 'NONE', #43130, #25547 ) ;
#26372 = CARTESIAN_POINT ( 'NONE',  ( 8.999999999999998224, -59.47573314508800024, 99.59235496188593117 ) ) ;
#26373 = CARTESIAN_POINT ( 'NONE',  ( -16.41266422346948772, 40.00000000000000000, -1.216702565357022037 ) ) ;
#26374 = EDGE_CURVE ( 'NONE', #1401, #51, #15596, .T. ) ;
#26376 = ORIENTED_EDGE ( 'NONE', *, *, #9438, .T. ) ;
#26375 = CARTESIAN_POINT ( 'NONE',  ( -10.00000000000000000, 0.000000000000000000, 0.000000000000000000 ) ) ;
#26377 = DIRECTION ( 'NONE',  ( 0.000000000000000000, 0.5076658003388352380, 0.8615540813938089570 ) ) ;
#26378 = ORIENTED_EDGE ( 'NONE', *, *, #41790, .F. ) ;
#26379 = DIRECTION ( 'NONE',  ( 3.996523416598993920E-16, 2.658563593772947074E-15, 1.000000000000000000 ) ) ;
#26380 = CARTESIAN_POINT ( 'NONE',  ( 36.74538074116732389, 40.00000000000000000, -63.64477163140654170 ) ) ;
#26381 = CYLINDRICAL_SURFACE ( 'NONE', #25058, 116.0000000000000000 ) ;
#26382 = VERTEX_POINT ( 'NONE', #7870 ) ;
#26383 = DIRECTION ( 'NONE',  ( 0.000000000000000000, 1.000000000000000000, 0.000000000000000000 ) ) ;
#26384 = CIRCLE ( 'NONE', #38906, 116.0000000000000000 ) ;
#26385 = CARTESIAN_POINT ( 'NONE',  ( 0.000000000000000000, 29.02167576844106023, 108.3790330702170621 ) ) ;
#26386 = CIRCLE ( 'NONE', #2664, 20.00000000000000711 ) ;
#26387 = EDGE_LOOP ( 'NONE', ( #2553, #15947, #13326, #28129 ) ) ;
#26388 = CIRCLE ( 'NONE', #8256, 0.2000000000000000944 ) ;
#26389 = ORIENTED_EDGE ( 'NONE', *, *, #19708, .F. ) ;
#26390 = CARTESIAN_POINT ( 'NONE',  ( 17.99999999999999645, -112.1427988504408120, 3.502162136923045566 ) ) ;
#26391 = EDGE_LOOP ( 'NONE', ( #8338, #18645, #18953, #9878 ) ) ;
#26392 = AXIS2_PLACEMENT_3D ( 'NONE', #13176, #26469, #32578 ) ;
#26393 = CARTESIAN_POINT ( 'NONE',  ( 17.99999999999999645, 45.89132998248186368, -102.3829004574625401 ) ) ;
#26394 = DIRECTION ( 'NONE',  ( 0.000000000000000000, 0.000000000000000000, -1.000000000000000000 ) ) ;
#26395 = DIRECTION ( 'NONE',  ( 1.000000000000000000, 0.000000000000000000, 0.000000000000000000 ) ) ;
#26396 = ADVANCED_FACE ( 'NONE', ( #27312 ), #4590, .T. ) ;
#26397 = EDGE_CURVE ( 'NONE', #10253, #38578, #20502, .T. ) ;
#26398 = CARTESIAN_POINT ( 'NONE',  ( 4.000000000000000888, 1.539600717838996990, -3.300726591567079815 ) ) ;
#26399 = EDGE_LOOP ( 'NONE', ( #22820, #19444, #36476, #30658 ) ) ;
#26400 = CARTESIAN_POINT ( 'NONE',  ( 17.99999999999999645, 2.418575551220858877, 120.4767259403369053 ) ) ;
#26401 = EDGE_CURVE ( 'NONE', #17636, #17009, #41342, .T. ) ;
#26402 = VERTEX_POINT ( 'NONE', #20802 ) ;
#26403 = CARTESIAN_POINT ( 'NONE',  ( 0.000000000000000000, -0.5156212287287311735, 112.1962860721878172 ) ) ;
#26404 = CARTESIAN_POINT ( 'NONE',  ( -19.99999999999999645, 31.00000000000000355, 2.168407390121265812E-15 ) ) ;
#26405 = VERTEX_POINT ( 'NONE', #7656 ) ;
#26406 = CARTESIAN_POINT ( 'NONE',  ( 0.000000000000000000, 61.59243992711585491, -93.77976230225978327 ) ) ;
#26407 = DIRECTION ( 'NONE',  ( 0.000000000000000000, -0.8951632913550570114, -0.4457383557765488558 ) ) ;
#26408 = ITEM_DEFINED_TRANSFORMATION ( 'NONE', 'NONE', #9346,  #13552 ) ;
#26409 = CARTESIAN_POINT ( 'NONE',  ( 0.000000000000000000, -115.9387338813861277, -3.769613505537241949 ) ) ;
#26410 = CARTESIAN_POINT ( 'NONE',  ( 64.37268382102905662, 31.00000000000000000, -8.487791176987355968 ) ) ;
#26411 = EDGE_CURVE ( 'NONE', #33890, #34535, #28145, .T. ) ;
#26412 = EDGE_LOOP ( 'NONE', ( #26753, #30228, #16043, #29404 ) ) ;
#26413 = CIRCLE ( 'NONE', #7586, 51.99999999999999289 ) ;
#26414 = CARTESIAN_POINT ( 'NONE',  ( 28.69597684714336339, 31.00000000000000355, 25.25520295781697655 ) ) ;
#26415 = CARTESIAN_POINT ( 'NONE',  ( -54.82550897924149069, 40.00000000000000711, 42.06954809655981364 ) ) ;
#26416 = AXIS2_PLACEMENT_3D ( 'NONE', #29116, #38904, #31953 ) ;
#26417 = LINE ( 'NONE', #19671, #36757 ) ;
#26418 = DIRECTION ( 'NONE',  ( 0.000000000000000000, 0.5264321628773570572, -0.8502171357296134380 ) ) ;
#26419 = CARTESIAN_POINT ( 'NONE',  ( 0.000000000000000000, -6.854627147199490622, 115.7972974066013307 ) ) ;
#26420 = ORIENTED_EDGE ( 'NONE', *, *, #41422, .F. ) ;
#26421 = CARTESIAN_POINT ( 'NONE',  ( 13.85568741775851542, 40.00000000000000000, -40.82620080729295609 ) ) ;
#26422 = FACE_OUTER_BOUND ( 'NONE', #15379, .T. ) ;
#26423 = CARTESIAN_POINT ( 'NONE',  ( 17.99999999999999645, 0.000000000000000000, 0.000000000000000000 ) ) ;
#26424 = ORIENTED_EDGE ( 'NONE', *, *, #27733, .T. ) ;
#26425 = DIRECTION ( 'NONE',  ( 0.000000000000000000, -0.5264321628773450668, -0.8502171357296208765 ) ) ;
#26426 = CARTESIAN_POINT ( 'NONE',  ( 17.99999999999999645, -62.45178862086154226, -93.20969140437570388 ) ) ;
#26427 = VERTEX_POINT ( 'NONE', #27107 ) ;
#26428 = CYLINDRICAL_SURFACE ( 'NONE', #20749, 20.00000000000000355 ) ;
#26429 = ORIENTED_EDGE ( 'NONE', *, *, #1366, .F. ) ;
#26430 = EDGE_LOOP ( 'NONE', ( #23422, #1306 ) ) ;
#26431 = DIRECTION ( 'NONE',  ( 0.000000000000000000, 0.000000000000000000, 1.000000000000000000 ) ) ;
#26432 = CARTESIAN_POINT ( 'NONE',  ( 91.58570893733639195, 31.00000000000000000, -30.97307622143650363 ) ) ;
#26433 = VERTEX_POINT ( 'NONE', #27760 ) ;
#26434 = DIRECTION ( 'NONE',  ( -1.000000000000000000, 0.000000000000000000, 0.000000000000000000 ) ) ;
#26435 = AXIS2_PLACEMENT_3D ( 'NONE', #10538, #16463, #13402 ) ;
#26436 = AXIS2_PLACEMENT_3D ( 'NONE', #42779, #9427, #16667 ) ;
#26437 = CARTESIAN_POINT ( 'NONE',  ( 0.000000000000000000, 0.000000000000000000, 6.999999999999998224 ) ) ;
#26438 = EDGE_CURVE ( 'NONE', #9587, #11400, #8589, .T. ) ;
#26439 = DIRECTION ( 'NONE',  ( -1.000000000000000000, 0.000000000000000000, 0.000000000000000000 ) ) ;
#26440 = EDGE_LOOP ( 'NONE', ( #30680, #17917, #21022, #11036 ) ) ;
#26441 = CARTESIAN_POINT ( 'NONE',  ( 0.000000000000000000, -78.75547124681428102, 91.20343606296975736 ) ) ;
#26442 = DIRECTION ( 'NONE',  ( -1.000000000000000000, -0.000000000000000000, 0.000000000000000000 ) ) ;
#26444 = DIRECTION ( 'NONE',  ( 0.000000000000000000, 0.000000000000000000, 1.000000000000000000 ) ) ;
#26443 = DIRECTION ( 'NONE',  ( 0.000000000000000000, 0.000000000000000000, -1.000000000000000000 ) ) ;
#26445 = EDGE_CURVE ( 'NONE', #24259, #24001, #12991, .T. ) ;
#26446 = CARTESIAN_POINT ( 'NONE',  ( 18.00000000000000355, -11.46872990052349550, -45.56340405422456286 ) ) ;
#26447 = ORIENTED_EDGE ( 'NONE', *, *, #22989, .F. ) ;
#26448 = EDGE_CURVE ( 'NONE', #10279, #13305, #17697, .T. ) ;
#26449 = SURFACE_STYLE_USAGE ( .BOTH. , #42999 ) ;
#26450 = CARTESIAN_POINT ( 'NONE',  ( 29.64712525329720449, 31.00000000000000355, -17.12831674356021239 ) ) ;
#26451 = EDGE_LOOP ( 'NONE', ( #27968, #39908 ) ) ;
#26452 = CARTESIAN_POINT ( 'NONE',  ( 0.000000000000000000, -35.11945359308084136, -38.34871548466050939 ) ) ;
#26453 = EDGE_CURVE ( 'NONE', #8821, #36472, #30797, .T. ) ;
#26454 = DIRECTION ( 'NONE',  ( 0.000000000000000000, -0.9714298932647074114, -0.2373266998711251186 ) ) ;
#26455 = EDGE_LOOP ( 'NONE', ( #264, #29739, #33887, #2500 ) ) ;
#26456 = DIRECTION ( 'NONE',  ( 0.000000000000000000, 0.000000000000000000, 1.000000000000000000 ) ) ;
#26457 = CARTESIAN_POINT ( 'NONE',  ( -16.93500259178182432, 40.00000000000000000, 34.36424406943201149 ) ) ;
#26458 = CARTESIAN_POINT ( 'NONE',  ( -40.56882557769177566, 40.00000000000000000, 31.01417895415859505 ) ) ;
#26459 = AXIS2_PLACEMENT_3D ( 'NONE', #23089, #16535, #6248 ) ;
#26460 = VERTEX_POINT ( 'NONE', #6412 ) ;
#26461 = VERTEX_POINT ( 'NONE', #19764 ) ;
#26462 = CARTESIAN_POINT ( 'NONE',  ( -31.75000000000000000, 0.000000000000000000, 0.000000000000000000 ) ) ;
#26463 = DIRECTION ( 'NONE',  ( -1.000000000000000000, -0.000000000000000000, -0.000000000000000000 ) ) ;
#26464 = CIRCLE ( 'NONE', #33398, 120.5010000000000190 ) ;
#26465 = DIRECTION ( 'NONE',  ( -3.996523416598930318E-16, 2.658563593772947863E-15, 1.000000000000000000 ) ) ;
#26466 = CARTESIAN_POINT ( 'NONE',  ( 18.00000000000000355, -35.20873326984102647, 31.88259874184018372 ) ) ;
#26467 = CARTESIAN_POINT ( 'NONE',  ( 0.000000000000000000, -39.78933988720098114, -24.98727647985043276 ) ) ;
#26468 = ORIENTED_EDGE ( 'NONE', *, *, #6812, .F. ) ;
#26469 = DIRECTION ( 'NONE',  ( -1.000000000000000000, -0.000000000000000000, -0.000000000000000000 ) ) ;
#26470 = EDGE_LOOP ( 'NONE', ( #6069, #10846, #24482, #30275 ) ) ;
#26471 = DIRECTION ( 'NONE',  ( 0.000000000000000000, 0.000000000000000000, 1.000000000000000000 ) ) ;
#26472 = ADVANCED_FACE ( 'NONE', ( #872 ), #16485, .F. ) ;
#26473 = DIRECTION ( 'NONE',  ( 0.000000000000000000, 0.000000000000000000, 1.000000000000000000 ) ) ;
#26474 =( REPRESENTATION_RELATIONSHIP ('NONE','NONE', #330, #18009 ) REPRESENTATION_RELATIONSHIP_WITH_TRANSFORMATION ( #23584 )SHAPE_REPRESENTATION_RELATIONSHIP( ) );
#26475 = ORIENTED_EDGE ( 'NONE', *, *, #33750, .F. ) ;
#26476 = LINE ( 'NONE', #41261, #14497 ) ;
#26477 = DIRECTION ( 'NONE',  ( -1.000000000000000000, 0.000000000000000000, -0.000000000000000000 ) ) ;
#26478 = VERTEX_POINT ( 'NONE', #10504 ) ;
#26479 = CYLINDRICAL_SURFACE ( 'NONE', #8941, 36.00000000000000000 ) ;
#26480 = ORIENTED_EDGE ( 'NONE', *, *, #8495, .T. ) ;
#26481 = CYLINDRICAL_SURFACE ( 'NONE', #6777, 2.649999999999993694 ) ;
#26482 = ORIENTED_EDGE ( 'NONE', *, *, #25037, .T. ) ;
#26484 = VERTEX_POINT ( 'NONE', #23844 ) ;
#26483 = CARTESIAN_POINT ( 'NONE',  ( -6.004904395537136175, 0.000000000000000000, 19.19999999999999574 ) ) ;
#26485 = CARTESIAN_POINT ( 'NONE',  ( 58.81396797841471624, 31.00000000000000355, 34.08301911901634895 ) ) ;
#26486 = VERTEX_POINT ( 'NONE', #20571 ) ;
#26487 = CARTESIAN_POINT ( 'NONE',  ( 9.000000000000001776, -112.8457601792517124, 26.86697618949339272 ) ) ;
#26488 = EDGE_CURVE ( 'NONE', #17450, #11761, #26050, .T. ) ;
#26489 = EDGE_LOOP ( 'NONE', ( #34747, #33241, #16318, #13463 ) ) ;
#26490 = DIRECTION ( 'NONE',  ( -1.000000000000000000, 0.000000000000000000, 0.000000000000000000 ) ) ;
#26491 = ORIENTED_EDGE ( 'NONE', *, *, #33372, .T. ) ;
#26492 = CARTESIAN_POINT ( 'NONE',  ( -10.92011822083620309, 40.00000000000000000, -83.75917815547794021 ) ) ;
#26493 = AXIS2_PLACEMENT_3D ( 'NONE', #35198, #5322, #15391 ) ;
#26494 = CIRCLE ( 'NONE', #32070, 116.0000000000000000 ) ;
#26495 = VECTOR ( 'NONE', #18856, 1000.000000000000000 ) ;
#26497 = CARTESIAN_POINT ( 'NONE',  ( 17.99999999999999645, -21.55123232222554464, 118.5581519187671660 ) ) ;
#26496 = DIRECTION ( 'NONE',  ( -1.000000000000000000, 0.000000000000000000, 0.000000000000000000 ) ) ;
#26498 = CIRCLE ( 'NONE', #34178, 58.99999999999999289 ) ;
#26499 = CYLINDRICAL_SURFACE ( 'NONE', #1754, 59.00000000000000000 ) ;
#26500 = ORIENTED_EDGE ( 'NONE', *, *, #15296, .T. ) ;
#26501 = DIRECTION ( 'NONE',  ( 1.000000000000000000, 0.000000000000000000, 0.000000000000000000 ) ) ;
#26502 = ORIENTED_EDGE ( 'NONE', *, *, #28220, .T. ) ;
#26503 = EDGE_CURVE ( 'NONE', #5464, #24053, #40800, .T. ) ;
#26504 = CARTESIAN_POINT ( 'NONE',  ( 42.80287614962796994, -2.055254544495723756, 69.29271901957280022 ) ) ;
#26505 = CARTESIAN_POINT ( 'NONE',  ( 58.80104710710317306, 31.00000000000000000, -45.11949705600698479 ) ) ;
#26507 = CARTESIAN_POINT ( 'NONE',  ( 0.000000000000000000, 0.000000000000000000, 0.000000000000000000 ) ) ;
#26506 = CYLINDRICAL_SURFACE ( 'NONE', #4419, 59.00000000000000000 ) ;
#26508 = VERTEX_POINT ( 'NONE', #34921 ) ;
#26509 = FACE_OUTER_BOUND ( 'NONE', #11852, .T. ) ;
#26510 = AXIS2_PLACEMENT_3D ( 'NONE', #35347, #28409, #28822 ) ;
#26511 = VERTEX_POINT ( 'NONE', #1532 ) ;
#26512 = DIRECTION ( 'NONE',  ( 1.000000000000000000, 0.000000000000000000, 0.000000000000000000 ) ) ;
#26513 = CARTESIAN_POINT ( 'NONE',  ( 18.00000000000000355, 0.000000000000000000, 0.000000000000000000 ) ) ;
#26514 = CARTESIAN_POINT ( 'NONE',  ( -72.38966680861454961, 31.00000000000000711, 55.38960906678870089 ) ) ;
#26515 = DIRECTION ( 'NONE',  ( -1.000000000000000000, -0.000000000000000000, -0.000000000000000000 ) ) ;
#26516 = VECTOR ( 'NONE', #33076, 1000.000000000000114 ) ;
#26517 = CARTESIAN_POINT ( 'NONE',  ( 0.000000000000000000, -36.06787431788703913, 37.45808914225474950 ) ) ;
#26518 = ORIENTED_EDGE ( 'NONE', *, *, #23626, .F. ) ;
#26519 = CYLINDRICAL_SURFACE ( 'NONE', #27051, 51.99999999999999289 ) ;
#26520 = ORIENTED_EDGE ( 'NONE', *, *, #630, .T. ) ;
#26522 = EDGE_CURVE ( 'NONE', #27469, #36133, #25356, .T. ) ;
#26521 = CIRCLE ( 'NONE', #7698, 59.00000000000000000 ) ;
#26523 = CARTESIAN_POINT ( 'NONE',  ( 17.99999999999999645, 24.70533337038261124, -26.18485254986667954 ) ) ;
#26524 = CIRCLE ( 'NONE', #28625, 2.649999999999971934 ) ;
#26526 = EDGE_CURVE ( 'NONE', #192, #39608, #28831, .T. ) ;
#26525 = CIRCLE ( 'NONE', #37627, 20.00000000000000711 ) ;
#26527 = DIRECTION ( 'NONE',  ( -1.000000000000000000, -0.000000000000000000, -0.000000000000000000 ) ) ;
#26528 = AXIS2_PLACEMENT_3D ( 'NONE', #31798, #11298, #25276 ) ;
#26529 = DIRECTION ( 'NONE',  ( -1.000000000000000000, -0.000000000000000000, 0.000000000000000000 ) ) ;
#26530 = ORIENTED_EDGE ( 'NONE', *, *, #13244, .T. ) ;
#26531 = DIRECTION ( 'NONE',  ( -1.000000000000000000, 0.000000000000000000, 0.000000000000000000 ) ) ;
#26532 = CYLINDRICAL_SURFACE ( 'NONE', #36801, 36.00000000000000000 ) ;
#26533 = CARTESIAN_POINT ( 'NONE',  ( 18.00000000000000355, 0.000000000000000000, 0.000000000000000000 ) ) ;
#26535 = EDGE_LOOP ( 'NONE', ( #15983, #17510, #16530, #33986 ) ) ;
#26534 = CYLINDRICAL_SURFACE ( 'NONE', #5474, 2.500000000000000444 ) ;
#26536 = CARTESIAN_POINT ( 'NONE',  ( -28.46928290085317315, 31.00000000000000355, -16.49637127829624106 ) ) ;
#26537 = DIRECTION ( 'NONE',  ( 0.000000000000000000, 1.000000000000000000, 0.000000000000000000 ) ) ;
#26538 = EDGE_CURVE ( 'NONE', #40845, #42638, #31615, .T. ) ;
#26540 = ORIENTED_EDGE ( 'NONE', *, *, #18319, .F. ) ;
#26539 = CARTESIAN_POINT ( 'NONE',  ( -15.99999999999997691, 17.11489954122026447, 5.571627607371296764E-15 ) ) ;
#26541 = ORIENTED_EDGE ( 'NONE', *, *, #10177, .F. ) ;
#26542 = CYLINDRICAL_SURFACE ( 'NONE', #4489, 0.7500000000000006661 ) ;
#26543 = CARTESIAN_POINT ( 'NONE',  ( 17.99999999999999645, 0.000000000000000000, 0.000000000000000000 ) ) ;
#26544 = CARTESIAN_POINT ( 'NONE',  ( -13.93478910046542829, 40.00000000000000000, -52.37520058408175316 ) ) ;
#26545 = DIRECTION ( 'NONE',  ( 0.000000000000000000, -1.000000000000000000, 0.000000000000000000 ) ) ;
#26546 = CIRCLE ( 'NONE', #7720, 120.5010000000000190 ) ;
#26547 = CARTESIAN_POINT ( 'NONE',  ( -31.75000000000000000, 0.000000000000000000, 0.000000000000000000 ) ) ;
#26548 = DIRECTION ( 'NONE',  ( 0.000000000000000000, 0.7865515558026436871, -0.6175246149461902645 ) ) ;
#26549 = AXIS2_PLACEMENT_3D ( 'NONE', #30642, #26501, #13206 ) ;
#26550 = VERTEX_POINT ( 'NONE', #8520 ) ;
#26551 = LINE ( 'NONE', #10606, #36233 ) ;
#26552 = ORIENTED_EDGE ( 'NONE', *, *, #40589, .T. ) ;
#26553 = ADVANCED_FACE ( 'NONE', ( #15326 ), #11379, .F. ) ;
#26554 = AXIS2_PLACEMENT_3D ( 'NONE', #12549, #5558, #18916 ) ;
#26555 = CARTESIAN_POINT ( 'NONE',  ( 18.00000000000000355, 51.85248208264522418, -3.914090171285654396 ) ) ;
#26556 = CYLINDRICAL_SURFACE ( 'NONE', #40773, 120.5010000000000190 ) ;
#26557 = VECTOR ( 'NONE', #41055, 1000.000000000000114 ) ;
#26558 = EDGE_CURVE ( 'NONE', #17666, #14830, #5104, .T. ) ;
#26559 = CARTESIAN_POINT ( 'NONE',  ( 19.15075862373047144, 31.00000000000000355, -38.85840887180553693 ) ) ;
#26560 = CARTESIAN_POINT ( 'NONE',  ( 17.99999999999999645, 0.000000000000000000, 0.000000000000000000 ) ) ;
#26561 = ORIENTED_EDGE ( 'NONE', *, *, #6345, .T. ) ;
#26562 = VECTOR ( 'NONE', #35474, 1000.000000000000000 ) ;
#26563 = CARTESIAN_POINT ( 'NONE',  ( 17.99999999999999645, 75.72520367775085504, 82.78868281116005789 ) ) ;
#26564 = ORIENTED_EDGE ( 'NONE', *, *, #34873, .T. ) ;
#26565 = CARTESIAN_POINT ( 'NONE',  ( 14.35450763783260797, 40.00000000000000000, -18.72194639494853874 ) ) ;
#26566 = CIRCLE ( 'NONE', #7049, 20.00000000000000711 ) ;
#26567 = ORIENTED_EDGE ( 'NONE', *, *, #8739, .F. ) ;
#26568 = LINE ( 'NONE', #33529, #26196 ) ;
#26569 = EDGE_LOOP ( 'NONE', ( #7576, #41705, #6485, #37304 ) ) ;
#26570 = CARTESIAN_POINT ( 'NONE',  ( -55.11358496760189496, 31.00000000000000711, 27.06326608205353779 ) ) ;
#26571 = CARTESIAN_POINT ( 'NONE',  ( 51.26988013557343749, 40.00000000000000000, 45.10883117380814866 ) ) ;
#26572 = CARTESIAN_POINT ( 'NONE',  ( 12.74197863150380883, 40.00000000000000000, 96.66318596537892915 ) ) ;
#26573 = ORIENTED_EDGE ( 'NONE', *, *, #3322, .F. ) ;
#26574 = EDGE_LOOP ( 'NONE', ( #26887, #37463, #35869, #2241 ) ) ;
#26575 = ADVANCED_FACE ( 'NONE', ( #18181 ), #14667, .F. ) ;
#26576 = DIRECTION ( 'NONE',  ( 0.000000000000000000, 0.9826841245925214130, -0.1852887240871113894 ) ) ;
#26577 = CARTESIAN_POINT ( 'NONE',  ( 0.000000000000000000, 0.000000000000000000, 0.000000000000000000 ) ) ;
#26578 = EDGE_CURVE ( 'NONE', #13372, #5751, #42702, .T. ) ;
#26579 = EDGE_CURVE ( 'NONE', #28841, #16283, #13508, .T. ) ;
#26580 = ADVANCED_FACE ( 'NONE', ( #27974 ), #2168, .F. ) ;
#26582 = ORIENTED_EDGE ( 'NONE', *, *, #1110, .T. ) ;
#26581 = LINE ( 'NONE', #23757, #10230 ) ;
#26583 = DIRECTION ( 'NONE',  ( 0.000000000000000000, 0.7525707698561354686, 0.6585113790650420906 ) ) ;
#26584 = CIRCLE ( 'NONE', #34723, 120.5010000000000332 ) ;
#26585 = ORIENTED_EDGE ( 'NONE', *, *, #18398, .T. ) ;
#26586 = CARTESIAN_POINT ( 'NONE',  ( -8.920000000000003482, 0.000000000000000000, 0.000000000000000000 ) ) ;
#26587 = CARTESIAN_POINT ( 'NONE',  ( -89.89583333403318477, 40.00000000000000711, 5.890486217120591839 ) ) ;
#26588 = CARTESIAN_POINT ( 'NONE',  ( 17.99999999999999645, -106.6051926090968180, -45.73109345704927620 ) ) ;
#26589 = AXIS2_PLACEMENT_3D ( 'NONE', #20617, #33888, #30839 ) ;
#26590 = AXIS2_PLACEMENT_3D ( 'NONE', #3483, #29709, #36653 ) ;
#26591 = VERTEX_POINT ( 'NONE', #35350 ) ;
#26592 = DIRECTION ( 'NONE',  ( 0.000000000000000000, 0.000000000000000000, 1.000000000000000000 ) ) ;
#26593 = CARTESIAN_POINT ( 'NONE',  ( 0.000000000000000000, 0.000000000000000000, 0.000000000000000000 ) ) ;
#26594 = CIRCLE ( 'NONE', #37007, 36.00000000000000000 ) ;
#26595 = ORIENTED_EDGE ( 'NONE', *, *, #42187, .T. ) ;
#26596 = VERTEX_POINT ( 'NONE', #38833 ) ;
#26597 = DIRECTION ( 'NONE',  ( -1.000000000000000000, 3.009274222672345096E-17, 0.000000000000000000 ) ) ;
#26598 = VERTEX_POINT ( 'NONE', #35551 ) ;
#26600 = FACE_OUTER_BOUND ( 'NONE', #14515, .T. ) ;
#26599 = CIRCLE ( 'NONE', #7773, 20.00000000000000000 ) ;
#26601 = DIRECTION ( 'NONE',  ( 0.000000000000000000, 0.000000000000000000, 1.000000000000000000 ) ) ;
#26602 = CARTESIAN_POINT ( 'NONE',  ( -150.4999999999986926, -3.000858968969551636E-13, 7.000000000000042633 ) ) ;
#26603 = DIRECTION ( 'NONE',  ( 1.000000000000000000, 0.000000000000000000, 0.000000000000000000 ) ) ;
#26604 = CARTESIAN_POINT ( 'NONE',  ( -2.100000000000000089, 2.571758278209441957E-16, -5.000000000000000000 ) ) ;
#26605 = ORIENTED_EDGE ( 'NONE', *, *, #31650, .T. ) ;
#26606 = FACE_OUTER_BOUND ( 'NONE', #26470, .T. ) ;
#26607 = ORIENTED_EDGE ( 'NONE', *, *, #8735, .T. ) ;
#26608 = ADVANCED_FACE ( 'NONE', ( #5469 ), #31654, .T. ) ;
#26609 = CARTESIAN_POINT ( 'NONE',  ( 103.7695705685756877, -106.4195705685758213, 9.999999999999669598 ) ) ;
#26610 = EDGE_CURVE ( 'NONE', #39801, #11061, #31237, .T. ) ;
#26611 = CARTESIAN_POINT ( 'NONE',  ( 0.000000000000000000, -119.8996782608630838, 12.02323392193314966 ) ) ;
#26612 = ORIENTED_EDGE ( 'NONE', *, *, #5243, .F. ) ;
#26613 = FACE_BOUND ( 'NONE', #15333, .T. ) ;
#26614 = CARTESIAN_POINT ( 'NONE',  ( -103.7695705685749772, 106.4195705685765745, 7.000000000000336620 ) ) ;
#26615 = APPLICATION_PROTOCOL_DEFINITION ( 'draft international standard', 'automotive_design', 1998, #14514 ) ;
#26616 = PLANE ( 'NONE',  #17037 ) ;
#26617 = CARTESIAN_POINT ( 'NONE',  ( -66.92166868300088822, 31.00000000000000711, -22.71661802240650019 ) ) ;
#26618 = ORIENTED_EDGE ( 'NONE', *, *, #13450, .F. ) ;
#26619 = CARTESIAN_POINT ( 'NONE',  ( 19.31996883370903362, 31.00000000000000355, 33.58758284028576924 ) ) ;
#26620 = CIRCLE ( 'NONE', #40512, 116.0000000000000000 ) ;
#26621 = CARTESIAN_POINT ( 'NONE',  ( 4.417864660711233959, 40.00000000000000000, 67.39583333436242185 ) ) ;
#26622 = AXIS2_PLACEMENT_3D ( 'NONE', #28457, #4864, #37799 ) ;
#26623 = DIRECTION ( 'NONE',  ( -1.000000000000000000, 0.000000000000000000, -0.000000000000000000 ) ) ;
#26624 = DIRECTION ( 'NONE',  ( -1.000000000000000000, 0.000000000000000000, 0.000000000000000000 ) ) ;
#26625 = EDGE_CURVE ( 'NONE', #15847, #33890, #4823, .T. ) ;
#26626 = EDGE_CURVE ( 'NONE', #32160, #3569, #32323, .T. ) ;
#26627 = ADVANCED_FACE ( 'NONE', ( #21459 ), #28182, .T. ) ;
#26628 = ORIENTED_EDGE ( 'NONE', *, *, #31090, .T. ) ;
#26629 = DIRECTION ( 'NONE',  ( 1.000000000000000000, -0.000000000000000000, -0.000000000000000000 ) ) ;
#26630 = DIRECTION ( 'NONE',  ( -1.000000000000000000, 0.000000000000000000, 0.000000000000000000 ) ) ;
#26631 = PRODUCT_DEFINITION_SHAPE ( 'NONE', 'NONE',  #43184 ) ;
#26632 = EDGE_CURVE ( 'NONE', #33075, #7939, #18389, .T. ) ;
#26633 = ORIENTED_EDGE ( 'NONE', *, *, #15778, .F. ) ;
#26634 = CARTESIAN_POINT ( 'NONE',  ( 33.03432996520027132, 40.00000000000000000, -28.98482729919588863 ) ) ;
#26635 = CYLINDRICAL_SURFACE ( 'NONE', #29254, 116.0000000000000000 ) ;
#26636 = DIRECTION ( 'NONE',  ( -1.000000000000000000, -0.000000000000000000, 0.000000000000000000 ) ) ;
#26637 = VERTEX_POINT ( 'NONE', #28412 ) ;
#26638 = CARTESIAN_POINT ( 'NONE',  ( -10.00000000000000000, 0.000000000000000000, 0.000000000000000000 ) ) ;
#26639 = DIRECTION ( 'NONE',  ( 0.000000000000000000, 0.000000000000000000, 1.000000000000000000 ) ) ;
#26640 = VERTEX_POINT ( 'NONE', #41681 ) ;
#26641 = CYLINDRICAL_SURFACE ( 'NONE', #23538, 20.00000000000000711 ) ;
#26642 = ORIENTED_EDGE ( 'NONE', *, *, #19895, .T. ) ;
#26643 = CIRCLE ( 'NONE', #12031, 59.00000000000000000 ) ;
#26644 = ORIENTED_EDGE ( 'NONE', *, *, #39073, .F. ) ;
#26645 = CARTESIAN_POINT ( 'NONE',  ( 17.99999999999999645, 52.88069566989596382, -103.2454939717363516 ) ) ;
#26646 = AXIS2_PLACEMENT_3D ( 'NONE', #34286, #27546, #11188 ) ;
#26647 = EDGE_CURVE ( 'NONE', #36577, #37926, #1673, .T. ) ;
#26648 = CARTESIAN_POINT ( 'NONE',  ( -45.36921519482122278, 31.00000000000000711, 78.33339762288051134 ) ) ;
#26649 = EDGE_LOOP ( 'NONE', ( #23248, #8258, #4802, #308 ) ) ;
#26650 = DIRECTION ( 'NONE',  ( -1.000000000000000000, -0.000000000000000000, 0.000000000000000000 ) ) ;
#26651 = AXIS2_PLACEMENT_3D ( 'NONE', #8493, #15081, #8704 ) ;
#26652 = CYLINDRICAL_SURFACE ( 'NONE', #33801, 120.5010000000000190 ) ;
#26653 = DIRECTION ( 'NONE',  ( 0.000000000000000000, 0.000000000000000000, 1.000000000000000000 ) ) ;
#26654 = VERTEX_POINT ( 'NONE', #22951 ) ;
#26655 = CYLINDRICAL_SURFACE ( 'NONE', #19686, 142.5000000000000284 ) ;
#26656 = CIRCLE ( 'NONE', #16264, 59.00000000000000000 ) ;
#26657 = DIRECTION ( 'NONE',  ( 0.000000000000000000, -0.6845471059286952764, 0.7289686274214055572 ) ) ;
#26659 = CARTESIAN_POINT ( 'NONE',  ( 17.99999999999999645, 100.6739960869724655, -49.52796165323157851 ) ) ;
#26658 = FACE_OUTER_BOUND ( 'NONE', #3657, .T. ) ;
#26660 = EDGE_CURVE ( 'NONE', #39282, #43150, #7936, .T. ) ;
#26661 = DIRECTION ( 'NONE',  ( 0.000000000000000000, 0.000000000000000000, 1.000000000000000000 ) ) ;
#26662 = ORIENTED_EDGE ( 'NONE', *, *, #39347, .T. ) ;
#26663 = SHAPE_REPRESENTATION_RELATIONSHIP ( 'NONE' , 'NONE' ,  #37437, #35926 ) ;
#26664 = CARTESIAN_POINT ( 'NONE',  ( 11.86982580658625075, 31.00000000000000355, 24.05989836594520526 ) ) ;
#26665 = EDGE_LOOP ( 'NONE', ( #11714, #42303, #33440, #34301 ) ) ;
#26666 = CARTESIAN_POINT ( 'NONE',  ( 17.99999999999999645, 0.000000000000000000, 0.000000000000000000 ) ) ;
#26667 = CARTESIAN_POINT ( 'NONE',  ( 5.991980000000000750, 0.000000000000000000, 0.000000000000000000 ) ) ;
#26668 = ORIENTED_EDGE ( 'NONE', *, *, #38506, .F. ) ;
#26669 = CARTESIAN_POINT ( 'NONE',  ( 17.99999999999999645, 0.000000000000000000, 0.000000000000000000 ) ) ;
#26670 = CARTESIAN_POINT ( 'NONE',  ( -39.89583333501392559, 40.00000000000000000, 2.617993869485681468 ) ) ;
#26671 = CARTESIAN_POINT ( 'NONE',  ( 34.59698569361206211, 40.00000000000000000, -30.23997570423562209 ) ) ;
#26672 = AXIS2_PLACEMENT_3D ( 'NONE', #17465, #385, #40093 ) ;
#26673 = EDGE_LOOP ( 'NONE', ( #35084, #1097, #30490, #39017 ) ) ;
#26674 = VERTEX_POINT ( 'NONE', #36195 ) ;
#26675 =( LENGTH_UNIT ( ) NAMED_UNIT ( * ) SI_UNIT ( .MILLI., .METRE. ) );
#26676 = ADVANCED_FACE ( 'NONE', ( #29462, #29044 ), #26616, .T. ) ;
#26677 = FACE_OUTER_BOUND ( 'NONE', #36649, .T. ) ;
#26678 = AXIS2_PLACEMENT_3D ( 'NONE', #37471, #1016, #30086 ) ;
#26679 = EDGE_CURVE ( 'NONE', #20934, #31940, #31651, .T. ) ;
#26680 = DIRECTION ( 'NONE',  ( -1.000000000000000000, 0.000000000000000000, 0.000000000000000000 ) ) ;
#26681 = CARTESIAN_POINT ( 'NONE',  ( 18.00000000000000355, 13.85708833599968770, 45.43276465116669982 ) ) ;
#26682 = VERTEX_POINT ( 'NONE', #39237 ) ;
#26683 = CYLINDRICAL_SURFACE ( 'NONE', #9649, 51.99999999999999289 ) ;
#26684 = ORIENTED_EDGE ( 'NONE', *, *, #5201, .T. ) ;
#26685 = DIRECTION ( 'NONE',  ( 0.000000000000000000, -0.5264321628773627193, 0.8502171357296098853 ) ) ;
#26686 = CIRCLE ( 'NONE', #32252, 16.00000000000023448 ) ;
#26687 = CARTESIAN_POINT ( 'NONE',  ( 1.312671235360372224, 3.860931062424219462, -0.05923475698270440348 ) ) ;
#26688 = ORIENTED_EDGE ( 'NONE', *, *, #14490, .T. ) ;
#26689 = DIRECTION ( 'NONE',  ( -1.000000000000000000, -0.000000000000000000, -0.000000000000000000 ) ) ;
#26690 = CARTESIAN_POINT ( 'NONE',  ( 0.000000000000000000, 47.32430374665931794, 21.55018039121544149 ) ) ;
#26691 = ORIENTED_EDGE ( 'NONE', *, *, #41699, .F. ) ;
#26692 = DIRECTION ( 'NONE',  ( 0.000000000000000000, 0.000000000000000000, 1.000000000000000000 ) ) ;
#26693 = VERTEX_POINT ( 'NONE', #39034 ) ;
#26694 = DIRECTION ( 'NONE',  ( -1.000000000000000000, -0.000000000000000000, -0.000000000000000000 ) ) ;
#26695 = EDGE_CURVE ( 'NONE', #20680, #24669, #8623, .T. ) ;
#26696 = ORIENTED_EDGE ( 'NONE', *, *, #8443, .T. ) ;
#26698 = ORIENTED_EDGE ( 'NONE', *, *, #8884, .T. ) ;
#26697 = CARTESIAN_POINT ( 'NONE',  ( 17.99999999999999645, 115.0622509503834578, -14.72000021165029082 ) ) ;
#26699 = EDGE_CURVE ( 'NONE', #14639, #11201, #18772, .T. ) ;
#26700 = CARTESIAN_POINT ( 'NONE',  ( -38.62815422673675414, 31.00000000000000355, -50.51519254952904703 ) ) ;
#26701 = ORIENTED_EDGE ( 'NONE', *, *, #5293, .T. ) ;
#26702 = CARTESIAN_POINT ( 'NONE',  ( 2.500000000000000000, -2.629050547790028551E-15, -2.041999999999999815 ) ) ;
#26703 = ORIENTED_EDGE ( 'NONE', *, *, #9040, .F. ) ;
#26704 = FACE_OUTER_BOUND ( 'NONE', #7363, .T. ) ;
#26705 = ORIENTED_EDGE ( 'NONE', *, *, #35416, .F. ) ;
#26706 = CARTESIAN_POINT ( 'NONE',  ( 69.92891852059224789, 39.99999999999999289, 53.79372986807582180 ) ) ;
#26708 = CARTESIAN_POINT ( 'NONE',  ( 0.000000000000000000, 29.03409033315581667, 12.21509719675401051 ) ) ;
#26707 = CARTESIAN_POINT ( 'NONE',  ( 8.999999999999998224, -73.51007459736489125, 89.73443560133338792 ) ) ;
#26709 = DIRECTION ( 'NONE',  ( 0.06345332152672161774, -5.286866677681789116E-16, -0.9979848074931934043 ) ) ;
#26710 = ORIENTED_EDGE ( 'NONE', *, *, #8076, .T. ) ;
#26711 = DIRECTION ( 'NONE',  ( 0.000000000000000000, -6.586068790149233915E-15, 1.000000000000000000 ) ) ;
#26712 = STYLED_ITEM ( 'NONE', ( #14772 ), #21924 ) ;
#26713 = VERTEX_POINT ( 'NONE', #32928 ) ;
#26714 = CIRCLE ( 'NONE', #7892, 120.5010000000000332 ) ;
#26715 = CARTESIAN_POINT ( 'NONE',  ( 18.00000000000000355, -24.47917365149977798, 45.87777302070926311 ) ) ;
#26716 = CARTESIAN_POINT ( 'NONE',  ( -79.27599250299880396, 31.00000000000000711, 10.45126230984107707 ) ) ;
#26718 = DIRECTION ( 'NONE',  ( -1.000000000000000000, 0.000000000000000000, -0.000000000000000000 ) ) ;
#26717 = CARTESIAN_POINT ( 'NONE',  ( 2.500000000000000444, 0.000000000000000000, -25.03750572909317285 ) ) ;
#26719 = ORIENTED_EDGE ( 'NONE', *, *, #34716, .T. ) ;
#26720 = DIRECTION ( 'NONE',  ( 0.000000000000000000, 0.000000000000000000, 1.000000000000000000 ) ) ;
#26721 = APPLICATION_CONTEXT ( 'automotive_design' ) ;
#26722 = VERTEX_POINT ( 'NONE', #10014 ) ;
#26723 = DIRECTION ( 'NONE',  ( 1.000000000000000000, 0.000000000000000000, 0.000000000000000000 ) ) ;
#26724 = CIRCLE ( 'NONE', #18424, 120.5010000000000190 ) ;
#26725 = CARTESIAN_POINT ( 'NONE',  ( 17.99999999999999645, -6.854627147199490622, 115.7972974066013307 ) ) ;
#26726 = CARTESIAN_POINT ( 'NONE',  ( 10.50000000000000178, 0.000000000000000000, -1.199999999999999956 ) ) ;
#26727 = AXIS2_PLACEMENT_3D ( 'NONE', #5033, #25571, #15529 ) ;
#26728 = EDGE_CURVE ( 'NONE', #19290, #1072, #9159, .T. ) ;
#26729 = DIRECTION ( 'NONE',  ( -1.000000000000000000, 0.000000000000000000, 0.000000000000000000 ) ) ;
#26730 = EDGE_CURVE ( 'NONE', #6975, #40301, #39462, .T. ) ;
#26731 = AXIS2_PLACEMENT_3D ( 'NONE', #19249, #32302, #26418 ) ;
#26732 = ORIENTED_EDGE ( 'NONE', *, *, #30580, .T. ) ;
#26733 = CARTESIAN_POINT ( 'NONE',  ( 8.999999999999998224, 109.3506818544110217, 38.70953859161049593 ) ) ;
#26734 = EDGE_LOOP ( 'NONE', ( #3534, #5968, #31099, #13700 ) ) ;
#26735 = CARTESIAN_POINT ( 'NONE',  ( 0.000000000000000000, 110.3490479609629489, 20.28201389785587949 ) ) ;
#26736 = CARTESIAN_POINT ( 'NONE',  ( 22.90854556226722138, -2.055254544495723756, -74.83297477053847047 ) ) ;
#26737 = CARTESIAN_POINT ( 'NONE',  ( 0.000000000000000000, 0.000000000000000000, 0.000000000000000000 ) ) ;
#26738 = ORIENTED_EDGE ( 'NONE', *, *, #39782, .T. ) ;
#26739 = ORIENTED_EDGE ( 'NONE', *, *, #40740, .T. ) ;
#26740 = CARTESIAN_POINT ( 'NONE',  ( 18.00000000000000355, 34.03046037009255542, 33.13733193845817482 ) ) ;
#26741 = PRESENTATION_LAYER_ASSIGNMENT (  '', '', ( #17715 ) ) ;
#26742 = DIRECTION ( 'NONE',  ( -1.000000000000000000, -0.000000000000000000, -0.000000000000000000 ) ) ;
#26743 = ADVANCED_FACE ( 'NONE', ( #15956 ), #13323, .F. ) ;
#26744 = CARTESIAN_POINT ( 'NONE',  ( 2.500000000000000000, 1.178949249685212974, -2.042000000000001148 ) ) ;
#26745 = CIRCLE ( 'NONE', #13525, 59.00000000000000000 ) ;
#26747 = EDGE_LOOP ( 'NONE', ( #18750, #36652, #8615, #36075 ) ) ;
#26746 = CARTESIAN_POINT ( 'NONE',  ( -20.00000000000000000, 0.000000000000000000, -6.000000000000000000 ) ) ;
#26748 = EDGE_CURVE ( 'NONE', #13428, #3211, #12842, .T. ) ;
#26749 = CARTESIAN_POINT ( 'NONE',  ( 31.41502175087182991, 31.00000000000000355, -18.07270130326418922 ) ) ;
#26750 = DIRECTION ( 'NONE',  ( 0.000000000000000000, 0.000000000000000000, 1.000000000000000000 ) ) ;
#26752 = VERTEX_POINT ( 'NONE', #35977 ) ;
#26751 = DIRECTION ( 'NONE',  ( -1.000000000000000000, 0.000000000000000000, 0.000000000000000000 ) ) ;
#26753 = ORIENTED_EDGE ( 'NONE', *, *, #30788, .T. ) ;
#26754 = DIRECTION ( 'NONE',  ( -1.000000000000000000, -0.000000000000000000, -0.000000000000000000 ) ) ;
#26755 = DIRECTION ( 'NONE',  ( 0.000000000000000000, 0.000000000000000000, 1.000000000000000000 ) ) ;
#26756 = CARTESIAN_POINT ( 'NONE',  ( 53.62204311759386854, 40.00000000000000000, -18.10832464707264577 ) ) ;
#26757 = CARTESIAN_POINT ( 'NONE',  ( 17.99999999999999645, -78.75547124681308730, -91.20343606297076633 ) ) ;
#26758 = CARTESIAN_POINT ( 'NONE',  ( 0.000000000000000000, -45.78515115856051665, 12.64416602183649374 ) ) ;
#26759 = DIRECTION ( 'NONE',  ( -1.000000000000000000, -0.000000000000000000, 0.000000000000000000 ) ) ;
#26760 = VERTEX_POINT ( 'NONE', #26409 ) ;
#26761 = CARTESIAN_POINT ( 'NONE',  ( 17.99999999999999645, -18.35539002514308038, -110.6858262410711831 ) ) ;
#26762 = ORIENTED_EDGE ( 'NONE', *, *, #36421, .T. ) ;
#26763 = EDGE_CURVE ( 'NONE', #16394, #40591, #29535, .T. ) ;
#26764 = CARTESIAN_POINT ( 'NONE',  ( 2.500000000000000000, 2.357898499370431722, -2.818925648462311528E-15 ) ) ;
#26765 = CARTESIAN_POINT ( 'NONE',  ( 38.90854556226734218, -14.05525454449573175, -74.83297477053821467 ) ) ;
#26767 = EDGE_CURVE ( 'NONE', #31141, #13037, #23296, .T. ) ;
#26766 = CARTESIAN_POINT ( 'NONE',  ( -3.108867721649295035, 31.00000000000000355, 47.60416666525765095 ) ) ;
#26768 = LINE ( 'NONE', #13477, #7193 ) ;
#26769 = ORIENTED_EDGE ( 'NONE', *, *, #41442, .F. ) ;
#26770 = AXIS2_PLACEMENT_3D ( 'NONE', #41019, #7868, #14224 ) ;
#26771 = CARTESIAN_POINT ( 'NONE',  ( -10.00000000000000000, 0.000000000000000000, 0.000000000000000000 ) ) ;
#26772 = EDGE_LOOP ( 'NONE', ( #1996, #22233, #37403, #35527 ) ) ;
#26773 = CARTESIAN_POINT ( 'NONE',  ( -2.924622967158192921, 40.00000000000000000, -22.14664255385889291 ) ) ;
#26774 = CIRCLE ( 'NONE', #7955, 116.0000000000000000 ) ;
#26775 = EDGE_LOOP ( 'NONE', ( #40317, #11009, #19022, #1811 ) ) ;
#26776 = DIRECTION ( 'NONE',  ( -1.000000000000000000, -0.000000000000000000, 0.000000000000000000 ) ) ;
#26777 = CARTESIAN_POINT ( 'NONE',  ( -55.03444096782886419, 31.00000000000000355, -48.41538206856125015 ) ) ;
#26778 = CARTESIAN_POINT ( 'NONE',  ( -70.49178429274644486, 40.00000000000000711, 40.57739572807859929 ) ) ;
#26779 = DIRECTION ( 'NONE',  ( 0.000000000000000000, 0.000000000000000000, 1.000000000000000000 ) ) ;
#26780 = AXIS2_PLACEMENT_3D ( 'NONE', #16590, #29888, #26597 ) ;
#26781 = ADVANCED_FACE ( 'NONE', ( #36406 ), #32287, .T. ) ;
#26782 = ORIENTED_EDGE ( 'NONE', *, *, #2791, .F. ) ;
#26783 = ORIENTED_EDGE ( 'NONE', *, *, #33213, .F. ) ;
#26784 = CARTESIAN_POINT ( 'NONE',  ( -2.836893136758495970, -3.208949435745868328, -3.505054077164885484 ) ) ;
#26785 = AXIS2_PLACEMENT_3D ( 'NONE', #24126, #26515, #36960 ) ;
#26786 = CARTESIAN_POINT ( 'NONE',  ( 18.00000000000000355, 37.91532898920961969, -28.61088654061597936 ) ) ;
#26787 = DIRECTION ( 'NONE',  ( -1.000000000000000000, -0.000000000000000000, 0.000000000000000000 ) ) ;
#26788 = CIRCLE ( 'NONE', #37923, 116.0000000000000000 ) ;
#26790 = ORIENTED_EDGE ( 'NONE', *, *, #26322, .F. ) ;
#26789 = DIRECTION ( 'NONE',  ( -1.000000000000000000, -0.000000000000000000, -0.000000000000000000 ) ) ;
#26791 = CYLINDRICAL_SURFACE ( 'NONE', #30965, 59.00000000000000000 ) ;
#26792 = EDGE_LOOP ( 'NONE', ( #9341, #31750, #23955, #37359 ) ) ;
#26793 = DIRECTION ( 'NONE',  ( -1.000000000000000000, 0.000000000000000000, -0.000000000000000000 ) ) ;
#26794 = EDGE_CURVE ( 'NONE', #39040, #36371, #6516, .T. ) ;
#26795 = CIRCLE ( 'NONE', #14990, 31.49900000000000588 ) ;
#26796 = CARTESIAN_POINT ( 'NONE',  ( 64.90595555531619709, 39.99999999999999289, 56.92265028770086843 ) ) ;
#26797 = DIRECTION ( 'NONE',  ( -1.000000000000000000, 0.000000000000000000, 0.000000000000000000 ) ) ;
#26798 = ORIENTED_EDGE ( 'NONE', *, *, #40319, .T. ) ;
#26799 = LINE ( 'NONE', #30518, #20692 ) ;
#26800 = EDGE_CURVE ( 'NONE', #34203, #39186, #23983, .T. ) ;
#26801 = FACE_OUTER_BOUND ( 'NONE', #30892, .T. ) ;
#26802 = EDGE_CURVE ( 'NONE', #37957, #16711, #5139, .T. ) ;
#26803 = ORIENTED_EDGE ( 'NONE', *, *, #22970, .F. ) ;
#26804 = AXIS2_PLACEMENT_3D ( 'NONE', #33675, #3990, #23896 ) ;
#26805 = EDGE_LOOP ( 'NONE', ( #19024, #33979, #29272, #27917 ) ) ;
#26806 = CARTESIAN_POINT ( 'NONE',  ( 17.99999999999999645, 0.000000000000000000, 0.000000000000000000 ) ) ;
#26807 = EDGE_LOOP ( 'NONE', ( #16815, #18289, #660, #12455 ) ) ;
#26808 = CARTESIAN_POINT ( 'NONE',  ( 1.622176940739286310, 40.00000000000000000, -24.60292901074089045 ) ) ;
#26809 = CARTESIAN_POINT ( 'NONE',  ( 0.000000000000000000, -17.08890430202782085, 43.76671000081940122 ) ) ;
#26810 = CYLINDRICAL_SURFACE ( 'NONE', #12332, 120.5010000000000190 ) ;
#26811 = DIRECTION ( 'NONE',  ( 0.000000000000000000, 0.000000000000000000, 1.000000000000000000 ) ) ;
#26812 = CARTESIAN_POINT ( 'NONE',  ( 9.000000000000001776, 46.77034588191303754, 22.72740077717245910 ) ) ;
#26814 = ORIENTED_EDGE ( 'NONE', *, *, #15328, .F. ) ;
#26813 = AXIS2_PLACEMENT_3D ( 'NONE', #6245, #13038, #6033 ) ;
#26816 = DIRECTION ( 'NONE',  ( 1.000000000000000000, 0.000000000000000000, 0.000000000000000000 ) ) ;
#26815 = DIRECTION ( 'NONE',  ( 1.000000000000000000, 0.000000000000000000, 0.000000000000000000 ) ) ;
#26817 = VECTOR ( 'NONE', #5864, 1000.000000000000000 ) ;
#26818 = EDGE_LOOP ( 'NONE', ( #25535, #16735, #28648, #42479 ) ) ;
#26819 = AXIS2_PLACEMENT_3D ( 'NONE', #2437, #42154, #9662 ) ;
#26820 = CARTESIAN_POINT ( 'NONE',  ( 17.99999999999999645, -5.492704054965900973, -115.8698847939556771 ) ) ;
#26822 = ADVANCED_FACE ( 'NONE', ( #10459 ), #40100, .T. ) ;
#26821 = DIRECTION ( 'NONE',  ( 0.000000000000000000, 0.000000000000000000, 1.000000000000000000 ) ) ;
#26823 = EDGE_LOOP ( 'NONE', ( #17758, #8116 ) ) ;
#26824 = CARTESIAN_POINT ( 'NONE',  ( 2.500000000000000000, 2.357898499370431722, -2.818925648462311528E-15 ) ) ;
#26825 = EDGE_CURVE ( 'NONE', #384, #3752, #36474, .T. ) ;
#26826 = CARTESIAN_POINT ( 'NONE',  ( 17.99999999999999645, -21.56073507908629594, -23.57770962728587705 ) ) ;
#26827 = ITEM_DEFINED_TRANSFORMATION ( 'NONE', 'NONE', #33013,  #13552 ) ;
#26829 = AXIS2_PLACEMENT_3D ( 'NONE', #22638, #31796, #19152 ) ;
#26828 = CARTESIAN_POINT ( 'NONE',  ( 17.99999999999999645, -35.54274411428134073, 115.1399337407605259 ) ) ;
#26830 = CARTESIAN_POINT ( 'NONE',  ( 29.59587406094124873, 31.00000000000000355, 60.01321678176139329 ) ) ;
#26831 = ORIENTED_EDGE ( 'NONE', *, *, #41538, .F. ) ;
#26832 = CARTESIAN_POINT ( 'NONE',  ( -41.89947471387618805, 31.00000000000000355, 2.670153906482984674 ) ) ;
#26833 = CARTESIAN_POINT ( 'NONE',  ( -72.56464488860213180, 40.00000000000000711, -35.76892886290303863 ) ) ;
#26834 = CIRCLE ( 'NONE', #32400, 116.0000000000000000 ) ;
#26835 = EDGE_CURVE ( 'NONE', #29982, #25462, #30249, .T. ) ;
#26836 = PRESENTATION_STYLE_ASSIGNMENT (( #32572 ) ) ;
#26837 = LINE ( 'NONE', #39474, #5416 ) ;
#26838 = AXIS2_PLACEMENT_3D ( 'NONE', #42758, #13357, #12917 ) ;
#26839 = ORIENTED_EDGE ( 'NONE', *, *, #17623, .F. ) ;
#26840 = DIRECTION ( 'NONE',  ( 1.000000000000000000, -0.000000000000000000, -0.000000000000000000 ) ) ;
#26841 = CIRCLE ( 'NONE', #8026, 120.5010000000000332 ) ;
#26842 = DIRECTION ( 'NONE',  ( -3.996523416598930318E-16, 2.658563593772947863E-15, 1.000000000000000000 ) ) ;
#26843 = EDGE_CURVE ( 'NONE', #9792, #25282, #17688, .T. ) ;
#26844 = ORIENTED_EDGE ( 'NONE', *, *, #26015, .T. ) ;
#26845 = CARTESIAN_POINT ( 'NONE',  ( -48.80550277073417931, 40.00000000000000000, -13.06547612810710035 ) ) ;
#26846 = CARTESIAN_POINT ( 'NONE',  ( 17.99999999999999645, 0.000000000000000000, 0.000000000000000000 ) ) ;
#26847 = CYLINDRICAL_SURFACE ( 'NONE', #13073, 59.00000000000000000 ) ;
#26848 = AXIS2_PLACEMENT_3D ( 'NONE', #33749, #20932, #128 ) ;
#26849 = ORIENTED_EDGE ( 'NONE', *, *, #30962, .T. ) ;
#26850 = EDGE_CURVE ( 'NONE', #1556, #38673, #24015, .T. ) ;
#26851 = CARTESIAN_POINT ( 'NONE',  ( 17.99999999999999645, 0.000000000000000000, 0.000000000000000000 ) ) ;
#26852 = FACE_OUTER_BOUND ( 'NONE', #2377, .T. ) ;
#26853 = VECTOR ( 'NONE', #6637, 1000.000000000000000 ) ;
#26854 = EDGE_LOOP ( 'NONE', ( #18302, #33864, #6823, #16709 ) ) ;
#26855 = DIRECTION ( 'NONE',  ( 0.000000000000000000, 0.000000000000000000, 1.000000000000000000 ) ) ;
#26856 = ORIENTED_EDGE ( 'NONE', *, *, #15882, .T. ) ;
#26857 = AXIS2_PLACEMENT_3D ( 'NONE', #35208, #29325, #41757 ) ;
#26858 = VERTEX_POINT ( 'NONE', #7389 ) ;
#26859 = CARTESIAN_POINT ( 'NONE',  ( 17.99999999999999645, -68.61497464550522807, -99.05794392877676557 ) ) ;
#26860 = CARTESIAN_POINT ( 'NONE',  ( -92.09225407318749035, 31.00000000000000711, -6.144973693751363264 ) ) ;
#26861 = ORIENTED_EDGE ( 'NONE', *, *, #2727, .T. ) ;
#26862 = DIRECTION ( 'NONE',  ( 1.000000000000000000, 0.000000000000000000, 0.000000000000000000 ) ) ;
#26863 = CARTESIAN_POINT ( 'NONE',  ( 17.99999999999999645, -61.59243992711397198, -93.77976230226100540 ) ) ;
#26864 = DIRECTION ( 'NONE',  ( -1.000000000000000000, -0.000000000000000000, 0.000000000000000000 ) ) ;
#26865 = ORIENTED_EDGE ( 'NONE', *, *, #19268, .T. ) ;
#26866 = CARTESIAN_POINT ( 'NONE',  ( -10.00000000000000000, 0.000000000000000000, 0.000000000000000000 ) ) ;
#26867 = AXIS2_PLACEMENT_3D ( 'NONE', #3056, #39090, #42572 ) ;
#26868 = FACE_OUTER_BOUND ( 'NONE', #8949, .T. ) ;
#26869 = EDGE_CURVE ( 'NONE', #27839, #26433, #32997, .T. ) ;
#26870 = ADVANCED_FACE ( 'NONE', ( #23585 ), #37061, .F. ) ;
#26871 = VECTOR ( 'NONE', #3595, 1000.000000000000000 ) ;
#26873 = CYLINDRICAL_SURFACE ( 'NONE', #39333, 31.49899999999999878 ) ;
#26872 = DIRECTION ( 'NONE',  ( 0.000000000000000000, 0.000000000000000000, 1.000000000000000000 ) ) ;
#26874 = EDGE_CURVE ( 'NONE', #33264, #33209, #27477, .T. ) ;
#26875 = EDGE_CURVE ( 'NONE', #42811, #5127, #38572, .T. ) ;
#26876 = AXIS2_PLACEMENT_3D ( 'NONE', #27903, #25088, #8015 ) ;
#26877 = DIRECTION ( 'NONE',  ( -1.000000000000000000, 0.000000000000000000, 0.000000000000000000 ) ) ;
#26878 = AXIS2_PLACEMENT_3D ( 'NONE', #1521, #21010, #41010 ) ;
#26879 = EDGE_LOOP ( 'NONE', ( #13250, #24005 ) ) ;
#26880 = AXIS2_PLACEMENT_3D ( 'NONE', #8102, #27321, #3938 ) ;
#26881 = CARTESIAN_POINT ( 'NONE',  ( -39.12533628356670334, 31.00000000000000355, -10.47265044290268499 ) ) ;
#26882 = ORIENTED_EDGE ( 'NONE', *, *, #6605, .F. ) ;
#26883 = CIRCLE ( 'NONE', #26172, 59.00000000000000000 ) ;
#26884 = CYLINDRICAL_SURFACE ( 'NONE', #5182, 47.49900000000000233 ) ;
#26885 = AXIS2_PLACEMENT_3D ( 'NONE', #3394, #6046, #30052 ) ;
#26886 = DIRECTION ( 'NONE',  ( 3.009274222672345096E-17, 1.000000000000000000, -2.455023325076454960E-18 ) ) ;
#26887 = ORIENTED_EDGE ( 'NONE', *, *, #4999, .T. ) ;
#26888 = CIRCLE ( 'NONE', #18588, 59.00000000000000000 ) ;
#26889 = VECTOR ( 'NONE', #13227, 1000.000000000000000 ) ;
#26890 = CARTESIAN_POINT ( 'NONE',  ( 17.99999999999999645, 29.68570942776472066, 10.53307442156944873 ) ) ;
#26891 = CARTESIAN_POINT ( 'NONE',  ( 19.15075862373047144, 40.00000000000000000, -38.85840887180553693 ) ) ;
#26892 = CARTESIAN_POINT ( 'NONE',  ( 14.57966847436756019, 40.00000000000000000, -42.69519604897453036 ) ) ;
#26893 = ORIENTED_EDGE ( 'NONE', *, *, #8320, .F. ) ;
#26894 = DIRECTION ( 'NONE',  ( 0.000000000000000000, 0.000000000000000000, 1.000000000000000000 ) ) ;
#26895 = DIRECTION ( 'NONE',  ( 0.000000000000000000, 0.000000000000000000, -1.000000000000000000 ) ) ;
#26896 = LINE ( 'NONE', #23651, #20380 ) ;
#26897 = ORIENTED_EDGE ( 'NONE', *, *, #33671, .T. ) ;
#26898 = CARTESIAN_POINT ( 'NONE',  ( -20.10416666680962550, 40.00000000000000000, -1.308996940106889273 ) ) ;
#26899 = ORIENTED_EDGE ( 'NONE', *, *, #5147, .T. ) ;
#26900 = CARTESIAN_POINT ( 'NONE',  ( 17.99999999999999645, 74.56001736500617483, 88.86396238369059120 ) ) ;
#26901 = FACE_OUTER_BOUND ( 'NONE', #37245, .T. ) ;
#26902 = ORIENTED_EDGE ( 'NONE', *, *, #41839, .F. ) ;
#26903 = VECTOR ( 'NONE', #35647, 1000.000000000000000 ) ;
#26904 = DIRECTION ( 'NONE',  ( 0.000000000000000000, 0.000000000000000000, 1.000000000000000000 ) ) ;
#26905 = CARTESIAN_POINT ( 'NONE',  ( 18.00000000000000355, -0.2227391519113303131, -46.98410307550732057 ) ) ;
#26906 = ORIENTED_EDGE ( 'NONE', *, *, #6545, .T. ) ;
#26907 = FACE_OUTER_BOUND ( 'NONE', #10335, .T. ) ;
#26908 = ORIENTED_EDGE ( 'NONE', *, *, #14790, .F. ) ;
#26909 = AXIS2_PLACEMENT_3D ( 'NONE', #33774, #4303, #40522 ) ;
#26910 = CARTESIAN_POINT ( 'NONE',  ( 0.000000000000000000, -12.43843445475238063, -111.5058645182330963 ) ) ;
#26911 = VECTOR ( 'NONE', #9270, 1000.000000000000000 ) ;
#26912 = ORIENTED_EDGE ( 'NONE', *, *, #26626, .F. ) ;
#26913 = STYLED_ITEM ( 'NONE', ( #13872 ), #13741 ) ;
#26915 = EDGE_LOOP ( 'NONE', ( #38764, #9081, #6613, #1597 ) ) ;
#26914 = DIRECTION ( 'NONE',  ( 0.000000000000000000, -0.5000000000000013323, -0.8660254037844380415 ) ) ;
#26916 = CARTESIAN_POINT ( 'NONE',  ( -55.11358496760189496, 31.00000000000000711, 27.06326608205353779 ) ) ;
#26917 = ORIENTED_EDGE ( 'NONE', *, *, #2029, .F. ) ;
#26918 = DIRECTION ( 'NONE',  ( 0.000000000000000000, 0.000000000000000000, 1.000000000000000000 ) ) ;
#26919 = AXIS2_PLACEMENT_3D ( 'NONE', #27097, #30587, #6994 ) ;
#26920 = EDGE_LOOP ( 'NONE', ( #42300, #10760, #17476 ) ) ;
#26921 = CARTESIAN_POINT ( 'NONE',  ( 8.999999999999998224, -24.70533337038242294, 26.18485254986683586 ) ) ;
#26922 = CIRCLE ( 'NONE', #23458, 13.59999999999999964 ) ;
#26923 = VERTEX_POINT ( 'NONE', #30545 ) ;
#26924 = CARTESIAN_POINT ( 'NONE',  ( -41.82916961767931951, 40.00000000000000000, -72.66191475361131324 ) ) ;
#26926 = DIRECTION ( 'NONE',  ( 0.000000000000000000, -0.9213119778704086382, -0.3888241754733309241 ) ) ;
#26925 = LINE ( 'NONE', #40205, #17569 ) ;
#26927 = ADVANCED_FACE ( 'NONE', ( #13968 ), #24009, .F. ) ;
#26928 = EDGE_CURVE ( 'NONE', #28542, #6200, #3660, .T. ) ;
#26929 = CARTESIAN_POINT ( 'NONE',  ( 0.000000000000000000, 5.667686777402355602, -46.64153600743599526 ) ) ;
#26930 = ORIENTED_EDGE ( 'NONE', *, *, #15351, .T. ) ;
#26931 = LINE ( 'NONE', #20201, #24498 ) ;
#26932 = ORIENTED_EDGE ( 'NONE', *, *, #16069, .T. ) ;
#26933 = EDGE_CURVE ( 'NONE', #5383, #40193, #35783, .T. ) ;
#26934 = DIRECTION ( 'NONE',  ( 0.000000000000000000, -0.9957341762950334685, -0.09226835946331299332 ) ) ;
#26935 = DIRECTION ( 'NONE',  ( 0.000000000000000000, 0.000000000000000000, 1.000000000000000000 ) ) ;
#26936 = CARTESIAN_POINT ( 'NONE',  ( -29.64342647699677613, 31.00000000000000355, -87.27882330658468391 ) ) ;
#26937 = CYLINDRICAL_SURFACE ( 'NONE', #29735, 59.00000000000000000 ) ;
#26938 = AXIS2_PLACEMENT_3D ( 'NONE', #38020, #27812, #41063 ) ;
#26939 = ORIENTED_EDGE ( 'NONE', *, *, #16250, .F. ) ;
#26940 = AXIS2_PLACEMENT_3D ( 'NONE', #29289, #35167, #25818 ) ;
#26941 = AXIS2_PLACEMENT_3D ( 'NONE', #35695, #42030, #32028 ) ;
#26942 = CIRCLE ( 'NONE', #17226, 10.49999999999999467 ) ;
#26943 = CARTESIAN_POINT ( 'NONE',  ( 0.000000000000000000, -96.25468616236614139, -72.49500943364587613 ) ) ;
#26944 = AXIS2_PLACEMENT_3D ( 'NONE', #10732, #21033, #886 ) ;
#26945 = ADVANCED_FACE ( 'NONE', ( #30318 ), #20750, .F. ) ;
#26946 = ORIENTED_EDGE ( 'NONE', *, *, #10792, .T. ) ;
#26947 = CARTESIAN_POINT ( 'NONE',  ( 17.99999999999999645, 103.4151313792870610, 61.85306461934443689 ) ) ;
#26948 = CARTESIAN_POINT ( 'NONE',  ( 17.99999999999999645, 0.000000000000000000, 0.000000000000000000 ) ) ;
#26949 = CARTESIAN_POINT ( 'NONE',  ( -50.38378093998269946, 31.00000000000000711, 87.00968337440518496 ) ) ;
#26950 = AXIS2_PLACEMENT_3D ( 'NONE', #31357, #42005, #18516 ) ;
#26951 = CARTESIAN_POINT ( 'NONE',  ( 18.00000000000000355, -2.123073309835499245, 47.45152853935333326 ) ) ;
#26952 = CIRCLE ( 'NONE', #8138, 120.5010000000000190 ) ;
#26953 = EDGE_LOOP ( 'NONE', ( #30029, #992, #1776 ) ) ;
#26954 = DIRECTION ( 'NONE',  ( -1.000000000000000000, -0.000000000000000000, -0.000000000000000000 ) ) ;
#26955 = EDGE_LOOP ( 'NONE', ( #33059, #33977, #14996, #41086 ) ) ;
#26956 = CYLINDRICAL_SURFACE ( 'NONE', #25608, 36.00000000000000000 ) ;
#26957 = VECTOR ( 'NONE', #9255, 1000.000000000000000 ) ;
#26958 = CIRCLE ( 'NONE', #27660, 13.60000000000000320 ) ;
#26959 = CARTESIAN_POINT ( 'NONE',  ( 21.00000000000000355, 0.000000000000000000, 0.000000000000000000 ) ) ;
#26960 = DIRECTION ( 'NONE',  ( -1.000000000000000000, 0.000000000000000000, 0.000000000000000000 ) ) ;
#26961 = ORIENTED_EDGE ( 'NONE', *, *, #2796, .T. ) ;
#26962 = EDGE_CURVE ( 'NONE', #13115, #19749, #25388, .T. ) ;
#26963 = EDGE_LOOP ( 'NONE', ( #34803, #23540, #40663, #36176 ) ) ;
#26964 = LINE ( 'NONE', #26740, #20325 ) ;
#26965 = DIRECTION ( 'NONE',  ( 0.000000000000000000, 0.9911528310040066403, 0.1327255272837255529 ) ) ;
#26966 = FACE_OUTER_BOUND ( 'NONE', #40802, .T. ) ;
#26968 = EDGE_LOOP ( 'NONE', ( #29156, #3958, #28641, #25959 ) ) ;
#26967 = CARTESIAN_POINT ( 'NONE',  ( -6.075999999999997847, 2.346238345499656945E-15, -19.11697999999999809 ) ) ;
#26969 = CARTESIAN_POINT ( 'NONE',  ( 3.798394181603659270, 31.00000000000000355, 29.10671710469610574 ) ) ;
#26970 = DIRECTION ( 'NONE',  ( -1.000000000000000000, 0.000000000000000000, 0.000000000000000000 ) ) ;
#26971 = AXIS2_PLACEMENT_3D ( 'NONE', #23546, #20070, #33335 ) ;
#26972 = AXIS2_PLACEMENT_3D ( 'NONE', #35194, #15176, #18687 ) ;
#26974 = ORIENTED_EDGE ( 'NONE', *, *, #26647, .F. ) ;
#26973 = CYLINDRICAL_SURFACE ( 'NONE', #36303, 59.00000000000000000 ) ;
#26975 = UNCERTAINTY_MEASURE_WITH_UNIT (LENGTH_MEASURE( 1.000000000000000082E-05 ), #12825, 'distance_accuracy_value', 'NONE');
#26976 = ORIENTED_EDGE ( 'NONE', *, *, #34246, .F. ) ;
#26977 = CARTESIAN_POINT ( 'NONE',  ( 2.500000000000000000, -1.178949249685214307, 2.042000000000001592 ) ) ;
#26978 = DIRECTION ( 'NONE',  ( 1.000000000000000000, 0.000000000000000000, 0.000000000000000000 ) ) ;
#26979 = CARTESIAN_POINT ( 'NONE',  ( 51.84393115708665079, 40.00000000000000000, 25.66707601012906537 ) ) ;
#26980 = AXIS2_PLACEMENT_3D ( 'NONE', #18837, #1548, #18404 ) ;
#26981 = VECTOR ( 'NONE', #7296, 1000.000000000000000 ) ;
#26982 = AXIS2_PLACEMENT_3D ( 'NONE', #18696, #31954, #2038 ) ;
#26983 = CARTESIAN_POINT ( 'NONE',  ( 38.90854556226734218, -12.05525454449572464, -74.83297477053821467 ) ) ;
#26984 = UNCERTAINTY_MEASURE_WITH_UNIT (LENGTH_MEASURE( 1.000000000000000082E-05 ), #211, 'distance_accuracy_value', 'NONE');
#26985 = EDGE_CURVE ( 'NONE', #28381, #12448, #12142, .T. ) ;
#26986 = CARTESIAN_POINT ( 'NONE',  ( 17.99999999999999645, -13.00789606333398218, -115.2683592318616235 ) ) ;
#26987 = ORIENTED_EDGE ( 'NONE', *, *, #15485, .T. ) ;
#26988 = CARTESIAN_POINT ( 'NONE',  ( 2.500000000000000000, 0.000000000000000000, 2.041999999999999815 ) ) ;
#26990 = ORIENTED_EDGE ( 'NONE', *, *, #26438, .T. ) ;
#26989 = CIRCLE ( 'NONE', #34631, 31.49899999999999523 ) ;
#26991 = CARTESIAN_POINT ( 'NONE',  ( 17.99999999999999645, 0.000000000000000000, 0.000000000000000000 ) ) ;
#26992 = CARTESIAN_POINT ( 'NONE',  ( 0.000000000000000000, 3.996885678773001604, 120.4346956066682282 ) ) ;
#26993 = AXIS2_PLACEMENT_3D ( 'NONE', #21715, #24337, #1799 ) ;
#26994 = CARTESIAN_POINT ( 'NONE',  ( -44.28363997456384737, 31.00000000000000355, 21.84072794957603492 ) ) ;
#26995 = CARTESIAN_POINT ( 'NONE',  ( -12.69999999999999929, 0.000000000000000000, 0.000000000000000000 ) ) ;
#26996 = ORIENTED_EDGE ( 'NONE', *, *, #38520, .F. ) ;
#26997 = EDGE_CURVE ( 'NONE', #3495, #16072, #3762, .T. ) ;
#26998 = EDGE_CURVE ( 'NONE', #24964, #29204, #23794, .T. ) ;
#26999 = PRODUCT_DEFINITION_SHAPE ( 'NONE', 'NONE',  #37893 ) ;
#27000 = DIRECTION ( 'NONE',  ( -1.000000000000000000, -0.000000000000000000, 0.000000000000000000 ) ) ;
#27001 = VERTEX_POINT ( 'NONE', #10901 ) ;
#27002 = CARTESIAN_POINT ( 'NONE',  ( 1.472621547668719444, 40.00000000000000000, -22.60416666365413718 ) ) ;
#27003 = ADVANCED_FACE ( 'NONE', ( #5419 ), #34872, .F. ) ;
#27004 = ORIENTED_EDGE ( 'NONE', *, *, #39889, .F. ) ;
#27005 = FACE_OUTER_BOUND ( 'NONE', #3153, .T. ) ;
#27006 = FACE_OUTER_BOUND ( 'NONE', #8864, .T. ) ;
#27007 = VECTOR ( 'NONE', #21538, 1000.000000000000000 ) ;
#27008 = CARTESIAN_POINT ( 'NONE',  ( -70.06919973877657526, 31.00000000000000711, -18.87919424805730984 ) ) ;
#27009 = CARTESIAN_POINT ( 'NONE',  ( 66.15140951845482675, 39.99999999999999289, -38.07406969931857077 ) ) ;
#27010 = CARTESIAN_POINT ( 'NONE',  ( 17.99999999999999645, -107.5680526044917542, -31.89649718262205269 ) ) ;
#27011 = VECTOR ( 'NONE', #8529, 1000.000000000000000 ) ;
#27012 = AXIS2_PLACEMENT_3D ( 'NONE', #17553, #14482, #10986 ) ;
#27013 = ORIENTED_EDGE ( 'NONE', *, *, #12932, .F. ) ;
#27014 = CARTESIAN_POINT ( 'NONE',  ( 9.000000000000001776, -108.8880088604273766, -39.99251838046072294 ) ) ;
#27015 = VERTEX_POINT ( 'NONE', #41630 ) ;
#27016 = CIRCLE ( 'NONE', #22154, 13.59999999999999964 ) ;
#27017 = DIRECTION ( 'NONE',  ( 0.000000000000000000, 0.000000000000000000, 1.000000000000000000 ) ) ;
#27018 = VECTOR ( 'NONE', #9455, 1000.000000000000000 ) ;
#27019 = LINE ( 'NONE', #14147, #40742 ) ;
#27021 = EDGE_LOOP ( 'NONE', ( #13567, #13352, #328, #7117 ) ) ;
#27020 = DIRECTION ( 'NONE',  ( -1.000000000000000000, -0.000000000000000000, -0.000000000000000000 ) ) ;
#27022 = CARTESIAN_POINT ( 'NONE',  ( 0.000000000000000000, 0.000000000000000000, 0.000000000000000000 ) ) ;
#27023 = ORIENTED_EDGE ( 'NONE', *, *, #13345, .F. ) ;
#27024 = DIRECTION ( 'NONE',  ( -1.000000000000000000, 0.000000000000000000, -0.000000000000000000 ) ) ;
#27025 = EDGE_CURVE ( 'NONE', #39668, #18842, #1917, .T. ) ;
#27026 = CARTESIAN_POINT ( 'NONE',  ( 84.66040299356156140, 39.99999999999999289, 11.14692016787551765 ) ) ;
#27027 = DIRECTION ( 'NONE',  ( -1.000000000000000000, -0.000000000000000000, 0.000000000000000000 ) ) ;
#27028 = EDGE_CURVE ( 'NONE', #31846, #32645, #28132, .T. ) ;
#27029 = CIRCLE ( 'NONE', #42344, 59.00000000000000000 ) ;
#27030 = ORIENTED_EDGE ( 'NONE', *, *, #5461, .T. ) ;
#27031 = LINE ( 'NONE', #27236, #41508 ) ;
#27032 = EDGE_CURVE ( 'NONE', #13484, #5383, #18559, .T. ) ;
#27033 = CARTESIAN_POINT ( 'NONE',  ( 8.999999999999998224, -86.84764344323014029, 76.89919913989720612 ) ) ;
#27034 = VERTEX_POINT ( 'NONE', #38556 ) ;
#27035 = SURFACE_SIDE_STYLE ('',( #20727 ) ) ;
#27036 = VERTEX_POINT ( 'NONE', #35079 ) ;
#27037 = DIRECTION ( 'NONE',  ( -1.000000000000000000, 0.000000000000000000, 0.000000000000000000 ) ) ;
#27038 = ORIENTED_EDGE ( 'NONE', *, *, #3995, .T. ) ;
#27039 = CARTESIAN_POINT ( 'NONE',  ( 27.10182830755125138, 40.00000000000000000, 1.799748011963437255 ) ) ;
#27040 = CARTESIAN_POINT ( 'NONE',  ( 17.99999999999999645, 0.000000000000000000, 0.000000000000000000 ) ) ;
#27041 = FACE_OUTER_BOUND ( 'NONE', #15342, .T. ) ;
#27042 = CARTESIAN_POINT ( 'NONE',  ( 5.384454397937118664, 0.000000000000000000, -5.000000000000000000 ) ) ;
#27043 = CARTESIAN_POINT ( 'NONE',  ( 17.99999999999999645, 40.37724737310206535, -104.6802291180863023 ) ) ;
#27044 = ORIENTED_EDGE ( 'NONE', *, *, #27471, .T. ) ;
#27045 = CIRCLE ( 'NONE', #25663, 120.5010000000000474 ) ;
#27047 = CARTESIAN_POINT ( 'NONE',  ( 17.99999999999999645, 0.000000000000000000, 0.000000000000000000 ) ) ;
#27046 = CARTESIAN_POINT ( 'NONE',  ( 0.000000000000000000, -29.86146781000025285, 112.0905559814577970 ) ) ;
#27048 = EDGE_CURVE ( 'NONE', #31862, #959, #15486, .T. ) ;
#27049 = CIRCLE ( 'NONE', #40241, 120.5010000000000190 ) ;
#27050 = ORIENTED_EDGE ( 'NONE', *, *, #8506, .F. ) ;
#27051 = AXIS2_PLACEMENT_3D ( 'NONE', #286, #26954, #9504 ) ;
#27052 = DIRECTION ( 'NONE',  ( 0.000000000000000000, 0.000000000000000000, 1.000000000000000000 ) ) ;
#27053 = CARTESIAN_POINT ( 'NONE',  ( 23.00000000000000000, 2.816687638038912352E-15, -6.000000000000000000 ) ) ;
#27054 = ORIENTED_EDGE ( 'NONE', *, *, #4857, .F. ) ;
#27055 = LINE ( 'NONE', #20104, #22541 ) ;
#27056 = AXIS2_PLACEMENT_3D ( 'NONE', #15976, #36211, #19046 ) ;
#27057 = DIRECTION ( 'NONE',  ( 0.000000000000000000, 0.000000000000000000, 1.000000000000000000 ) ) ;
#27058 = EDGE_CURVE ( 'NONE', #1072, #41904, #9364, .T. ) ;
#27059 = DIRECTION ( 'NONE',  ( -1.000000000000000000, 0.000000000000000000, 0.000000000000000000 ) ) ;
#27060 = CARTESIAN_POINT ( 'NONE',  ( 21.58803501788969115, 31.00000000000000355, 63.55567069162312777 ) ) ;
#27061 = EDGE_LOOP ( 'NONE', ( #27347, #21759, #8600, #3688 ) ) ;
#27062 = CARTESIAN_POINT ( 'NONE',  ( 24.31498657912377226, 31.00000000000000355, 42.27453502171529465 ) ) ;
#27063 = CARTESIAN_POINT ( 'NONE',  ( -20.19574676229028043, 40.00000000000000000, 75.42596061005518493 ) ) ;
#27064 = CARTESIAN_POINT ( 'NONE',  ( -2.797566391619251075E-15, 1.860994515641065082E-14, 7.000000000000002665 ) ) ;
#27065 = DIRECTION ( 'NONE',  ( 0.000000000000000000, -2.140472356798500845E-14, -1.000000000000000000 ) ) ;
#27066 = AXIS2_PLACEMENT_3D ( 'NONE', #1561, #7681, #24526 ) ;
#27067 = AXIS2_PLACEMENT_3D ( 'NONE', #30337, #40342, #39479 ) ;
#27068 = EDGE_LOOP ( 'NONE', ( #18479, #35122 ) ) ;
#27069 = CARTESIAN_POINT ( 'NONE',  ( 18.00000000000000355, 0.000000000000000000, 0.000000000000000000 ) ) ;
#27070 = DIRECTION ( 'NONE',  ( -1.000000000000000000, -0.000000000000000000, 0.000000000000000000 ) ) ;
#27071 = VERTEX_POINT ( 'NONE', #4986 ) ;
#27072 = CARTESIAN_POINT ( 'NONE',  ( -56.43872490705654599, 40.00000000000000711, 19.17141758012168751 ) ) ;
#27073 = CYLINDRICAL_SURFACE ( 'NONE', #38294, 19.99999999999989342 ) ;
#27075 = ADVANCED_FACE ( 'NONE', ( #41183 ), #12197, .T. ) ;
#27074 = CARTESIAN_POINT ( 'NONE',  ( 0.000000000000000000, 0.000000000000000000, 0.000000000000000000 ) ) ;
#27076 = AXIS2_PLACEMENT_3D ( 'NONE', #16240, #5955, #39314 ) ;
#27077 = ORIENTED_EDGE ( 'NONE', *, *, #25179, .T. ) ;
#27078 = EDGE_CURVE ( 'NONE', #34811, #21374, #26788, .T. ) ;
#27079 = DIRECTION ( 'NONE',  ( -1.000000000000000000, -0.000000000000000000, 0.000000000000000000 ) ) ;
#27080 = CIRCLE ( 'NONE', #34728, 20.00000000000000711 ) ;
#27081 = CYLINDRICAL_SURFACE ( 'NONE', #22243, 116.0000000000000000 ) ;
#27082 = ORIENTED_EDGE ( 'NONE', *, *, #21108, .F. ) ;
#27083 = DIRECTION ( 'NONE',  ( -1.000000000000000000, 0.000000000000000000, 0.000000000000000000 ) ) ;
#27084 = VERTEX_POINT ( 'NONE', #37919 ) ;
#27085 = DIRECTION ( 'NONE',  ( -1.000000000000000000, 0.000000000000000000, 0.000000000000000000 ) ) ;
#27086 = ORIENTED_EDGE ( 'NONE', *, *, #21476, .T. ) ;
#27087 = CARTESIAN_POINT ( 'NONE',  ( 0.000000000000000000, -21.55123232222391394, -118.5581519187674360 ) ) ;
#27088 = CARTESIAN_POINT ( 'NONE',  ( 12.51314706078824912, 31.00000000000000355, -94.07914177284597201 ) ) ;
#27089 = ORIENTED_EDGE ( 'NONE', *, *, #36751, .T. ) ;
#27090 = CARTESIAN_POINT ( 'NONE',  ( 17.99999999999999645, 0.000000000000000000, 0.000000000000000000 ) ) ;
#27091 = EDGE_CURVE ( 'NONE', #10543, #5501, #11483, .T. ) ;
#27092 = DIRECTION ( 'NONE',  ( 0.000000000000000000, 0.000000000000000000, 1.000000000000000000 ) ) ;
#27093 = DIRECTION ( 'NONE',  ( 0.000000000000000000, 1.000000000000000000, -1.060184893785364939E-15 ) ) ;
#27094 = VERTEX_POINT ( 'NONE', #8039 ) ;
#27095 = DIRECTION ( 'NONE',  ( 0.000000000000000000, 0.000000000000000000, -1.000000000000000000 ) ) ;
#27096 = EDGE_CURVE ( 'NONE', #4115, #8700, #20559, .T. ) ;
#27097 = CARTESIAN_POINT ( 'NONE',  ( 0.000000000000000000, 5.919241748380035695, -31.39643714728450163 ) ) ;
#27098 = AXIS2_PLACEMENT_3D ( 'NONE', #8290, #9515, #29824 ) ;
#27099 = CIRCLE ( 'NONE', #36100, 120.5010000000000332 ) ;
#27101 = CYLINDRICAL_SURFACE ( 'NONE', #3791, 10.50000000000000178 ) ;
#27100 = CARTESIAN_POINT ( 'NONE',  ( 0.000000000000000000, -46.83041522348427321, -101.9567785075606139 ) ) ;
#27102 = FACE_OUTER_BOUND ( 'NONE', #1950, .T. ) ;
#27103 = VECTOR ( 'NONE', #22371, 1000.000000000000000 ) ;
#27104 = ORIENTED_EDGE ( 'NONE', *, *, #19082, .T. ) ;
#27105 = DIRECTION ( 'NONE',  ( -6.982962677686266711E-15, 0.000000000000000000, -1.000000000000000000 ) ) ;
#27106 = EDGE_CURVE ( 'NONE', #12490, #37365, #27482, .T. ) ;
#27107 = CARTESIAN_POINT ( 'NONE',  ( 17.99999999999999645, -35.89808275599447285, 2.706964063997103764 ) ) ;
#27108 = CARTESIAN_POINT ( 'NONE',  ( 11.12085686420672381, 31.00000000000000355, -41.54537790535560760 ) ) ;
#27109 = VERTEX_POINT ( 'NONE', #11549 ) ;
#27110 = FACE_OUTER_BOUND ( 'NONE', #20891, .T. ) ;
#27111 = EDGE_CURVE ( 'NONE', #19328, #14493, #33753, .T. ) ;
#27112 = CARTESIAN_POINT ( 'NONE',  ( -105.3367680159044966, 31.00000000000000355, 2.032994142711224583 ) ) ;
#27113 = ORIENTED_EDGE ( 'NONE', *, *, #39490, .T. ) ;
#27114 = CIRCLE ( 'NONE', #36983, 31.49900000000000233 ) ;
#27115 = DIRECTION ( 'NONE',  ( -1.000000000000000000, -0.000000000000000000, -0.000000000000000000 ) ) ;
#27116 = CARTESIAN_POINT ( 'NONE',  ( 34.77048308403384169, 40.00000000000000000, 30.48958026498159768 ) ) ;
#27117 = CARTESIAN_POINT ( 'NONE',  ( 2.996940313443920978, 40.00000000000000000, -44.59688583547568896 ) ) ;
#27118 = EDGE_LOOP ( 'NONE', ( #14384, #39228, #38479, #30059 ) ) ;
#27119 = DIRECTION ( 'NONE',  ( 0.000000000000000000, -0.9048270524660145808, -0.4257792915650832066 ) ) ;
#27120 = CARTESIAN_POINT ( 'NONE',  ( 5.200000000000002842, 0.000000000000000000, 0.000000000000000000 ) ) ;
#27121 = DIRECTION ( 'NONE',  ( 1.000000000000000000, 0.000000000000000000, 0.000000000000000000 ) ) ;
#27122 = VERTEX_POINT ( 'NONE', #18134 ) ;
#27123 = CARTESIAN_POINT ( 'NONE',  ( 23.22631124480444598, 40.00000000000000000, -7.893869537065737241 ) ) ;
#27124 = VERTEX_POINT ( 'NONE', #8269 ) ;
#27125 = DIRECTION ( 'NONE',  ( -1.000000000000000000, 0.000000000000000000, 0.000000000000000000 ) ) ;
#27126 = DIRECTION ( 'NONE',  ( 3.009274222672345096E-17, 1.000000000000000000, -2.455023325076454960E-18 ) ) ;
#27127 = EDGE_CURVE ( 'NONE', #29868, #40246, #12878, .T. ) ;
#27128 = ORIENTED_EDGE ( 'NONE', *, *, #18220, .F. ) ;
#27130 = EDGE_CURVE ( 'NONE', #41070, #13955, #35298, .T. ) ;
#27129 = CIRCLE ( 'NONE', #4103, 20.00000000000000711 ) ;
#27131 = AXIS2_PLACEMENT_3D ( 'NONE', #19156, #12167, #25488 ) ;
#27132 = CARTESIAN_POINT ( 'NONE',  ( -9.000000000000007105, 0.000000000000000000, 0.000000000000000000 ) ) ;
#27133 = EDGE_CURVE ( 'NONE', #6470, #8854, #18785, .T. ) ;
#27134 = EDGE_CURVE ( 'NONE', #37442, #29982, #34311, .T. ) ;
#27135 = CARTESIAN_POINT ( 'NONE',  ( 9.000000000000001776, 49.25004636492411692, -16.68630974939707556 ) ) ;
#27136 = ORIENTED_EDGE ( 'NONE', *, *, #9037, .T. ) ;
#27137 = DIRECTION ( 'NONE',  ( -1.000000000000000000, 0.000000000000000000, -0.000000000000000000 ) ) ;
#27138 = VERTEX_POINT ( 'NONE', #39626 ) ;
#27139 = CIRCLE ( 'NONE', #18828, 51.99999999999999289 ) ;
#27140 = DIRECTION ( 'NONE',  ( -1.000000000000000000, -0.000000000000000000, -0.000000000000000000 ) ) ;
#27141 = VERTEX_POINT ( 'NONE', #12620 ) ;
#27143 = ORIENTED_EDGE ( 'NONE', *, *, #27560, .F. ) ;
#27142 = CARTESIAN_POINT ( 'NONE',  ( 0.2142857142857142738, -10.49781318335647917, 0.000000000000000000 ) ) ;
#27144 = CARTESIAN_POINT ( 'NONE',  ( -4.113979049837550583, 31.00000000000000355, -64.40000927351897531 ) ) ;
#27145 = VERTEX_POINT ( 'NONE', #43119 ) ;
#27146 = LINE ( 'NONE', #29771, #11937 ) ;
#27147 = ORIENTED_EDGE ( 'NONE', *, *, #6249, .F. ) ;
#27148 = FACE_BOUND ( 'NONE', #7325, .T. ) ;
#27149 = VERTEX_POINT ( 'NONE', #25521 ) ;
#27150 = CARTESIAN_POINT ( 'NONE',  ( -53.37462671635322664, 40.00000000000000711, 60.68184199298008252 ) ) ;
#27152 = DIRECTION ( 'NONE',  ( 1.000000000000000000, -0.000000000000000000, -0.000000000000000000 ) ) ;
#27151 = DIRECTION ( 'NONE',  ( -1.000000000000000000, 0.000000000000000000, 0.000000000000000000 ) ) ;
#27153 = DIRECTION ( 'NONE',  ( -1.000000000000000000, 0.000000000000000000, 0.000000000000000000 ) ) ;
#27154 = ORIENTED_EDGE ( 'NONE', *, *, #32054, .F. ) ;
#27155 = DIRECTION ( 'NONE',  ( 1.000000000000000000, 0.000000000000000000, 0.000000000000000000 ) ) ;
#27156 = VERTEX_POINT ( 'NONE', #18987 ) ;
#27157 = EDGE_CURVE ( 'NONE', #17321, #16407, #24743, .T. ) ;
#27158 = CARTESIAN_POINT ( 'NONE',  ( 9.000000000000000000, -13.57797752207901532, -33.34124362422488730 ) ) ;
#27159 = CIRCLE ( 'NONE', #18912, 10.99999999999998934 ) ;
#27160 = ORIENTED_EDGE ( 'NONE', *, *, #23679, .F. ) ;
#27161 = CARTESIAN_POINT ( 'NONE',  ( -15.99999999999997691, 31.00000000000000355, 2.500000000000006217 ) ) ;
#27162 = CARTESIAN_POINT ( 'NONE',  ( -81.55297449308174862, 31.00000000000000711, -40.20044092665353475 ) ) ;
#27163 = AXIS2_PLACEMENT_3D ( 'NONE', #38698, #22178, #23026 ) ;
#27164 = CARTESIAN_POINT ( 'NONE',  ( 0.000000000000000000, -2.357898499370432166, 3.035766082959412415E-15 ) ) ;
#27165 = VERTEX_POINT ( 'NONE', #6052 ) ;
#27166 = CARTESIAN_POINT ( 'NONE',  ( 0.000000000000000000, 28.35267316522783432, 22.18391138608718549 ) ) ;
#27167 = ORIENTED_EDGE ( 'NONE', *, *, #41687, .F. ) ;
#27168 = SURFACE_SIDE_STYLE ('',( #40642 ) ) ;
#27169 = LINE ( 'NONE', #39580, #38077 ) ;
#27170 =( NAMED_UNIT ( * ) SI_UNIT ( $, .STERADIAN. ) SOLID_ANGLE_UNIT ( ) );
#27171 = CYLINDRICAL_SURFACE ( 'NONE', #24011, 59.00000000000000000 ) ;
#27172 = VERTEX_POINT ( 'NONE', #32877 ) ;
#27173 = FACE_OUTER_BOUND ( 'NONE', #22468, .T. ) ;
#27174 = ORIENTED_EDGE ( 'NONE', *, *, #4760, .F. ) ;
#27175 = FACE_OUTER_BOUND ( 'NONE', #24854, .T. ) ;
#27176 = DIRECTION ( 'NONE',  ( 0.000000000000000000, 0.000000000000000000, 1.000000000000000000 ) ) ;
#27177 = ADVANCED_FACE ( 'NONE', ( #16113 ), #42259, .F. ) ;
#27178 = EDGE_CURVE ( 'NONE', #9970, #41689, #15686, .T. ) ;
#27179 = CYLINDRICAL_SURFACE ( 'NONE', #39342, 31.49899999999999878 ) ;
#27180 = ORIENTED_EDGE ( 'NONE', *, *, #24045, .F. ) ;
#27181 = VERTEX_POINT ( 'NONE', #32670 ) ;
#27182 = DIRECTION ( 'NONE',  ( 1.000000000000000000, 0.000000000000000000, -6.546126324440847704E-16 ) ) ;
#27183 = DIRECTION ( 'NONE',  ( -1.000000000000000000, 0.000000000000000000, 0.000000000000000000 ) ) ;
#27184 = EDGE_CURVE ( 'NONE', #39162, #5150, #17068, .T. ) ;
#27185 = CARTESIAN_POINT ( 'NONE',  ( 17.99999999999999645, -96.25468616236614139, -72.49500943364587613 ) ) ;
#27186 = AXIS2_PLACEMENT_3D ( 'NONE', #25642, #2439, #38900 ) ;
#27188 = ORIENTED_EDGE ( 'NONE', *, *, #15058, .T. ) ;
#27187 = CARTESIAN_POINT ( 'NONE',  ( 9.000000000000001776, 7.162210897276454880, -51.50439529848819831 ) ) ;
#27189 = CIRCLE ( 'NONE', #18167, 20.00000000000000355 ) ;
#27190 = CARTESIAN_POINT ( 'NONE',  ( -4.434938641671373638, 31.00000000000000355, -34.07637162043106116 ) ) ;
#27191 = AXIS2_PLACEMENT_3D ( 'NONE', #8129, #41051, #34306 ) ;
#27192 = CARTESIAN_POINT ( 'NONE',  ( 0.000000000000000000, -59.07817985939071548, 105.0250430397506847 ) ) ;
#27194 = VERTEX_POINT ( 'NONE', #9753 ) ;
#27193 = CARTESIAN_POINT ( 'NONE',  ( 17.99999999999999645, 0.000000000000000000, 0.000000000000000000 ) ) ;
#27195 = ORIENTED_EDGE ( 'NONE', *, *, #35282, .F. ) ;
#27196 = FACE_OUTER_BOUND ( 'NONE', #21480, .T. ) ;
#27197 = CARTESIAN_POINT ( 'NONE',  ( -49.95450512539639476, 40.00000000000000000, 13.28959769214884545 ) ) ;
#27198 = EDGE_CURVE ( 'NONE', #41379, #7422, #21260, .T. ) ;
#27199 = CARTESIAN_POINT ( 'NONE',  ( 17.99999999999999645, 0.000000000000000000, 0.000000000000000000 ) ) ;
#27200 = CARTESIAN_POINT ( 'NONE',  ( 0.000000000000000000, 87.92975456462900752, 69.68953103478187927 ) ) ;
#27201 = EDGE_LOOP ( 'NONE', ( #5651, #8004, #28188, #13221 ) ) ;
#27202 = DIRECTION ( 'NONE',  ( -1.000000000000000000, 0.000000000000000000, 0.000000000000000000 ) ) ;
#27203 = ORIENTED_EDGE ( 'NONE', *, *, #25085, .F. ) ;
#27204 = CARTESIAN_POINT ( 'NONE',  ( 0.000000000000000000, -17.33727698085246871, 110.8498592715972961 ) ) ;
#27205 = CARTESIAN_POINT ( 'NONE',  ( 17.99999999999999645, 0.000000000000000000, 0.000000000000000000 ) ) ;
#27206 = AXIS2_PLACEMENT_3D ( 'NONE', #4585, #31444, #30794 ) ;
#27207 = CARTESIAN_POINT ( 'NONE',  ( 42.30435120181500963, 31.00000000000000355, 37.09784777058769123 ) ) ;
#27208 = DIRECTION ( 'NONE',  ( -1.000000000000000000, 0.000000000000000000, 0.000000000000000000 ) ) ;
#27209 = ORIENTED_EDGE ( 'NONE', *, *, #17041, .T. ) ;
#27210 = EDGE_CURVE ( 'NONE', #16104, #10372, #5199, .T. ) ;
#27211 = CARTESIAN_POINT ( 'NONE',  ( 0.000000000000000000, -54.09091620264790379, 102.6166301549515936 ) ) ;
#27212 = ORIENTED_EDGE ( 'NONE', *, *, #14582, .F. ) ;
#27213 = CARTESIAN_POINT ( 'NONE',  ( 15.62097837807030842, 40.00000000000000000, -17.81927981957692353 ) ) ;
#27214 = VECTOR ( 'NONE', #21849, 1000.000000000000000 ) ;
#27215 = VERTEX_POINT ( 'NONE', #32243 ) ;
#27216 = LINE ( 'NONE', #27874, #13126 ) ;
#27217 = CIRCLE ( 'NONE', #11911, 120.5010000000000190 ) ;
#27218 = DIRECTION ( 'NONE',  ( 0.000000000000000000, 0.000000000000000000, 1.000000000000000000 ) ) ;
#27219 = CARTESIAN_POINT ( 'NONE',  ( 76.69346925293527306, 31.00000000000000000, 10.21457306974767398 ) ) ;
#27220 = CARTESIAN_POINT ( 'NONE',  ( -5.321195512787074478, 40.00000000000000000, 79.59297073838583003 ) ) ;
#27221 = CARTESIAN_POINT ( 'NONE',  ( -10.00000000000000000, 0.000000000000000000, 0.000000000000000000 ) ) ;
#27222 = VERTEX_POINT ( 'NONE', #29413 ) ;
#27223 = DIRECTION ( 'NONE',  ( -1.000000000000000000, 0.000000000000000000, 0.000000000000000000 ) ) ;
#27224 = ORIENTED_EDGE ( 'NONE', *, *, #24194, .T. ) ;
#27225 = LINE ( 'NONE', #1003, #38792 ) ;
#27226 = DIRECTION ( 'NONE',  ( 1.000000000000000000, 0.000000000000000000, -0.000000000000000000 ) ) ;
#27228 = VERTEX_POINT ( 'NONE', #2748 ) ;
#27227 = CARTESIAN_POINT ( 'NONE',  ( 5.200000000000002842, 0.000000000000000000, 2.500000000000000444 ) ) ;
#27229 = EDGE_CURVE ( 'NONE', #40591, #35323, #42678, .T. ) ;
#27230 = DIRECTION ( 'NONE',  ( -1.000000000000000000, 0.000000000000000000, 0.000000000000000000 ) ) ;
#27231 = ORIENTED_EDGE ( 'NONE', *, *, #30523, .F. ) ;
#27232 = CARTESIAN_POINT ( 'NONE',  ( 68.41617299536980568, 39.99999999999999289, 52.47886963225217016 ) ) ;
#27233 = CARTESIAN_POINT ( 'NONE',  ( 17.99999999999999645, -92.10690493017015967, -64.06707842432270184 ) ) ;
#27234 = VERTEX_POINT ( 'NONE', #3176 ) ;
#27235 = VECTOR ( 'NONE', #20106, 1000.000000000000000 ) ;
#27236 = CARTESIAN_POINT ( 'NONE',  ( 18.00000000000000355, -24.72041153920704204, -40.55929306992713634 ) ) ;
#27237 = CARTESIAN_POINT ( 'NONE',  ( 17.99999999999999645, 97.89532456239568603, -54.81585448086097045 ) ) ;
#27238 = EDGE_LOOP ( 'NONE', ( #42815, #9356, #27621, #17328 ) ) ;
#27239 = VECTOR ( 'NONE', #27202, 1000.000000000000000 ) ;
#27240 = EDGE_CURVE ( 'NONE', #11938, #2698, #12828, .T. ) ;
#27241 =( NAMED_UNIT ( * ) PLANE_ANGLE_UNIT ( ) SI_UNIT ( $, .RADIAN. ) );
#27242 = ORIENTED_EDGE ( 'NONE', *, *, #12080, .T. ) ;
#27243 = DIRECTION ( 'NONE',  ( 0.000000000000000000, 0.000000000000000000, 1.000000000000000000 ) ) ;
#27244 = VERTEX_POINT ( 'NONE', #26137 ) ;
#27245 = DIRECTION ( 'NONE',  ( -1.000000000000000000, -0.000000000000000000, -0.000000000000000000 ) ) ;
#27246 = DIRECTION ( 'NONE',  ( 0.000000000000000000, 0.000000000000000000, 1.000000000000000000 ) ) ;
#27247 = AXIS2_PLACEMENT_3D ( 'NONE', #29986, #40615, #6832 ) ;
#27248 = EDGE_CURVE ( 'NONE', #22633, #15523, #7970, .T. ) ;
#27249 = DIRECTION ( 'NONE',  ( 1.000000000000000000, -1.373900992973641671E-15, -3.895519384649692070E-16 ) ) ;
#27250 = CIRCLE ( 'NONE', #8428, 120.5010000000000190 ) ;
#27251 = DIRECTION ( 'NONE',  ( 1.000000000000000000, 0.000000000000000000, 0.000000000000000000 ) ) ;
#27252 = ORIENTED_EDGE ( 'NONE', *, *, #35697, .F. ) ;
#27254 = DIRECTION ( 'NONE',  ( -1.000000000000000000, 0.000000000000000000, -0.000000000000000000 ) ) ;
#27253 = LINE ( 'NONE', #23351, #745 ) ;
#27255 = ORIENTED_EDGE ( 'NONE', *, *, #3409, .F. ) ;
#27256 = AXIS2_PLACEMENT_3D ( 'NONE', #9357, #35741, #29240 ) ;
#27257 = CARTESIAN_POINT ( 'NONE',  ( 17.99999999999999645, 84.62908780824871258, 85.78116633471321961 ) ) ;
#27258 = CARTESIAN_POINT ( 'NONE',  ( 2.127120017302678523, 31.00000000000000355, -32.60416666460785962 ) ) ;
#27259 = ORIENTED_EDGE ( 'NONE', *, *, #4397, .F. ) ;
#27260 = DIRECTION ( 'NONE',  ( 1.000000000000000000, 0.000000000000000000, 0.000000000000000000 ) ) ;
#27261 = VECTOR ( 'NONE', #216, 1000.000000000000000 ) ;
#27262 = DIRECTION ( 'NONE',  ( -1.000000000000000000, 0.000000000000000000, -0.000000000000000000 ) ) ;
#27263 = ITEM_DEFINED_TRANSFORMATION ( 'NONE', 'NONE', #7253,  #13552 ) ;
#27264 = DIRECTION ( 'NONE',  ( -1.000000000000000000, 0.000000000000000000, 0.000000000000000000 ) ) ;
#27265 = CARTESIAN_POINT ( 'NONE',  ( 33.41571365387085280, 31.00000000000000355, 57.85165222247763239 ) ) ;
#27266 = EDGE_CURVE ( 'NONE', #17290, #14958, #19822, .T. ) ;
#27267 = ORIENTED_EDGE ( 'NONE', *, *, #32091, .T. ) ;
#27268 = CARTESIAN_POINT ( 'NONE',  ( 42.86166521170756027, 31.00000000000000355, 21.22462828018744219 ) ) ;
#27269 = CARTESIAN_POINT ( 'NONE',  ( -5.072363130230006512, 40.00000000000000000, 77.60416666578095146 ) ) ;
#27270 = AXIS2_PLACEMENT_3D ( 'NONE', #21120, #37637, #24599 ) ;
#27271 = AXIS2_PLACEMENT_3D ( 'NONE', #19748, #35640, #16472 ) ;
#27272 = DIRECTION ( 'NONE',  ( 0.000000000000000000, 0.000000000000000000, 1.000000000000000000 ) ) ;
#27273 = CIRCLE ( 'NONE', #62, 120.5010000000000190 ) ;
#27274 = CARTESIAN_POINT ( 'NONE',  ( 4.999999999999997335, 0.000000000000000000, 0.000000000000000000 ) ) ;
#27275 = DIRECTION ( 'NONE',  ( 1.000000000000000000, -1.373900992973643249E-15, -5.551115123125812284E-16 ) ) ;
#27276 = AXIS2_PLACEMENT_3D ( 'NONE', #26109, #12797, #42223 ) ;
#27277 = ORIENTED_EDGE ( 'NONE', *, *, #16007, .F. ) ;
#27278 = CYLINDRICAL_SURFACE ( 'NONE', #2986, 13.60000000000000142 ) ;
#27279 = CARTESIAN_POINT ( 'NONE',  ( -10.00000000000000000, 0.000000000000000000, 0.000000000000000000 ) ) ;
#27280 = EDGE_CURVE ( 'NONE', #12750, #40931, #22650, .T. ) ;
#27281 = VERTEX_POINT ( 'NONE', #19609 ) ;
#27282 = CARTESIAN_POINT ( 'NONE',  ( 3.763366191185776088, 40.00000000000000000, 57.39583333449059666 ) ) ;
#27283 = DIRECTION ( 'NONE',  ( -1.000000000000000000, 0.000000000000000000, -0.000000000000000000 ) ) ;
#27284 = DIRECTION ( 'NONE',  ( 0.000000000000000000, 0.000000000000000000, -1.000000000000000000 ) ) ;
#27285 = CIRCLE ( 'NONE', #8464, 59.00000000000000000 ) ;
#27286 = ORIENTED_EDGE ( 'NONE', *, *, #16894, .T. ) ;
#27287 = CARTESIAN_POINT ( 'NONE',  ( 17.99999999999999645, 31.80866420683990725, 2.997093558041416195 ) ) ;
#27288 = DIRECTION ( 'NONE',  ( -1.000000000000000000, -0.000000000000000000, -0.000000000000000000 ) ) ;
#27289 = ORIENTED_EDGE ( 'NONE', *, *, #37223, .T. ) ;
#27290 = DIRECTION ( 'NONE',  ( -0.000000000000000000, -0.000000000000000000, -1.000000000000000000 ) ) ;
#27291 = ORIENTED_EDGE ( 'NONE', *, *, #16011, .T. ) ;
#27292 = EDGE_CURVE ( 'NONE', #17290, #3403, #10785, .T. ) ;
#27293 = CARTESIAN_POINT ( 'NONE',  ( 0.000000000000000000, 0.000000000000000000, -6.000000000000000000 ) ) ;
#27294 = ORIENTED_EDGE ( 'NONE', *, *, #3282, .T. ) ;
#27295 = CYLINDRICAL_SURFACE ( 'NONE', #39690, 13.59999999999999787 ) ;
#27296 = DIRECTION ( 'NONE',  ( 0.000000000000000000, 0.000000000000000000, -1.000000000000000000 ) ) ;
#27297 = EDGE_CURVE ( 'NONE', #24263, #38578, #39193, .T. ) ;
#27298 = EDGE_LOOP ( 'NONE', ( #32797, #4400, #11386, #8150 ) ) ;
#27299 = CARTESIAN_POINT ( 'NONE',  ( 31.80287614962791665, -40.05525454449572464, 69.29271901957253021 ) ) ;
#27300 = ADVANCED_FACE ( 'NONE', ( #9316 ), #5625, .F. ) ;
#27301 = DIRECTION ( 'NONE',  ( 0.000000000000000000, 0.000000000000000000, 1.000000000000000000 ) ) ;
#27302 = VERTEX_POINT ( 'NONE', #32454 ) ;
#27303 = DIRECTION ( 'NONE',  ( 0.000000000000000000, 0.000000000000000000, -1.000000000000000000 ) ) ;
#27304 = AXIS2_PLACEMENT_3D ( 'NONE', #38010, #41275, #18431 ) ;
#27305 = AXIS2_PLACEMENT_3D ( 'NONE', #9942, #25916, #28969 ) ;
#27306 = DIRECTION ( 'NONE',  ( 1.000000000000000000, 0.000000000000000000, -3.273063162220425331E-16 ) ) ;
#27307 = CARTESIAN_POINT ( 'NONE',  ( -106.4195705685756081, 106.4195705685752529, 10.00000000000000000 ) ) ;
#27308 = AXIS2_PLACEMENT_3D ( 'NONE', #38272, #8386, #21752 ) ;
#27309 = DIRECTION ( 'NONE',  ( 0.000000000000000000, -1.411300455031978955E-14, -1.000000000000000000 ) ) ;
#27310 = ORIENTED_EDGE ( 'NONE', *, *, #21907, .T. ) ;
#27311 = DIRECTION ( 'NONE',  ( 1.110223024625194258E-16, 0.9999999999999998890, -8.326672684688820732E-17 ) ) ;
#27312 = FACE_OUTER_BOUND ( 'NONE', #24273, .T. ) ;
#27313 = CARTESIAN_POINT ( 'NONE',  ( 2.781618486875130358, 31.00000000000000355, -42.60416666509636485 ) ) ;
#27314 = EDGE_CURVE ( 'NONE', #22843, #34135, #16333, .T. ) ;
#27315 = AXIS2_PLACEMENT_3D ( 'NONE', #13151, #29085, #39713 ) ;
#27316 = ORIENTED_EDGE ( 'NONE', *, *, #11418, .F. ) ;
#27317 = LINE ( 'NONE', #4153, #38616 ) ;
#27318 = EDGE_CURVE ( 'NONE', #28779, #19793, #4266, .T. ) ;
#27319 = CARTESIAN_POINT ( 'NONE',  ( 18.00000000000000355, 49.25004636492388954, 16.68630974939776834 ) ) ;
#27320 = ORIENTED_EDGE ( 'NONE', *, *, #38485, .F. ) ;
#27321 = DIRECTION ( 'NONE',  ( 1.000000000000000000, 0.000000000000000000, 0.000000000000000000 ) ) ;
#27322 = CARTESIAN_POINT ( 'NONE',  ( -47.94314659152439617, 40.00000000000000000, -16.27230485535717719 ) ) ;
#27323 = CARTESIAN_POINT ( 'NONE',  ( -61.40313508883502891, 40.00000000000000711, 7.989450542818913092 ) ) ;
#27324 = ORIENTED_EDGE ( 'NONE', *, *, #9647, .T. ) ;
#27325 = DIRECTION ( 'NONE',  ( -1.000000000000000000, -0.000000000000000000, 0.000000000000000000 ) ) ;
#27326 = CARTESIAN_POINT ( 'NONE',  ( 17.99999999999999645, 0.000000000000000000, 0.000000000000000000 ) ) ;
#27327 = PLANE ( 'NONE',  #4669 ) ;
#27328 = CARTESIAN_POINT ( 'NONE',  ( 0.000000000000000000, -45.89132998247981732, -102.3829004574634496 ) ) ;
#27329 = CIRCLE ( 'NONE', #20411, 19.19999999999999218 ) ;
#27330 = ORIENTED_EDGE ( 'NONE', *, *, #39410, .F. ) ;
#27331 = CARTESIAN_POINT ( 'NONE',  ( -18.08361268445098347, 40.00000000000000000, -10.43497034982449456 ) ) ;
#27332 = ORIENTED_EDGE ( 'NONE', *, *, #41449, .T. ) ;
#27333 = DIRECTION ( 'NONE',  ( -1.000000000000000000, -0.000000000000000000, -0.000000000000000000 ) ) ;
#27334 = CIRCLE ( 'NONE', #16893, 47.49900000000000233 ) ;
#27335 = CARTESIAN_POINT ( 'NONE',  ( 0.000000000000000000, 111.9370513079675789, -44.61600100275059333 ) ) ;
#27336 = CIRCLE ( 'NONE', #39141, 52.00000000000000000 ) ;
#27337 = VERTEX_POINT ( 'NONE', #24175 ) ;
#27338 = DIRECTION ( 'NONE',  ( 0.000000000000000000, 0.000000000000000000, 1.000000000000000000 ) ) ;
#27339 = VECTOR ( 'NONE', #15932, 1000.000000000000000 ) ;
#27340 = CARTESIAN_POINT ( 'NONE',  ( 0.000000000000000000, 0.000000000000000000, -20.00000000000000000 ) ) ;
#27341 = ORIENTED_EDGE ( 'NONE', *, *, #26210, .T. ) ;
#27342 = CYLINDRICAL_SURFACE ( 'NONE', #11044, 31.49899999999999878 ) ;
#27343 = VERTEX_POINT ( 'NONE', #27422 ) ;
#27344 = FACE_OUTER_BOUND ( 'NONE', #32592, .T. ) ;
#27345 = EDGE_CURVE ( 'NONE', #26382, #28779, #14251, .T. ) ;
#27346 = CIRCLE ( 'NONE', #16235, 2.649999999999985700 ) ;
#27347 = ORIENTED_EDGE ( 'NONE', *, *, #10122, .T. ) ;
#27349 = ORIENTED_EDGE ( 'NONE', *, *, #21940, .T. ) ;
#27348 = DIRECTION ( 'NONE',  ( -3.996523416598930318E-16, 2.658563593772947863E-15, 1.000000000000000000 ) ) ;
#27350 = CARTESIAN_POINT ( 'NONE',  ( 24.27443280711675300, 31.00000000000000355, -71.15176282235542260 ) ) ;
#27351 = EDGE_CURVE ( 'NONE', #15394, #42205, #7330, .T. ) ;
#27352 = EDGE_LOOP ( 'NONE', ( #17899, #24255, #20879, #11087 ) ) ;
#27353 = FACE_OUTER_BOUND ( 'NONE', #31525, .T. ) ;
#27354 = EDGE_CURVE ( 'NONE', #8485, #20720, #3038, .T. ) ;
#27355 = ORIENTED_EDGE ( 'NONE', *, *, #18598, .T. ) ;
#27356 = DIRECTION ( 'NONE',  ( 0.000000000000000000, -0.2486898871648415554, -0.9685831611286345177 ) ) ;
#27357 = EDGE_LOOP ( 'NONE', ( #22388, #32621, #16481, #28878 ) ) ;
#27358 = CARTESIAN_POINT ( 'NONE',  ( -59.98614492175870794, 40.00000000000000711, 68.21249229748744369 ) ) ;
#27360 = CARTESIAN_POINT ( 'NONE',  ( 17.99999999999999645, -11.41303419184897017, -111.6154788735837116 ) ) ;
#27359 = DIRECTION ( 'NONE',  ( 1.000000000000000000, 0.000000000000000000, 0.000000000000000000 ) ) ;
#27361 = DIRECTION ( 'NONE',  ( 0.000000000000000000, 0.000000000000000000, 1.000000000000000000 ) ) ;
#27362 = CARTESIAN_POINT ( 'NONE',  ( 17.99999999999999645, 0.000000000000000000, 0.000000000000000000 ) ) ;
#27363 = ORIENTED_EDGE ( 'NONE', *, *, #12541, .F. ) ;
#27364 = VECTOR ( 'NONE', #42034, 1000.000000000000000 ) ;
#27365 = CARTESIAN_POINT ( 'NONE',  ( 17.99999999999999645, 94.83915810436481308, -59.94836581341496640 ) ) ;
#27366 = DIRECTION ( 'NONE',  ( 0.000000000000000000, -0.5877852522924624790, -0.8090169943749551118 ) ) ;
#27367 = AXIS2_PLACEMENT_3D ( 'NONE', #39844, #26369, #39634 ) ;
#27368 = EDGE_CURVE ( 'NONE', #12013, #11159, #38605, .T. ) ;
#27369 = CARTESIAN_POINT ( 'NONE',  ( -44.26264085333531995, 31.00000000000000711, 76.66224561662070869 ) ) ;
#27370 = EDGE_CURVE ( 'NONE', #14587, #26032, #20691, .T. ) ;
#27371 = CARTESIAN_POINT ( 'NONE',  ( 3.472371940585993855, 2.614027278893175321, -3.320322319201766792 ) ) ;
#27372 = ORIENTED_EDGE ( 'NONE', *, *, #26802, .F. ) ;
#27373 = EDGE_CURVE ( 'NONE', #31744, #21728, #17763, .T. ) ;
#27374 = EDGE_CURVE ( 'NONE', #18374, #33890, #23324, .T. ) ;
#27375 = AXIS2_PLACEMENT_3D ( 'NONE', #17007, #20286, #10647 ) ;
#27376 = CARTESIAN_POINT ( 'NONE',  ( 17.99999999999999645, 5.822172717930266472, 31.41458249383143198 ) ) ;
#27377 = ORIENTED_EDGE ( 'NONE', *, *, #41281, .F. ) ;
#27378 = ORIENTED_EDGE ( 'NONE', *, *, #10257, .T. ) ;
#27379 = FILL_AREA_STYLE ('',( #10573 ) ) ;
#27380 = CARTESIAN_POINT ( 'NONE',  ( -2.500000000000000444, 3.061616997868383634E-16, -25.03750572909317285 ) ) ;
#27381 = DIRECTION ( 'NONE',  ( 0.000000000000000000, 0.000000000000000000, -1.000000000000000000 ) ) ;
#27382 = DIRECTION ( 'NONE',  ( -1.000000000000000000, 0.000000000000000000, 0.000000000000000000 ) ) ;
#27383 = ORIENTED_EDGE ( 'NONE', *, *, #18002, .F. ) ;
#27384 = CARTESIAN_POINT ( 'NONE',  ( 0.000000000000000000, -150.5000000000000284, 10.00000000000000000 ) ) ;
#27385 = VERTEX_POINT ( 'NONE', #27211 ) ;
#27386 = LINE ( 'NONE', #27608, #8167 ) ;
#27387 = CARTESIAN_POINT ( 'NONE',  ( 0.000000000000000000, 0.000000000000000000, 0.000000000000000000 ) ) ;
#27388 = DIRECTION ( 'NONE',  ( 0.000000000000000000, 0.8443279255020164076, -0.5358267949789947693 ) ) ;
#27389 = VERTEX_POINT ( 'NONE', #37438 ) ;
#27390 = ORIENTED_EDGE ( 'NONE', *, *, #30943, .T. ) ;
#27391 = CARTESIAN_POINT ( 'NONE',  ( -1.420922472151883646E-13, 9.833206111663764869E-13, 369.6955262170047831 ) ) ;
#27392 = DIRECTION ( 'NONE',  ( 0.000000000000000000, -0.9822872507286865007, -0.1873813145857354812 ) ) ;
#27393 = ADVANCED_FACE ( 'NONE', ( #4046 ), #23737, .T. ) ;
#27394 = CIRCLE ( 'NONE', #25338, 36.00000000000000000 ) ;
#27395 = CARTESIAN_POINT ( 'NONE',  ( 4.000000000000000000, 0.8378280264232961239, -3.220590601395640018 ) ) ;
#27396 = ORIENTED_EDGE ( 'NONE', *, *, #16996, .F. ) ;
#27398 = VERTEX_POINT ( 'NONE', #23950 ) ;
#27397 = DIRECTION ( 'NONE',  ( -1.000000000000000000, 0.000000000000000000, 0.000000000000000000 ) ) ;
#27399 = CARTESIAN_POINT ( 'NONE',  ( 46.89194940766294906, 31.00000000000000355, 6.259973086888626526 ) ) ;
#27400 = DIRECTION ( 'NONE',  ( 3.009274222672345096E-17, 1.000000000000000000, -2.455023325076455345E-18 ) ) ;
#27402 = ORIENTED_EDGE ( 'NONE', *, *, #18629, .T. ) ;
#27401 = CARTESIAN_POINT ( 'NONE',  ( 17.99999999999999645, -98.69720329640996681, 60.94966826379877745 ) ) ;
#27403 = ORIENTED_EDGE ( 'NONE', *, *, #17227, .F. ) ;
#27404 = DIRECTION ( 'NONE',  ( -1.000000000000000000, 0.000000000000000000, 0.000000000000000000 ) ) ;
#27406 = CARTESIAN_POINT ( 'NONE',  ( 54.03410584561684971, 40.00000000000000000, 41.58544482236945328 ) ) ;
#27405 = CIRCLE ( 'NONE', #31577, 31.49900000000000233 ) ;
#27407 = CARTESIAN_POINT ( 'NONE',  ( -12.69999999999999929, 1.641026710857453510E-15, 13.40000000000000213 ) ) ;
#27408 = FACE_OUTER_BOUND ( 'NONE', #36169, .T. ) ;
#27409 = VERTEX_POINT ( 'NONE', #36563 ) ;
#27410 = CYLINDRICAL_SURFACE ( 'NONE', #28623, 120.5010000000000190 ) ;
#27411 = ORIENTED_EDGE ( 'NONE', *, *, #19705, .T. ) ;
#27412 = DIRECTION ( 'NONE',  ( -3.009274222672345096E-17, -1.000000000000000000, 2.455023325076454960E-18 ) ) ;
#27413 = DIRECTION ( 'NONE',  ( 1.000000000000000000, 0.000000000000000000, 0.000000000000000000 ) ) ;
#27414 = EDGE_CURVE ( 'NONE', #6179, #34636, #42826, .T. ) ;
#27415 = CARTESIAN_POINT ( 'NONE',  ( -46.87443272357899815, 31.00000000000000355, 35.96965017775951878 ) ) ;
#27416 = EDGE_CURVE ( 'NONE', #16411, #9970, #41437, .T. ) ;
#27417 = DIRECTION ( 'NONE',  ( 1.000000000000000000, 0.000000000000000000, 0.000000000000000000 ) ) ;
#27418 = ORIENTED_EDGE ( 'NONE', *, *, #13528, .F. ) ;
#27419 = EDGE_CURVE ( 'NONE', #7533, #26358, #33063, .T. ) ;
#27420 = ADVANCED_FACE ( 'NONE', ( #34166 ), #39834, .T. ) ;
#27421 = EDGE_CURVE ( 'NONE', #11059, #35721, #28249, .T. ) ;
#27422 = CARTESIAN_POINT ( 'NONE',  ( 18.00000000000000355, 8.053585752062561554, -46.81126742072013514 ) ) ;
#27423 = ORIENTED_EDGE ( 'NONE', *, *, #11107, .F. ) ;
#27424 = CIRCLE ( 'NONE', #18432, 20.00000000000000000 ) ;
#27425 = CARTESIAN_POINT ( 'NONE',  ( -13.09503298281258132, 40.00000000000000000, -17.05789676611946959 ) ) ;
#27426 = ORIENTED_EDGE ( 'NONE', *, *, #26660, .F. ) ;
#27427 = CARTESIAN_POINT ( 'NONE',  ( 18.00000000000000355, 8.053585752061904302, 46.81126742072025593 ) ) ;
#27428 = CARTESIAN_POINT ( 'NONE',  ( -80.96080130434580724, -40.05525454449572464, 14.45886780445738395 ) ) ;
#27429 = CARTESIAN_POINT ( 'NONE',  ( 51.69257347811147696, 31.00000000000000355, 59.10123636506271083 ) ) ;
#27430 = CARTESIAN_POINT ( 'NONE',  ( -70.06919973880852126, 40.00000000000000711, -18.87919424805731339 ) ) ;
#27431 = EDGE_CURVE ( 'NONE', #23269, #21931, #36538, .T. ) ;
#27432 = DIRECTION ( 'NONE',  ( 0.000000000000000000, 0.000000000000000000, -1.000000000000000000 ) ) ;
#27433 = VERTEX_POINT ( 'NONE', #10178 ) ;
#27434 = CARTESIAN_POINT ( 'NONE',  ( 4.000000000000000000, -2.309401076758514915, -3.433295621305383349 ) ) ;
#27435 = EDGE_LOOP ( 'NONE', ( #27843, #21829, #14453, #23846, #2994 ) ) ;
#27436 = CARTESIAN_POINT ( 'NONE',  ( 18.00000000000000355, 0.000000000000000000, 0.000000000000000000 ) ) ;
#27437 = CARTESIAN_POINT ( 'NONE',  ( 17.99999999999999645, 87.92975456462995965, -69.68953103478068556 ) ) ;
#27439 = ORIENTED_EDGE ( 'NONE', *, *, #39160, .F. ) ;
#27438 = CARTESIAN_POINT ( 'NONE',  ( -10.00000000000000000, 0.000000000000000000, 0.000000000000000000 ) ) ;
#27440 = DIRECTION ( 'NONE',  ( 0.000000000000000000, 0.000000000000000000, -1.000000000000000000 ) ) ;
#27441 = ORIENTED_EDGE ( 'NONE', *, *, #29055, .T. ) ;
#27442 = CARTESIAN_POINT ( 'NONE',  ( 0.000000000000000000, 0.000000000000000000, 0.000000000000000000 ) ) ;
#27443 = AXIS2_PLACEMENT_3D ( 'NONE', #35633, #39317, #3316 ) ;
#27444 = CARTESIAN_POINT ( 'NONE',  ( 80.16187752211510542, 39.99999999999999289, -27.22680903928618434 ) ) ;
#27445 = FACE_OUTER_BOUND ( 'NONE', #42596, .T. ) ;
#27446 = ORIENTED_EDGE ( 'NONE', *, *, #7862, .T. ) ;
#27447 = DIRECTION ( 'NONE',  ( 0.000000000000000000, 0.000000000000000000, 1.000000000000000000 ) ) ;
#27448 = AXIS2_PLACEMENT_3D ( 'NONE', #929, #41514, #8365 ) ;
#27449 = CARTESIAN_POINT ( 'NONE',  ( 0.000000000000000000, 0.000000000000000000, 0.000000000000000000 ) ) ;
#27450 = VECTOR ( 'NONE', #16160, 1000.000000000000000 ) ;
#27451 = ORIENTED_EDGE ( 'NONE', *, *, #31905, .F. ) ;
#27452 = CYLINDRICAL_SURFACE ( 'NONE', #17052, 12.59999999999999964 ) ;
#27453 = AXIS2_PLACEMENT_3D ( 'NONE', #37934, #11795, #41416 ) ;
#27454 = ORIENTED_EDGE ( 'NONE', *, *, #11172, .T. ) ;
#27455 = CARTESIAN_POINT ( 'NONE',  ( 17.99999999999999645, -111.8797445107945236, 8.437727291342365987 ) ) ;
#27456 = ORIENTED_EDGE ( 'NONE', *, *, #32299, .F. ) ;
#27457 = CARTESIAN_POINT ( 'NONE',  ( 6.473670811831357064, 40.00000000000000000, -24.11571013580714151 ) ) ;
#27458 = CARTESIAN_POINT ( 'NONE',  ( 18.00000000000000355, 44.47301969247445186, 16.68249143361925491 ) ) ;
#27459 = DIRECTION ( 'NONE',  ( -0.06345332152672161774, 0.000000000000000000, 0.9979848074931934043 ) ) ;
#27460 = CARTESIAN_POINT ( 'NONE',  ( 18.00000000000000355, -36.06787431788649911, -37.45808914225526820 ) ) ;
#27461 = EDGE_LOOP ( 'NONE', ( #39959, #34372, #41766, #8226 ) ) ;
#27464 = LINE ( 'NONE', #20739, #6708 ) ;
#27463 = CYLINDRICAL_SURFACE ( 'NONE', #13371, 51.99999999999999289 ) ;
#27462 = AXIS2_PLACEMENT_3D ( 'NONE', #12242, #22303, #19027 ) ;
#27465 = ORIENTED_EDGE ( 'NONE', *, *, #12742, .F. ) ;
#27466 = AXIS2_PLACEMENT_3D ( 'NONE', #9265, #25680, #35456 ) ;
#27467 = DIRECTION ( 'NONE',  ( 1.000000000000000000, 1.836909530733573776E-16, 0.000000000000000000 ) ) ;
#27468 = CARTESIAN_POINT ( 'NONE',  ( 25.10416666396844576, 31.00000000000000355, 1.636246165087044124 ) ) ;
#27469 = VERTEX_POINT ( 'NONE', #333 ) ;
#27470 = CARTESIAN_POINT ( 'NONE',  ( 0.000000000000000000, 0.000000000000000000, 0.000000000000000000 ) ) ;
#27471 = EDGE_CURVE ( 'NONE', #291, #192, #22680, .T. ) ;
#27472 = EDGE_CURVE ( 'NONE', #12319, #33465, #20259, .T. ) ;
#27473 = FACE_BOUND ( 'NONE', #1807, .T. ) ;
#27474 = AXIS2_PLACEMENT_3D ( 'NONE', #32066, #31861, #41872 ) ;
#27475 = EDGE_CURVE ( 'NONE', #15430, #1492, #42113, .T. ) ;
#27476 = AXIS2_PLACEMENT_3D ( 'NONE', #31866, #32274, #8505 ) ;
#27477 = LINE ( 'NONE', #26828, #3726 ) ;
#27478 = CARTESIAN_POINT ( 'NONE',  ( -69.89583333424914713, 31.00000000000000711, 4.581489278091138040 ) ) ;
#27479 = VECTOR ( 'NONE', #27601, 1000.000000000000000 ) ;
#27480 = VERTEX_POINT ( 'NONE', #40918 ) ;
#27481 = CARTESIAN_POINT ( 'NONE',  ( 36.58905133582347702, 31.00000000000000355, -27.97030060560319953 ) ) ;
#27482 = CIRCLE ( 'NONE', #28212, 59.00000000000000711 ) ;
#27483 = CARTESIAN_POINT ( 'NONE',  ( -39.25113411183426848, 40.00000000000000000, 67.98392962655870519 ) ) ;
#27484 = EDGE_CURVE ( 'NONE', #40651, #15607, #31554, .T. ) ;
#27485 = AXIS2_PLACEMENT_3D ( 'NONE', #40061, #6484, #40290 ) ;
#27486 = DIRECTION ( 'NONE',  ( -1.000000000000000000, -0.000000000000000000, 0.000000000000000000 ) ) ;
#27487 = EDGE_CURVE ( 'NONE', #27181, #15605, #35853, .T. ) ;
#27488 = DIRECTION ( 'NONE',  ( -1.000000000000000000, -0.000000000000000000, -0.000000000000000000 ) ) ;
#27489 = CYLINDRICAL_SURFACE ( 'NONE', #5195, 18.77999999999999048 ) ;
#27491 = VERTEX_POINT ( 'NONE', #31129 ) ;
#27490 = CARTESIAN_POINT ( 'NONE',  ( 0.5999999999999994227, -12.75000000000000000, 0.000000000000000000 ) ) ;
#27492 = DIRECTION ( 'NONE',  ( -0.000000000000000000, 0.000000000000000000, 1.000000000000000000 ) ) ;
#27493 = CARTESIAN_POINT ( 'NONE',  ( 17.99999999999999645, 27.83061035786954918, 117.2431154827798281 ) ) ;
#27494 = ORIENTED_EDGE ( 'NONE', *, *, #27788, .F. ) ;
#27495 = CARTESIAN_POINT ( 'NONE',  ( -59.89583333444493718, 40.00000000000000711, 3.926990808566372060 ) ) ;
#27496 = CARTESIAN_POINT ( 'NONE',  ( 9.000000000000001776, -18.53613841426822972, 48.58406706613897086 ) ) ;
#27497 = VECTOR ( 'NONE', #1536, 1000.000000000000000 ) ;
#27498 = DIRECTION ( 'NONE',  ( -1.000000000000000000, 0.000000000000000000, 0.000000000000000000 ) ) ;
#27499 = ORIENTED_EDGE ( 'NONE', *, *, #3259, .T. ) ;
#27500 = CYLINDRICAL_SURFACE ( 'NONE', #37748, 120.5010000000000190 ) ;
#27501 = DIRECTION ( 'NONE',  ( 1.000000000000000000, -3.035766082959412415E-17, 0.000000000000000000 ) ) ;
#27502 = MANIFOLD_SOLID_BREP ( 'Body', #28198 ) ;
#27503 = EDGE_LOOP ( 'NONE', ( #40095, #3919, #10502, #25360 ) ) ;
#27504 = DIRECTION ( 'NONE',  ( 0.000000000000000000, 0.000000000000000000, 1.000000000000000000 ) ) ;
#27505 = ORIENTED_EDGE ( 'NONE', *, *, #32960, .T. ) ;
#27506 = VECTOR ( 'NONE', #4297, 1000.000000000000000 ) ;
#27507 = VECTOR ( 'NONE', #42711, 1000.000000000000000 ) ;
#27508 = DIRECTION ( 'NONE',  ( 0.000000000000000000, 0.9714298932647106311, -0.2373266998711119624 ) ) ;
#27509 = B_SPLINE_CURVE_WITH_KNOTS ( 'NONE', 3,
 ( #23978, #14590, #10430, #17661, #37244, #34623 ),
 .UNSPECIFIED., .F., .F.,
 ( 4, 2, 4 ),
 ( 0.002365888236227977302, 0.003551327329835078910, 0.004736766423442180518 ),
 .UNSPECIFIED. ) ;
#27510 = ORIENTED_EDGE ( 'NONE', *, *, #40986, .T. ) ;
#27511 = AXIS2_PLACEMENT_3D ( 'NONE', #3300, #34233, #27720 ) ;
#27512 = CYLINDRICAL_SURFACE ( 'NONE', #16776, 59.00000000000000000 ) ;
#27513 = DIRECTION ( 'NONE',  ( -1.000000000000000000, -0.000000000000000000, 0.000000000000000000 ) ) ;
#27514 = EDGE_LOOP ( 'NONE', ( #14130, #18346, #41213, #29417 ) ) ;
#27515 = AXIS2_PLACEMENT_3D ( 'NONE', #38087, #38302, #5140 ) ;
#27516 = CARTESIAN_POINT ( 'NONE',  ( 18.00000000000000355, -43.83938735307255286, -18.28286404005844901 ) ) ;
#27517 = LINE ( 'NONE', #30996, #33120 ) ;
#27518 = ORIENTED_EDGE ( 'NONE', *, *, #26092, .F. ) ;
#27519 = DIRECTION ( 'NONE',  ( 0.000000000000000000, 0.000000000000000000, 1.000000000000000000 ) ) ;
#27520 = CIRCLE ( 'NONE', #22007, 36.00000000000000000 ) ;
#27521 = DIRECTION ( 'NONE',  ( -3.996523416598930318E-16, 2.658563593772947863E-15, 1.000000000000000000 ) ) ;
#27522 = CARTESIAN_POINT ( 'NONE',  ( 17.99999999999999645, 0.000000000000000000, 0.000000000000000000 ) ) ;
#27523 = EDGE_CURVE ( 'NONE', #25483, #3709, #21130, .T. ) ;
#27524 = DIRECTION ( 'NONE',  ( 0.000000000000000000, -0.3681245526846854133, 0.9297764858882485717 ) ) ;
#27525 = EDGE_LOOP ( 'NONE', ( #17968, #1063, #22517, #8255 ) ) ;
#27527 = AXIS2_PLACEMENT_3D ( 'NONE', #24771, #41512, #25206 ) ;
#27526 = CARTESIAN_POINT ( 'NONE',  ( 47.33767018637040280, -4.413178189597207806E-27, 69.39124571101467609 ) ) ;
#27528 = DIRECTION ( 'NONE',  ( 0.000000000000000000, -0.8951632913550663373, 0.4457383557765300375 ) ) ;
#27529 = CARTESIAN_POINT ( 'NONE',  ( -37.46020281470095625, 31.00000000000000355, 12.72710441276525017 ) ) ;
#27530 = VERTEX_POINT ( 'NONE', #41791 ) ;
#27532 = CARTESIAN_POINT ( 'NONE',  ( -101.9959696149863646, 35.50000000000000711, -0.1269066430510136789 ) ) ;
#27531 = LINE ( 'NONE', #39987, #7924 ) ;
#27533 = DIRECTION ( 'NONE',  ( -1.000000000000000000, 0.000000000000000000, 0.000000000000000000 ) ) ;
#27534 = ORIENTED_EDGE ( 'NONE', *, *, #28143, .F. ) ;
#27535 = ADVANCED_FACE ( 'NONE', ( #4932 ), #25256, .F. ) ;
#27536 = VECTOR ( 'NONE', #430, 1000.000000000000000 ) ;
#27537 = CARTESIAN_POINT ( 'NONE',  ( 20.55500000000001748, 3.061616997868384127E-16, -2.500000000000000888 ) ) ;
#27538 = CARTESIAN_POINT ( 'NONE',  ( -47.99616210117395099, 40.00000000000000000, 12.86278070621785119 ) ) ;
#27539 = CIRCLE ( 'NONE', #24067, 58.99999999999999289 ) ;
#27540 = CARTESIAN_POINT ( 'NONE',  ( 54.55067978551168295, 40.00000000000000000, 18.62288743479739495 ) ) ;
#27541 = EDGE_CURVE ( 'NONE', #18546, #8390, #21346, .T. ) ;
#27542 = EDGE_CURVE ( 'NONE', #14855, #29068, #8624, .T. ) ;
#27543 = DIRECTION ( 'NONE',  ( 1.000000000000000000, 0.000000000000000000, 0.000000000000000000 ) ) ;
#27544 = CIRCLE ( 'NONE', #29665, 116.0000000000000000 ) ;
#27545 = CARTESIAN_POINT ( 'NONE',  ( 26.85238513915532721, -2.055254544495723756, 88.54322126041917329 ) ) ;
#27546 = DIRECTION ( 'NONE',  ( 0.000000000000000000, 0.000000000000000000, -1.000000000000000000 ) ) ;
#27547 = AXIS2_PLACEMENT_3D ( 'NONE', #39800, #36753, #33490 ) ;
#27548 = ORIENTED_EDGE ( 'NONE', *, *, #9224, .F. ) ;
#27549 = CARTESIAN_POINT ( 'NONE',  ( -26.30698076681265363, 40.00000000000000000, 12.97770382244945253 ) ) ;
#27550 = ORIENTED_EDGE ( 'NONE', *, *, #20498, .F. ) ;
#27551 = CARTESIAN_POINT ( 'NONE',  ( 17.99999999999999645, 101.1249659627855806, -48.60055280209454054 ) ) ;
#27552 = LINE ( 'NONE', #20595, #7502 ) ;
#27553 = EDGE_LOOP ( 'NONE', ( #4152, #15764, #18293, #12756 ) ) ;
#27554 = CARTESIAN_POINT ( 'NONE',  ( -19.99999999999999645, 17.11489954122026447, 1.283214542831032867 ) ) ;
#27555 = CARTESIAN_POINT ( 'NONE',  ( 17.99999999999999645, -23.79363200506973186, 27.01597816121639184 ) ) ;
#27556 = ORIENTED_EDGE ( 'NONE', *, *, #8574, .F. ) ;
#27557 = DIRECTION ( 'NONE',  ( 0.000000000000000000, -0.4132121857683668797, -0.9106347728549183396 ) ) ;
#27558 = EDGE_LOOP ( 'NONE', ( #33591, #14169, #33618, #17946 ) ) ;
#27559 = EDGE_CURVE ( 'NONE', #39944, #24642, #5365, .T. ) ;
#27560 = EDGE_CURVE ( 'NONE', #14617, #2185, #19873, .T. ) ;
#27561 = AXIS2_PLACEMENT_3D ( 'NONE', #19077, #39722, #9211 ) ;
#27562 = ORIENTED_EDGE ( 'NONE', *, *, #39011, .F. ) ;
#27564 = VERTEX_POINT ( 'NONE', #989 ) ;
#27563 = DIRECTION ( 'NONE',  ( -1.058513553088275437E-16, -1.000000000000000000, 8.813324511995299047E-17 ) ) ;
#27565 = CARTESIAN_POINT ( 'NONE',  ( -35.33737842959504150, 31.00000000000000355, 60.98257694382487415 ) ) ;
#27567 = EDGE_CURVE ( 'NONE', #34450, #14228, #11725, .T. ) ;
#27566 = ORIENTED_EDGE ( 'NONE', *, *, #37709, .T. ) ;
#27568 = LINE ( 'NONE', #17563, #26557 ) ;
#27569 = AXIS2_PLACEMENT_3D ( 'NONE', #18489, #38292, #34810 ) ;
#27570 = AXIS2_PLACEMENT_3D ( 'NONE', #5234, #15094, #32076 ) ;
#27571 = ORIENTED_EDGE ( 'NONE', *, *, #24061, .T. ) ;
#27572 = CIRCLE ( 'NONE', #19243, 59.00000000000000711 ) ;
#27573 = CARTESIAN_POINT ( 'NONE',  ( 17.99999999999999645, -95.31344542257689056, -66.11616384574544725 ) ) ;
#27574 = ORIENTED_EDGE ( 'NONE', *, *, #15494, .T. ) ;
#27575 = CARTESIAN_POINT ( 'NONE',  ( 96.90013369365227902, 39.99999999999999289, -6.223598210838602540 ) ) ;
#27576 = AXIS2_PLACEMENT_3D ( 'NONE', #17140, #30850, #34114 ) ;
#27577 = CIRCLE ( 'NONE', #2461, 2.649999999999993694 ) ;
#27579 = CARTESIAN_POINT ( 'NONE',  ( 0.000000000000000000, 37.91532898920922889, 28.61088654061651937 ) ) ;
#27578 = DIRECTION ( 'NONE',  ( 0.000000000000000000, 0.6736956436465584286, -0.7390089172206580903 ) ) ;
#27580 = PRESENTATION_LAYER_ASSIGNMENT (  '', '', ( #25519 ) ) ;
#27581 = LINE ( 'NONE', #13861, #25533 ) ;
#27582 = CARTESIAN_POINT ( 'NONE',  ( 5.657435538624008755E-15, 4.615443851143735910E-16, 367.6955262170047263 ) ) ;
#27583 = EDGE_CURVE ( 'NONE', #3911, #33690, #14339, .T. ) ;
#27584 = ORIENTED_EDGE ( 'NONE', *, *, #19362, .T. ) ;
#27585 =( NAMED_UNIT ( * ) PLANE_ANGLE_UNIT ( ) SI_UNIT ( $, .RADIAN. ) );
#27586 = CIRCLE ( 'NONE', #8040, 59.00000000000000000 ) ;
#27587 = DIRECTION ( 'NONE',  ( 1.000000000000000000, 0.000000000000000000, -0.000000000000000000 ) ) ;
#27588 = FACE_OUTER_BOUND ( 'NONE', #11682, .T. ) ;
#27589 = CARTESIAN_POINT ( 'NONE',  ( 63.16980243745005907, 31.00000000000000000, -55.41789732285823078 ) ) ;
#27590 = FACE_OUTER_BOUND ( 'NONE', #20593, .T. ) ;
#27591 = VERTEX_POINT ( 'NONE', #14782 ) ;
#27592 = CARTESIAN_POINT ( 'NONE',  ( 18.71272080434063056, 40.00000000000000000, 21.38210947162712117 ) ) ;
#27593 = ADVANCED_FACE ( 'NONE', ( #25063 ), #24833, .F. ) ;
#27594 = ORIENTED_EDGE ( 'NONE', *, *, #326, .F. ) ;
#27595 = ORIENTED_EDGE ( 'NONE', *, *, #30132, .F. ) ;
#27596 = DIRECTION ( 'NONE',  ( 0.000000000000000000, 0.9980267284282717810, -0.06279051952930989056 ) ) ;
#27597 = EDGE_CURVE ( 'NONE', #26000, #35433, #31775, .T. ) ;
#27598 = DIRECTION ( 'NONE',  ( 0.000000000000000000, 2.587384167558627638E-15, -1.000000000000000000 ) ) ;
#27600 = DIRECTION ( 'NONE',  ( -1.000000000000000000, -0.000000000000000000, -0.000000000000000000 ) ) ;
#27599 = VECTOR ( 'NONE', #16708, 1000.000000000000000 ) ;
#27601 = DIRECTION ( 'NONE',  ( -1.000000000000000000, 0.000000000000000000, 0.000000000000000000 ) ) ;
#27602 = VECTOR ( 'NONE', #3220, 1000.000000000000000 ) ;
#27603 = VECTOR ( 'NONE', #16777, 1000.000000000000000 ) ;
#27604 = EDGE_LOOP ( 'NONE', ( #29311, #3642, #8396, #20436 ) ) ;
#27605 = CARTESIAN_POINT ( 'NONE',  ( 0.000000000000000000, 52.88069566989596382, -103.2454939717363516 ) ) ;
#27606 = EDGE_LOOP ( 'NONE', ( #10481, #12102, #16889, #18028 ) ) ;
#27607 = DIRECTION ( 'NONE',  ( -1.000000000000000000, -0.000000000000000000, -0.000000000000000000 ) ) ;
#27608 = CARTESIAN_POINT ( 'NONE',  ( 17.99999999999999645, -119.7318547011702634, 13.59315897125686412 ) ) ;
#27609 = MECHANICAL_DESIGN_GEOMETRIC_PRESENTATION_REPRESENTATION (  '', ( #26913 ), #5290 ) ;
#27610 = VECTOR ( 'NONE', #20251, 1000.000000000000000 ) ;
#27611 = CIRCLE ( 'NONE', #32451, 51.99999999999999289 ) ;
#27612 = DIRECTION ( 'NONE',  ( -1.000000000000000000, 0.000000000000000000, -0.000000000000000000 ) ) ;
#27613 = AXIS2_PLACEMENT_3D ( 'NONE', #13576, #36663, #4359 ) ;
#27614 = DIRECTION ( 'NONE',  ( 0.000000000000000000, 0.000000000000000000, 1.000000000000000000 ) ) ;
#27615 = ORIENTED_EDGE ( 'NONE', *, *, #36349, .T. ) ;
#27616 = ORIENTED_EDGE ( 'NONE', *, *, #11207, .T. ) ;
#27617 = CYLINDRICAL_SURFACE ( 'NONE', #25921, 20.00000000000000355 ) ;
#27618 = DIRECTION ( 'NONE',  ( 0.000000000000000000, 0.000000000000000000, -1.000000000000000000 ) ) ;
#27619 = CIRCLE ( 'NONE', #7380, 58.99999999999999289 ) ;
#27620 = CARTESIAN_POINT ( 'NONE',  ( 4.000000000000000000, 2.512223110932545023, -3.469391141908803711 ) ) ;
#27621 = ORIENTED_EDGE ( 'NONE', *, *, #28389, .T. ) ;
#27623 = ORIENTED_EDGE ( 'NONE', *, *, #15076, .T. ) ;
#27622 = CARTESIAN_POINT ( 'NONE',  ( 17.99999999999999645, 0.000000000000000000, 0.000000000000000000 ) ) ;
#27624 = CARTESIAN_POINT ( 'NONE',  ( 5.928665350384932253, 31.00000000000000355, -44.40877992884582426 ) ) ;
#27625 = EDGE_CURVE ( 'NONE', #32669, #267, #32401, .T. ) ;
#27626 = CARTESIAN_POINT ( 'NONE',  ( -102.0670434220619427, -2.055254544495720648, 139.0496534599708980 ) ) ;
#27627 = PRODUCT_DEFINITION ( 'UNKNOWN', '', #34420, #760 ) ;
#27629 = DIRECTION ( 'NONE',  ( 0.000000000000000000, 0.9957341762950341346, 0.09226835946330559646 ) ) ;
#27628 = DIRECTION ( 'NONE',  ( -1.000000000000000000, 0.000000000000000000, -0.000000000000000000 ) ) ;
#27630 = VERTEX_POINT ( 'NONE', #9709 ) ;
#27631 = CARTESIAN_POINT ( 'NONE',  ( 58.81396797841472335, 40.00000000000000000, 34.08301911901634895 ) ) ;
#27632 = AXIS2_PLACEMENT_3D ( 'NONE', #42134, #39879, #23149 ) ;
#27633 = DIRECTION ( 'NONE',  ( -1.000000000000000000, 0.000000000000000000, 0.000000000000000000 ) ) ;
#27634 = CARTESIAN_POINT ( 'NONE',  ( 4.000000000000000000, 2.309401076758497151, -5.000000000000000000 ) ) ;
#27636 = EDGE_LOOP ( 'NONE', ( #8994, #4492, #12018, #10894 ) ) ;
#27635 = CIRCLE ( 'NONE', #3917, 31.49900000000000588 ) ;
#27637 = FACE_OUTER_BOUND ( 'NONE', #37797, .T. ) ;
#27638 = VECTOR ( 'NONE', #33685, 1000.000000000000000 ) ;
#27639 = EDGE_CURVE ( 'NONE', #2980, #8823, #28921, .T. ) ;
#27640 = ORIENTED_EDGE ( 'NONE', *, *, #39627, .F. ) ;
#27641 = FILL_AREA_STYLE_COLOUR ( '', #24028 ) ;
#27642 = CIRCLE ( 'NONE', #19311, 2.649999999999985700 ) ;
#27643 = FACE_OUTER_BOUND ( 'NONE', #10086, .T. ) ;
#27644 = DIRECTION ( 'NONE',  ( -1.000000000000000000, -0.000000000000000000, 0.000000000000000000 ) ) ;
#27645 = AXIS2_PLACEMENT_3D ( 'NONE', #25821, #8999, #25615 ) ;
#27646 = CARTESIAN_POINT ( 'NONE',  ( 48.77780477658175329, 31.00000000000000355, -24.05648398140741406 ) ) ;
#27647 = DIRECTION ( 'NONE',  ( 1.000000000000000000, 0.000000000000000000, 0.000000000000000000 ) ) ;
#27648 = ORIENTED_EDGE ( 'NONE', *, *, #12665, .T. ) ;
#27650 = AXIS2_PLACEMENT_3D ( 'NONE', #8444, #1015, #1671 ) ;
#27649 = CARTESIAN_POINT ( 'NONE',  ( 18.00000000000000355, -3.840921266749491192, -47.34345070675175293 ) ) ;
#27651 = ORIENTED_EDGE ( 'NONE', *, *, #19705, .F. ) ;
#27652 = ADVANCED_FACE ( 'NONE', ( #6213 ), #39336, .T. ) ;
#27653 = CARTESIAN_POINT ( 'NONE',  ( -12.50349052776452297, 40.00000000000000000, 25.37591446456323041 ) ) ;
#27654 = EDGE_LOOP ( 'NONE', ( #23421, #2112, #13515, #28883 ) ) ;
#27655 = DIRECTION ( 'NONE',  ( 0.000000000000000000, 0.000000000000000000, 1.000000000000000000 ) ) ;
#27656 = ADVANCED_FACE ( 'NONE', ( #2909 ), #15850, .T. ) ;
#27657 = DIRECTION ( 'NONE',  ( -1.000000000000000000, 0.000000000000000000, 0.000000000000000000 ) ) ;
#27658 = CARTESIAN_POINT ( 'NONE',  ( 37.84579180137232157, 31.00000000000000355, -65.31998993212283722 ) ) ;
#27659 = CARTESIAN_POINT ( 'NONE',  ( 19.52887458859586900, 40.00000000000000000, -72.48875405283516216 ) ) ;
#27660 = AXIS2_PLACEMENT_3D ( 'NONE', #32821, #23050, #22620 ) ;
#27661 = MANIFOLD_SOLID_BREP ( 'CirPattern1', #38594 ) ;
#27662 = DIRECTION ( 'NONE',  ( 0.000000000000000000, 0.000000000000000000, 1.000000000000000000 ) ) ;
#27663 = ORIENTED_EDGE ( 'NONE', *, *, #42527, .T. ) ;
#27664 = LINE ( 'NONE', #31354, #24237 ) ;
#27665 = ORIENTED_EDGE ( 'NONE', *, *, #27841, .T. ) ;
#27666 = CARTESIAN_POINT ( 'NONE',  ( 18.00000000000000355, -42.03146605346801579, 22.12489237027304512 ) ) ;
#27667 = CARTESIAN_POINT ( 'NONE',  ( 17.99999999999999645, 87.92975456462900752, 69.68953103478187927 ) ) ;
#27668 = EDGE_CURVE ( 'NONE', #7181, #16426, #3793, .T. ) ;
#27669 = CIRCLE ( 'NONE', #26253, 10.99999999999998934 ) ;
#27671 = EDGE_LOOP ( 'NONE', ( #6894, #9041, #38545, #25178 ) ) ;
#27670 = CARTESIAN_POINT ( 'NONE',  ( 17.99999999999999645, 41.62036691425679180, -113.0850832732710529 ) ) ;
#27672 = FACE_OUTER_BOUND ( 'NONE', #22319, .T. ) ;
#27673 = ORIENTED_EDGE ( 'NONE', *, *, #5677, .F. ) ;
#27674 = LINE ( 'NONE', #4739, #12647 ) ;
#27675 = CARTESIAN_POINT ( 'NONE',  ( 24.08498528996878107, 40.00000000000000000, -89.94621034038658536 ) ) ;
#27676 = LINE ( 'NONE', #10644, #6175 ) ;
#27677 = ORIENTED_EDGE ( 'NONE', *, *, #1218, .F. ) ;
#27678 = ADVANCED_FACE ( 'NONE', ( #18934 ), #15434, .F. ) ;
#27679 = DIRECTION ( 'NONE',  ( -1.000000000000000000, 0.000000000000000000, -0.000000000000000000 ) ) ;
#27680 = ADVANCED_FACE ( 'NONE', ( #9268 ), #22844, .T. ) ;
#27681 = DIRECTION ( 'NONE',  ( 0.000000000000000000, 0.000000000000000000, 1.000000000000000000 ) ) ;
#27682 = AXIS2_PLACEMENT_3D ( 'NONE', #10858, #3834, #13929 ) ;
#27683 = EDGE_CURVE ( 'NONE', #19436, #40032, #8718, .T. ) ;
#27684 = ADVANCED_FACE ( 'NONE', ( #36094 ), #35660, .F. ) ;
#27685 = CIRCLE ( 'NONE', #14450, 59.00000000000000000 ) ;
#27686 = DIRECTION ( 'NONE',  ( 1.000000000000000000, 0.000000000000000000, 0.000000000000000000 ) ) ;
#27687 = ORIENTED_EDGE ( 'NONE', *, *, #18961, .F. ) ;
#27688 = LINE ( 'NONE', #40952, #8678 ) ;
#27689 = ORIENTED_EDGE ( 'NONE', *, *, #11244, .F. ) ;
#27690 = CARTESIAN_POINT ( 'NONE',  ( -24.64063138600937464, 40.00000000000000000, 18.85097431370326859 ) ) ;
#27691 = DIRECTION ( 'NONE',  ( 0.000000000000000000, 0.000000000000000000, 1.000000000000000000 ) ) ;
#27692 = CIRCLE ( 'NONE', #10961, 22.99999999999987921 ) ;
#27693 = CARTESIAN_POINT ( 'NONE',  ( 2.500000000000000000, 0.000000000000000000, 0.000000000000000000 ) ) ;
#27694 = CARTESIAN_POINT ( 'NONE',  ( 18.00000000000000355, -39.55064067543082018, 25.36340625197346199 ) ) ;
#27695 = ORIENTED_EDGE ( 'NONE', *, *, #35904, .F. ) ;
#27697 = CARTESIAN_POINT ( 'NONE',  ( 17.99999999999999645, 0.000000000000000000, 0.000000000000000000 ) ) ;
#27696 = DIRECTION ( 'NONE',  ( 0.000000000000000000, 0.000000000000000000, 1.000000000000000000 ) ) ;
#27698 = ORIENTED_EDGE ( 'NONE', *, *, #38768, .F. ) ;
#27699 = CARTESIAN_POINT ( 'NONE',  ( 17.99999999999999645, 3.803237743092368284, -31.26855263151010789 ) ) ;
#27700 = CARTESIAN_POINT ( 'NONE',  ( -7.231618336280544845, 31.00000000000000355, 27.02512817425793656 ) ) ;
#27702 = ORIENTED_EDGE ( 'NONE', *, *, #7199, .T. ) ;
#27701 = AXIS2_PLACEMENT_3D ( 'NONE', #26959, #36524, #20224 ) ;
#27703 = DIRECTION ( 'NONE',  ( -1.000000000000000000, 1.084202172485488534E-16, 0.000000000000000000 ) ) ;
#27704 = CARTESIAN_POINT ( 'NONE',  ( 17.99999999999999645, -13.22719389141960100, -28.58720592780609593 ) ) ;
#27705 = VECTOR ( 'NONE', #2603, 1000.000000000000000 ) ;
#27706 = CONTEXT_DEPENDENT_SHAPE_REPRESENTATION ( #41223, #36352 ) ;
#27707 = CIRCLE ( 'NONE', #18681, 13.59999999999999964 ) ;
#27708 = DIRECTION ( 'NONE',  ( 1.000000000000000000, -0.000000000000000000, 0.000000000000000000 ) ) ;
#27709 = CARTESIAN_POINT ( 'NONE',  ( 73.03870520561201829, 31.00000000000000000, -42.18585045165268355 ) ) ;
#27710 = CIRCLE ( 'NONE', #14476, 13.40000000000000213 ) ;
#27711 = EDGE_CURVE ( 'NONE', #15795, #15605, #35221, .T. ) ;
#27712 = VERTEX_POINT ( 'NONE', #42202 ) ;
#27714 = CARTESIAN_POINT ( 'NONE',  ( 46.49836147156941024, 31.00000000000000355, -6.043767708844123732 ) ) ;
#27713 = VECTOR ( 'NONE', #16731, 1000.000000000000000 ) ;
#27715 = AXIS2_PLACEMENT_3D ( 'NONE', #33625, #17086, #34712 ) ;
#27716 = CARTESIAN_POINT ( 'NONE',  ( -79.69263343296167079, 40.00000000000000711, -10.49242979028127820 ) ) ;
#27717 = FACE_OUTER_BOUND ( 'NONE', #14799, .T. ) ;
#27718 = AXIS2_PLACEMENT_3D ( 'NONE', #15365, #11869, #5295 ) ;
#27719 = CARTESIAN_POINT ( 'NONE',  ( -158.5000000000000284, 1.941065176648555254E-14, 6.999999999999998224 ) ) ;
#27720 = DIRECTION ( 'NONE',  ( 0.000000000000000000, -0.8443279255020200713, 0.5358267949789887741 ) ) ;
#27722 = ORIENTED_EDGE ( 'NONE', *, *, #19445, .F. ) ;
#27721 = CARTESIAN_POINT ( 'NONE',  ( 17.99999999999999645, 75.72520367775197769, -82.78868281115903471 ) ) ;
#27723 = DIRECTION ( 'NONE',  ( 0.000000000000000000, 0.000000000000000000, 1.000000000000000000 ) ) ;
#27724 = CARTESIAN_POINT ( 'NONE',  ( 17.99999999999999645, -108.8684555192045025, -27.12806418649726936 ) ) ;
#27725 = VERTEX_POINT ( 'NONE', #12363 ) ;
#27726 = CARTESIAN_POINT ( 'NONE',  ( 54.85378563033546584, 40.00000000000000000, 7.219977902337870290 ) ) ;
#27727 = CARTESIAN_POINT ( 'NONE',  ( 17.99999999999999645, 0.000000000000000000, 0.000000000000000000 ) ) ;
#27728 = DIRECTION ( 'NONE',  ( -3.996523416598930318E-16, 2.658563593772947863E-15, 1.000000000000000000 ) ) ;
#27729 = ORIENTED_EDGE ( 'NONE', *, *, #4433, .F. ) ;
#27730 = AXIS2_PLACEMENT_3D ( 'NONE', #32364, #29324, #35207 ) ;
#27731 = CARTESIAN_POINT ( 'NONE',  ( 17.99999999999999645, -3.996885678772183592, -120.4346956066682424 ) ) ;
#27732 = DIRECTION ( 'NONE',  ( 0.000000000000000000, 1.599473849036242195E-14, -1.000000000000000000 ) ) ;
#27733 = EDGE_CURVE ( 'NONE', #9792, #3101, #1039, .T. ) ;
#27734 = EDGE_CURVE ( 'NONE', #14255, #14013, #11548, .T. ) ;
#27735 = ORIENTED_EDGE ( 'NONE', *, *, #26099, .F. ) ;
#27736 = DIRECTION ( 'NONE',  ( 0.000000000000000000, -0.7865515558026355825, -0.6175246149462008116 ) ) ;
#27737 = ORIENTED_EDGE ( 'NONE', *, *, #5161, .T. ) ;
#27738 = AXIS2_PLACEMENT_3D ( 'NONE', #39681, #36859, #6963 ) ;
#27739 = AXIS2_PLACEMENT_3D ( 'NONE', #8292, #21647, #34902 ) ;
#27740 = EDGE_CURVE ( 'NONE', #8724, #25091, #30343, .T. ) ;
#27741 = CIRCLE ( 'NONE', #7496, 116.0000000000000000 ) ;
#27742 = CYLINDRICAL_SURFACE ( 'NONE', #31608, 13.59999999999999964 ) ;
#27743 = ORIENTED_EDGE ( 'NONE', *, *, #22623, .T. ) ;
#27744 = AXIS2_PLACEMENT_3D ( 'NONE', #14957, #18897, #22369 ) ;
#27745 = DIRECTION ( 'NONE',  ( 0.000000000000000000, -0.1837495178165775012, 0.9829730996839004531 ) ) ;
#27746 = FACE_OUTER_BOUND ( 'NONE', #26665, .T. ) ;
#27747 = ORIENTED_EDGE ( 'NONE', *, *, #3401, .F. ) ;
#27748 = AXIS2_PLACEMENT_3D ( 'NONE', #33435, #16683, #23431 ) ;
#27749 = CARTESIAN_POINT ( 'NONE',  ( -105.9879088449591933, 17.11489954122026447, -0.3807199291576673361 ) ) ;
#27750 = CARTESIAN_POINT ( 'NONE',  ( 0.000000000000000000, -23.79363200506972476, 27.01597816121638829 ) ) ;
#27751 = VERTEX_POINT ( 'NONE', #13870 ) ;
#27752 = CARTESIAN_POINT ( 'NONE',  ( 17.99999999999999645, -110.3490479609630910, -20.28201389785511211 ) ) ;
#27753 = VECTOR ( 'NONE', #12182, 1000.000000000000000 ) ;
#27754 = CYLINDRICAL_SURFACE ( 'NONE', #37333, 120.5010000000000190 ) ;
#27755 = EDGE_CURVE ( 'NONE', #37926, #36577, #2428, .T. ) ;
#27756 = CARTESIAN_POINT ( 'NONE',  ( 0.000000000000000000, 0.000000000000000000, 0.000000000000000000 ) ) ;
#27757 = CARTESIAN_POINT ( 'NONE',  ( -10.00000000000000000, 0.000000000000000000, 0.000000000000000000 ) ) ;
#27758 = ORIENTED_EDGE ( 'NONE', *, *, #20083, .F. ) ;
#27759 = DIRECTION ( 'NONE',  ( 2.706052175835637734E-17, -1.000000000000000000, -1.107734830738722853E-16 ) ) ;
#27760 = CARTESIAN_POINT ( 'NONE',  ( -10.00000000000000178, 1.543054966925665076E-15, 12.59999999999999964 ) ) ;
#27761 = CARTESIAN_POINT ( 'NONE',  ( 35.10416666475790493, 31.00000000000000355, 2.290744634698880233 ) ) ;
#27762 = ORIENTED_EDGE ( 'NONE', *, *, #9664, .F. ) ;
#27764 = LINE ( 'NONE', #34711, #19300 ) ;
#27763 = DIRECTION ( 'NONE',  ( 0.000000000000000000, 0.000000000000000000, 1.000000000000000000 ) ) ;
#27765 = DIRECTION ( 'NONE',  ( 1.000000000000000000, 0.000000000000000000, 0.000000000000000000 ) ) ;
#27766 = CIRCLE ( 'NONE', #17353, 58.99999999999998579 ) ;
#27767 = VERTEX_POINT ( 'NONE', #26943 ) ;
#27768 = CARTESIAN_POINT ( 'NONE',  ( -10.00000000000000000, 0.000000000000000000, 0.000000000000000000 ) ) ;
#27769 = EDGE_CURVE ( 'NONE', #40629, #32031, #14315, .T. ) ;
#27770 = CARTESIAN_POINT ( 'NONE',  ( 41.10549127292548377, 40.00000000000000000, 20.25863663968860706 ) ) ;
#27771 = CIRCLE ( 'NONE', #2640, 2.500000000000000444 ) ;
#27772 = CARTESIAN_POINT ( 'NONE',  ( 27.80911911934546055, 40.00000000000000000, -47.97225535894359894 ) ) ;
#27773 = AXIS2_PLACEMENT_3D ( 'NONE', #9062, #4936, #31992 ) ;
#27774 = CIRCLE ( 'NONE', #42364, 2.500000000000000444 ) ;
#27775 = CIRCLE ( 'NONE', #31250, 120.5010000000000332 ) ;
#27776 = CARTESIAN_POINT ( 'NONE',  ( 9.000000000000001776, -17.77780072541773748, 114.6296200873375284 ) ) ;
#27777 = CARTESIAN_POINT ( 'NONE',  ( 17.99999999999999645, -46.12538073176424547, 111.3235835452210267 ) ) ;
#27778 = AXIS2_PLACEMENT_3D ( 'NONE', #28433, #28636, #1558 ) ;
#27779 = DIRECTION ( 'NONE',  ( -0.000000000000000000, -0.000000000000000000, 1.000000000000000000 ) ) ;
#27780 = CARTESIAN_POINT ( 'NONE',  ( 103.7695705685756877, -106.4195705685758213, 6.999999999999666933 ) ) ;
#27781 = ORIENTED_EDGE ( 'NONE', *, *, #41281, .T. ) ;
#27782 = CARTESIAN_POINT ( 'NONE',  ( -3.620280825866593055, 40.00000000000000000, 27.53105304817175636 ) ) ;
#27783 = VERTEX_POINT ( 'NONE', #274 ) ;
#27784 = CARTESIAN_POINT ( 'NONE',  ( 17.99999999999999645, 28.62203781743003717, 14.19692359621465094 ) ) ;
#27785 = CARTESIAN_POINT ( 'NONE',  ( -2.712762565639006418, 3.052587955997511759, -3.430618716626627318 ) ) ;
#27786 = ORIENTED_EDGE ( 'NONE', *, *, #9882, .T. ) ;
#27787 = CARTESIAN_POINT ( 'NONE',  ( 9.000000000000001776, -114.1157422997284669, 20.82300072952894610 ) ) ;
#27788 = EDGE_CURVE ( 'NONE', #11794, #27783, #19220, .T. ) ;
#27789 = DIRECTION ( 'NONE',  ( 0.000000000000000000, 0.000000000000000000, 1.000000000000000000 ) ) ;
#27790 = VERTEX_POINT ( 'NONE', #10786 ) ;
#27791 = FACE_OUTER_BOUND ( 'NONE', #13621, .T. ) ;
#27792 = VERTEX_POINT ( 'NONE', #514 ) ;
#27793 = PRODUCT_RELATED_PRODUCT_CATEGORY ( 'part', '', ( #5687 ) ) ;
#27794 = VERTEX_POINT ( 'NONE', #37166 ) ;
#27795 = DIRECTION ( 'NONE',  ( -1.000000000000000000, -0.000000000000000000, -0.000000000000000000 ) ) ;
#27796 = CARTESIAN_POINT ( 'NONE',  ( -4.761419979751499554, 31.00000000000000355, -74.40007767863900767 ) ) ;
#27797 = ORIENTED_EDGE ( 'NONE', *, *, #11076, .T. ) ;
#27798 = CARTESIAN_POINT ( 'NONE',  ( 0.000000000000000000, -115.9750404417044223, 2.406240749597103434 ) ) ;
#27799 = CIRCLE ( 'NONE', #4787, 13.59999999999999787 ) ;
#27800 = AXIS2_PLACEMENT_3D ( 'NONE', #3897, #37723, #4337 ) ;
#27801 = ADVANCED_FACE ( 'NONE', ( #23477 ), #3996, .T. ) ;
#27802 = CYLINDRICAL_SURFACE ( 'NONE', #39327, 20.00000000000000711 ) ;
#27803 = CIRCLE ( 'NONE', #29886, 13.59999999999999964 ) ;
#27804 = EDGE_LOOP ( 'NONE', ( #13337, #32042, #29668, #13597 ) ) ;
#27805 = EDGE_CURVE ( 'NONE', #27156, #33352, #31024, .T. ) ;
#27806 = FACE_OUTER_BOUND ( 'NONE', #1876, .T. ) ;
#27807 = ORIENTED_EDGE ( 'NONE', *, *, #25527, .T. ) ;
#27808 = CARTESIAN_POINT ( 'NONE',  ( 6.309545988805658645, 40.00000000000000000, -94.59213238963913284 ) ) ;
#27809 = EDGE_CURVE ( 'NONE', #6403, #31369, #42145, .T. ) ;
#27811 = DIRECTION ( 'NONE',  ( -0.000000000000000000, 0.000000000000000000, -1.000000000000000000 ) ) ;
#27810 = CARTESIAN_POINT ( 'NONE',  ( 0.000000000000000000, 101.8011932243955613, -55.61040422519224791 ) ) ;
#27812 = DIRECTION ( 'NONE',  ( -1.000000000000000000, -0.000000000000000000, -0.000000000000000000 ) ) ;
#27813 = DIRECTION ( 'NONE',  ( -0.000000000000000000, -0.000000000000000000, -1.000000000000000000 ) ) ;
#27814 = VERTEX_POINT ( 'NONE', #27166 ) ;
#27815 = CARTESIAN_POINT ( 'NONE',  ( 17.99999999999999645, -80.02407177072905142, -78.64108602300026973 ) ) ;
#27816 = DIRECTION ( 'NONE',  ( 1.000000000000000000, 0.000000000000000000, 0.000000000000000000 ) ) ;
#27817 = CARTESIAN_POINT ( 'NONE',  ( 84.89583333414414312, 31.00000000000000000, -5.563236982362012029 ) ) ;
#27818 = CARTESIAN_POINT ( 'NONE',  ( -4.121423858225412573, -12.61643262889541184, -1.199999999999999956 ) ) ;
#27819 = VERTEX_POINT ( 'NONE', #17371 ) ;
#27820 = CARTESIAN_POINT ( 'NONE',  ( 27.10182830755125138, 40.00000000000000000, 1.799748011963437255 ) ) ;
#27821 = ADVANCED_FACE ( 'NONE', ( #720 ), #14079, .T. ) ;
#27822 = VERTEX_POINT ( 'NONE', #17145 ) ;
#27823 = ORIENTED_EDGE ( 'NONE', *, *, #6025, .T. ) ;
#27824 = LINE ( 'NONE', #4429, #1098 ) ;
#27825 = DIRECTION ( 'NONE',  ( -1.000000000000000000, -0.000000000000000000, 0.000000000000000000 ) ) ;
#27826 = VECTOR ( 'NONE', #16952, 1000.000000000000000 ) ;
#27827 = CARTESIAN_POINT ( 'NONE',  ( 22.90854556226710415, -40.05525454449572464, -74.83297477053821467 ) ) ;
#27828 = CIRCLE ( 'NONE', #36854, 120.5010000000000190 ) ;
#27829 = DIRECTION ( 'NONE',  ( -1.000000000000000000, -0.000000000000000000, -0.000000000000000000 ) ) ;
#27830 = VECTOR ( 'NONE', #7464, 1000.000000000000000 ) ;
#27831 = ORIENTED_EDGE ( 'NONE', *, *, #21356, .F. ) ;
#27832 = DIRECTION ( 'NONE',  ( 0.000000000000000000, 0.000000000000000000, 1.000000000000000000 ) ) ;
#27833 = VERTEX_POINT ( 'NONE', #36955 ) ;
#27834 = CARTESIAN_POINT ( 'NONE',  ( 17.99999999999999645, 18.35539002514530793, -110.6858262410707994 ) ) ;
#27835 = CARTESIAN_POINT ( 'NONE',  ( -91.96080130434573618, -35.35525454449571470, 14.45886780445633946 ) ) ;
#27836 = CARTESIAN_POINT ( 'NONE',  ( 0.000000000000000000, 40.13512380273970592, 113.6206972269522737 ) ) ;
#27837 = DIRECTION ( 'NONE',  ( -1.000000000000000000, 0.000000000000000000, -0.000000000000000000 ) ) ;
#27838 = ORIENTED_EDGE ( 'NONE', *, *, #8209, .T. ) ;
#27839 = VERTEX_POINT ( 'NONE', #20419 ) ;
#27840 = CARTESIAN_POINT ( 'NONE',  ( 18.00000000000000355, -32.32520163883560826, -34.09746168776070618 ) ) ;
#27841 = EDGE_CURVE ( 'NONE', #28053, #40741, #33681, .T. ) ;
#27842 = DIRECTION ( 'NONE',  ( -1.000000000000000000, -0.000000000000000000, -0.000000000000000000 ) ) ;
#27843 = ORIENTED_EDGE ( 'NONE', *, *, #26157, .F. ) ;
#27845 = VERTEX_POINT ( 'NONE', #16931 ) ;
#27844 = DIRECTION ( 'NONE',  ( 1.000000000000000000, 0.000000000000000000, 0.000000000000000000 ) ) ;
#27846 = CARTESIAN_POINT ( 'NONE',  ( -12.95950413119362743, 31.00000000000000355, 37.95406330259781669 ) ) ;
#27847 = CARTESIAN_POINT ( 'NONE',  ( 18.00000000000000355, -47.49120266317494554, -0.8606222198180160099 ) ) ;
#27848 = ADVANCED_FACE ( 'NONE', ( #37387, #3763 ), #10569, .T. ) ;
#27850 = CARTESIAN_POINT ( 'NONE',  ( 17.99999999999999645, 30.71634675606066267, -8.790889055186230649 ) ) ;
#27849 = CARTESIAN_POINT ( 'NONE',  ( 18.00000000000000355, -37.91532898920940653, 28.61088654061626357 ) ) ;
#27851 = UNCERTAINTY_MEASURE_WITH_UNIT (LENGTH_MEASURE( 1.000000000000000082E-05 ), #39575, 'distance_accuracy_value', 'NONE');
#27852 = ORIENTED_EDGE ( 'NONE', *, *, #2840, .T. ) ;
#27853 = DIRECTION ( 'NONE',  ( -0.000000000000000000, 1.000000000000000000, 1.224646799147353207E-16 ) ) ;
#27854 = CARTESIAN_POINT ( 'NONE',  ( -28.16914340537297434, 40.00000000000000000, -57.36152490105313007 ) ) ;
#27855 = VECTOR ( 'NONE', #10095, 1000.000000000000114 ) ;
#27856 = VECTOR ( 'NONE', #17610, 1000.000000000000000 ) ;
#27857 = CARTESIAN_POINT ( 'NONE',  ( -0.2142857142857142738, -10.49781318335647917, -1.199999999999999956 ) ) ;
#27858 = ADVANCED_FACE ( 'NONE', ( #13218, #26509 ), #39783, .F. ) ;
#27859 = DIRECTION ( 'NONE',  ( 1.000000000000000000, 0.000000000000000000, 0.000000000000000000 ) ) ;
#27860 = VERTEX_POINT ( 'NONE', #6631 ) ;
#27861 = AXIS2_PLACEMENT_3D ( 'NONE', #5897, #33593, #16846 ) ;
#27862 = DIRECTION ( 'NONE',  ( 0.000000000000000000, -0.8993121301712229121, 0.4373073204588476259 ) ) ;
#27863 = ORIENTED_EDGE ( 'NONE', *, *, #36191, .T. ) ;
#27864 = SURFACE_SIDE_STYLE ('',( #17840 ) ) ;
#27865 = CARTESIAN_POINT ( 'NONE',  ( 17.99999999999999645, 0.000000000000000000, 0.000000000000000000 ) ) ;
#27866 = DIRECTION ( 'NONE',  ( 0.000000000000000000, 0.000000000000000000, 1.000000000000000000 ) ) ;
#27867 = CARTESIAN_POINT ( 'NONE',  ( -29.22812062908682051, 31.00000000000000355, 50.62729764625685647 ) ) ;
#27868 = CARTESIAN_POINT ( 'NONE',  ( -80.96080130434580724, -35.35525454449571470, 14.45886780445738395 ) ) ;
#27869 = ORIENTED_EDGE ( 'NONE', *, *, #37480, .T. ) ;
#27870 = ORIENTED_EDGE ( 'NONE', *, *, #29035, .T. ) ;
#27871 = CARTESIAN_POINT ( 'NONE',  ( -29.44516979616424024, 40.00000000000000000, -7.879824757621473275 ) ) ;
#27872 = ADVANCED_FACE ( 'NONE', ( #19997 ), #39833, .F. ) ;
#27873 = ORIENTED_EDGE ( 'NONE', *, *, #25378, .T. ) ;
#27874 = CARTESIAN_POINT ( 'NONE',  ( 17.99999999999999645, 119.7318547011701497, 13.59315897125768124 ) ) ;
#27875 = EDGE_CURVE ( 'NONE', #33033, #32706, #37301, .T. ) ;
#27876 = CARTESIAN_POINT ( 'NONE',  ( -10.00000000000000000, 0.000000000000000000, 0.000000000000000000 ) ) ;
#27877 = CARTESIAN_POINT ( 'NONE',  ( 86.24314314301659579, 31.00000000000000000, -11.24622374123920920 ) ) ;
#27878 = CARTESIAN_POINT ( 'NONE',  ( 77.59064570039033981, 39.99999999999999289, -38.12735739512951483 ) ) ;
#27879 = MANIFOLD_SOLID_BREP ( 'Boss-Extrude4', #35842 ) ;
#27880 = DIRECTION ( 'NONE',  ( -1.000000000000000000, 0.000000000000000000, 0.000000000000000000 ) ) ;
#27881 = ORIENTED_EDGE ( 'NONE', *, *, #14202, .F. ) ;
#27882 = CARTESIAN_POINT ( 'NONE',  ( 2.339412683011424576, -2.055254544495723756, -89.04250581823735899 ) ) ;
#27883 = VERTEX_POINT ( 'NONE', #23907 ) ;
#27884 = AXIS2_PLACEMENT_3D ( 'NONE', #16304, #26545, #33302 ) ;
#27885 = DIRECTION ( 'NONE',  ( 1.000000000000000000, 0.000000000000000000, 0.000000000000000000 ) ) ;
#27886 = AXIS2_PLACEMENT_3D ( 'NONE', #20059, #16781, #7341 ) ;
#27887 = CARTESIAN_POINT ( 'NONE',  ( -10.00000000000000000, 0.000000000000000000, 0.000000000000000000 ) ) ;
#27888 = AXIS2_PLACEMENT_3D ( 'NONE', #19909, #26431, #39701 ) ;
#27890 = VERTEX_POINT ( 'NONE', #37172 ) ;
#27889 = CARTESIAN_POINT ( 'NONE',  ( -17.44537629401976631, 17.11489954122025736, -4.261559264950514958 ) ) ;
#27891 = DIRECTION ( 'NONE',  ( 1.000000000000000000, 0.000000000000000000, 0.000000000000000000 ) ) ;
#27892 = EDGE_LOOP ( 'NONE', ( #20056, #9690, #30716, #6665 ) ) ;
#27893 = DIRECTION ( 'NONE',  ( 0.000000000000000000, -0.2631025642275284238, 0.9647678688145140402 ) ) ;
#27894 = EDGE_CURVE ( 'NONE', #16799, #13177, #3564, .T. ) ;
#27895 = CARTESIAN_POINT ( 'NONE',  ( -55.79431841392906222, 40.00000000000000000, -72.71543055464235294 ) ) ;
#27896 = DIRECTION ( 'NONE',  ( 0.000000000000000000, 0.000000000000000000, 1.000000000000000000 ) ) ;
#27897 = APPLICATION_CONTEXT ( 'automotive_design' ) ;
#27898 = ORIENTED_EDGE ( 'NONE', *, *, #14377, .T. ) ;
#27899 = DIRECTION ( 'NONE',  ( -1.000000000000000000, -0.000000000000000000, -0.000000000000000000 ) ) ;
#27900 = CARTESIAN_POINT ( 'NONE',  ( 0.000000000000000000, 2.357898499370431722, -2.818925648462311528E-15 ) ) ;
#27901 = EDGE_CURVE ( 'NONE', #33403, #27001, #6618, .T. ) ;
#27903 = CARTESIAN_POINT ( 'NONE',  ( 0.000000000000000000, 0.000000000000000000, 0.000000000000000000 ) ) ;
#27902 = CARTESIAN_POINT ( 'NONE',  ( -109.0695705685741785, -106.4195705685773135, 9.999999999999751310 ) ) ;
#27904 = ORIENTED_EDGE ( 'NONE', *, *, #41118, .F. ) ;
#27905 = CARTESIAN_POINT ( 'NONE',  ( -10.00000000000000000, 0.000000000000000000, 0.000000000000000000 ) ) ;
#27906 = EDGE_LOOP ( 'NONE', ( #20116, #41493, #2214, #22579 ) ) ;
#27907 = DIRECTION ( 'NONE',  ( 0.000000000000000000, 0.000000000000000000, 1.000000000000000000 ) ) ;
#27908 = CARTESIAN_POINT ( 'NONE',  ( 37.09854380388319584, 40.00000000000000000, 2.490183985263671129 ) ) ;
#27909 = DIRECTION ( 'NONE',  ( 1.000000000000000000, 0.000000000000000000, -3.273063162220425331E-16 ) ) ;
#27910 = EDGE_CURVE ( 'NONE', #15791, #14923, #1767, .T. ) ;
#27911 = CARTESIAN_POINT ( 'NONE',  ( 17.99999999999999645, 73.78980555658732499, -95.26571049921918188 ) ) ;
#27912 = EDGE_CURVE ( 'NONE', #26032, #19113, #28283, .T. ) ;
#27913 = DIRECTION ( 'NONE',  ( 1.000000000000000000, 0.000000000000000000, 0.000000000000000000 ) ) ;
#27914 = VERTEX_POINT ( 'NONE', #6861 ) ;
#27916 = DIRECTION ( 'NONE',  ( 1.000000000000000000, 0.000000000000000000, 0.000000000000000000 ) ) ;
#27915 = DIRECTION ( 'NONE',  ( 0.000000000000000000, 0.000000000000000000, -1.000000000000000000 ) ) ;
#27917 = ORIENTED_EDGE ( 'NONE', *, *, #21276, .F. ) ;
#27918 = CIRCLE ( 'NONE', #15371, 120.5010000000000190 ) ;
#27919 = CARTESIAN_POINT ( 'NONE',  ( 17.99999999999999645, -76.48293397876315680, 82.08917884620285577 ) ) ;
#27920 = CARTESIAN_POINT ( 'NONE',  ( 18.00000000000000355, 15.49408907645234201, -44.90087086784576087 ) ) ;
#27921 = CIRCLE ( 'NONE', #34170, 59.00000000000000000 ) ;
#27923 = CARTESIAN_POINT ( 'NONE',  ( -18.92511213055653130, 31.00000000000000355, 21.58621387822740090 ) ) ;
#27922 = AXIS2_PLACEMENT_3D ( 'NONE', #11153, #24483, #20788 ) ;
#27924 = EDGE_LOOP ( 'NONE', ( #4092, #17178, #41003, #23437 ) ) ;
#27925 = CARTESIAN_POINT ( 'NONE',  ( 17.99999999999999645, -87.92975456462855277, -69.68953103478244770 ) ) ;
#27926 = LINE ( 'NONE', #13967, #39742 ) ;
#27927 = DIRECTION ( 'NONE',  ( -1.000000000000000000, -0.000000000000000000, -0.000000000000000000 ) ) ;
#27928 = CARTESIAN_POINT ( 'NONE',  ( -26.42126989340051324, 31.00000000000000355, -77.78956226056263290 ) ) ;
#27929 = EDGE_CURVE ( 'NONE', #38358, #35775, #24125, .T. ) ;
#27930 = EDGE_CURVE ( 'NONE', #32170, #10324, #4220, .T. ) ;
#27931 = EDGE_LOOP ( 'NONE', ( #13940, #39006 ) ) ;
#27932 = CARTESIAN_POINT ( 'NONE',  ( 3.791180027291366716, 31.00000000000000355, 59.39995347152935778 ) ) ;
#27933 = EDGE_CURVE ( 'NONE', #12068, #41700, #16936, .T. ) ;
#27934 = EDGE_CURVE ( 'NONE', #24013, #4177, #9915, .T. ) ;
#27935 = EDGE_CURVE ( 'NONE', #35201, #4402, #36573, .T. ) ;
#27936 = CARTESIAN_POINT ( 'NONE',  ( -55.79431841392906222, 40.00000000000000000, -72.71543055464235294 ) ) ;
#27937 = CYLINDRICAL_SURFACE ( 'NONE', #13694, 13.60000000000000142 ) ;
#27938 = VECTOR ( 'NONE', #30317, 1000.000000000000000 ) ;
#27939 = DIRECTION ( 'NONE',  ( -1.000000000000000000, -0.000000000000000000, -0.000000000000000000 ) ) ;
#27940 = CYLINDRICAL_SURFACE ( 'NONE', #1004, 120.5010000000000190 ) ;
#27942 = ORIENTED_EDGE ( 'NONE', *, *, #7405, .T. ) ;
#27941 = CARTESIAN_POINT ( 'NONE',  ( 0.000000000000000000, 109.1131968883995000, 26.12628443612074847 ) ) ;
#27943 = CARTESIAN_POINT ( 'NONE',  ( 17.99999999999999645, 59.47573314508867526, -99.59235496188547643 ) ) ;
#27944 = AXIS2_PLACEMENT_3D ( 'NONE', #8462, #32030, #31821 ) ;
#27945 = CARTESIAN_POINT ( 'NONE',  ( 0.000000000000000000, -11.46872990052412788, 45.56340405422441364 ) ) ;
#27946 = VERTEX_POINT ( 'NONE', #13650 ) ;
#27947 = CARTESIAN_POINT ( 'NONE',  ( 61.18335543008118549, 39.99999999999999289, -20.78249587198964576 ) ) ;
#27948 = LINE ( 'NONE', #30770, #19431 ) ;
#27949 = ORIENTED_EDGE ( 'NONE', *, *, #13641, .F. ) ;
#27950 = CIRCLE ( 'NONE', #40352, 59.00000000000000711 ) ;
#27951 = DIRECTION ( 'NONE',  ( 0.000000000000000000, -0.9510565162951565288, 0.3090169943749383474 ) ) ;
#27952 = CARTESIAN_POINT ( 'NONE',  ( -10.00000000000000178, 13.40000000000000036, 0.000000000000000000 ) ) ;
#27953 = AXIS2_PLACEMENT_3D ( 'NONE', #24201, #7577, #20937 ) ;
#27954 = ORIENTED_EDGE ( 'NONE', *, *, #4204, .F. ) ;
#27955 = CARTESIAN_POINT ( 'NONE',  ( 17.99999999999999645, 69.72480978690171582, -92.70626138605946664 ) ) ;
#27956 = ORIENTED_EDGE ( 'NONE', *, *, #19119, .T. ) ;
#27957 = EDGE_CURVE ( 'NONE', #21604, #4304, #22039, .T. ) ;
#27958 = DIRECTION ( 'NONE',  ( -1.000000000000000000, 0.000000000000000000, 0.000000000000000000 ) ) ;
#27959 = ORIENTED_EDGE ( 'NONE', *, *, #19066, .F. ) ;
#27960 = CARTESIAN_POINT ( 'NONE',  ( 142.4999999999992895, -3.154162532185255727E-13, -45.00000000000004974 ) ) ;
#27961 = CARTESIAN_POINT ( 'NONE',  ( -6.638544827991894159, 31.00000000000000355, 99.59190654106262741 ) ) ;
#27962 = VERTEX_POINT ( 'NONE', #4886 ) ;
#27963 = DIRECTION ( 'NONE',  ( -1.000000000000000000, -0.000000000000000000, -0.000000000000000000 ) ) ;
#27964 = CARTESIAN_POINT ( 'NONE',  ( 17.99999999999999645, 29.03409033315599075, -12.21509719675360373 ) ) ;
#27965 = ORIENTED_EDGE ( 'NONE', *, *, #2072, .F. ) ;
#27966 = DIRECTION ( 'NONE',  ( -1.000000000000000000, 0.000000000000000000, 0.000000000000000000 ) ) ;
#27967 = DIRECTION ( 'NONE',  ( -1.000000000000000000, 0.000000000000000000, 0.000000000000000000 ) ) ;
#27968 = ORIENTED_EDGE ( 'NONE', *, *, #10204, .F. ) ;
#27969 = CARTESIAN_POINT ( 'NONE',  ( 17.99999999999999645, -110.1579703617964725, -21.29539948940357164 ) ) ;
#27970 = AXIS2_PLACEMENT_3D ( 'NONE', #36083, #41982, #8613 ) ;
#27971 = LINE ( 'NONE', #37321, #505 ) ;
#27972 = ORIENTED_EDGE ( 'NONE', *, *, #6474, .T. ) ;
#27973 = CARTESIAN_POINT ( 'NONE',  ( -106.4195705685748550, 1.999999999999996669, 106.4195705685759776 ) ) ;
#27974 = FACE_OUTER_BOUND ( 'NONE', #3030, .T. ) ;
#27975 = CARTESIAN_POINT ( 'NONE',  ( 42.89889459577944564, 31.00000000000000355, -32.91970121835214513 ) ) ;
#27976 = CIRCLE ( 'NONE', #15435, 5.384454397937118664 ) ;
#27977 = ORIENTED_EDGE ( 'NONE', *, *, #34482, .T. ) ;
#27979 = DIRECTION ( 'NONE',  ( -1.000000000000000000, -0.000000000000000000, -0.000000000000000000 ) ) ;
#27978 = DIRECTION ( 'NONE',  ( 0.000000000000000000, 0.000000000000000000, 1.000000000000000000 ) ) ;
#27980 = CIRCLE ( 'NONE', #33519, 59.00000000000000711 ) ;
#27981 = CARTESIAN_POINT ( 'NONE',  ( 0.000000000000000000, 0.000000000000000000, 0.000000000000000000 ) ) ;
#27982 = EDGE_CURVE ( 'NONE', #15009, #23495, #5262, .T. ) ;
#27983 = ORIENTED_EDGE ( 'NONE', *, *, #41711, .T. ) ;
#27984 = EDGE_CURVE ( 'NONE', #24128, #7783, #4535, .T. ) ;
#27985 = EDGE_CURVE ( 'NONE', #5464, #15814, #27544, .T. ) ;
#27986 = DIRECTION ( 'NONE',  ( -1.000000000000000000, 0.000000000000000000, 0.000000000000000000 ) ) ;
#27987 = CARTESIAN_POINT ( 'NONE',  ( 31.73387399974884104, 40.00000000000000000, -54.96645564127986461 ) ) ;
#27988 = CARTESIAN_POINT ( 'NONE',  ( -3.469229457552012619, 40.00000000000000000, -54.39987425098301799 ) ) ;
#27989 = ADVANCED_FACE ( 'NONE', ( #41081 ), #1387, .F. ) ;
#27990 = CIRCLE ( 'NONE', #2155, 116.0000000000000000 ) ;
#27991 = DIRECTION ( 'NONE',  ( -1.058513553088275437E-16, -1.000000000000000000, 8.813324511995299047E-17 ) ) ;
#27992 = LINE ( 'NONE', #27777, #22865 ) ;
#27993 = CARTESIAN_POINT ( 'NONE',  ( 0.000000000000000000, 0.000000000000000000, 0.000000000000000000 ) ) ;
#27994 = CARTESIAN_POINT ( 'NONE',  ( 17.99999999999999645, -104.0201923570372173, -51.34003878071168003 ) ) ;
#27995 = ORIENTED_EDGE ( 'NONE', *, *, #3346, .F. ) ;
#27996 = CARTESIAN_POINT ( 'NONE',  ( -27.62299686580952240, 40.00000000000000000, -13.61136854378590577 ) ) ;
#27997 = ORIENTED_EDGE ( 'NONE', *, *, #37930, .T. ) ;
#27998 = DIRECTION ( 'NONE',  ( -1.000000000000000000, 0.000000000000000000, 0.000000000000000000 ) ) ;
#27999 = FACE_OUTER_BOUND ( 'NONE', #14611, .T. ) ;
#28000 = ORIENTED_EDGE ( 'NONE', *, *, #2848, .T. ) ;
#28001 = CYLINDRICAL_SURFACE ( 'NONE', #30556, 59.00000000000000000 ) ;
#28002 = CARTESIAN_POINT ( 'NONE',  ( 0.000000000000000000, 9.744342220504043084, -46.48873837489787064 ) ) ;
#28003 = ORIENTED_EDGE ( 'NONE', *, *, #4329, .F. ) ;
#28004 = DIRECTION ( 'NONE',  ( -1.000000000000000000, 0.000000000000000000, 0.000000000000000000 ) ) ;
#28005 = VERTEX_POINT ( 'NONE', #24566 ) ;
#28006 = ORIENTED_EDGE ( 'NONE', *, *, #5908, .T. ) ;
#28007 = FACE_OUTER_BOUND ( 'NONE', #23642, .T. ) ;
#28008 = AXIS2_PLACEMENT_3D ( 'NONE', #12598, #6451, #15669 ) ;
#28009 = CARTESIAN_POINT ( 'NONE',  ( 51.69257347811147696, 31.00000000000000355, 59.10123636506271083 ) ) ;
#28010 = ORIENTED_EDGE ( 'NONE', *, *, #2518, .T. ) ;
#28011 = DIRECTION ( 'NONE',  ( 0.000000000000000000, 0.000000000000000000, 1.000000000000000000 ) ) ;
#28012 = CIRCLE ( 'NONE', #9167, 58.99999999999998579 ) ;
#28013 = DIRECTION ( 'NONE',  ( 3.009274222672345096E-17, 1.000000000000000000, -2.455023325076454960E-18 ) ) ;
#28014 = VERTEX_POINT ( 'NONE', #31078 ) ;
#28015 = CARTESIAN_POINT ( 'NONE',  ( -4.197393957002303999, -7.773935952363655451E-14, -3.503767560748929810 ) ) ;
#28016 = VERTEX_POINT ( 'NONE', #38461 ) ;
#28017 = CARTESIAN_POINT ( 'NONE',  ( -73.90312034494817794, 40.00000000000000711, -56.84521418463217657 ) ) ;
#28018 = CIRCLE ( 'NONE', #15475, 52.00000000000000000 ) ;
#28019 = CARTESIAN_POINT ( 'NONE',  ( 22.27703560431448793, 31.00000000000000355, 17.12883495622356023 ) ) ;
#28021 = CARTESIAN_POINT ( 'NONE',  ( 17.99999999999999645, -9.484061862023704492, -30.03730300138991538 ) ) ;
#28020 = CARTESIAN_POINT ( 'NONE',  ( 9.000000000000001776, -51.93417535146739539, -2.615612846549718817 ) ) ;
#28022 = DIRECTION ( 'NONE',  ( -1.000000000000000000, -0.000000000000000000, -0.000000000000000000 ) ) ;
#28023 = CYLINDRICAL_SURFACE ( 'NONE', #40275, 126.0000000000000284 ) ;
#28024 = ORIENTED_EDGE ( 'NONE', *, *, #33563, .F. ) ;
#28025 = FILL_AREA_STYLE_COLOUR ( '', #7191 ) ;
#28026 = DIRECTION ( 'NONE',  ( 1.000000000000000000, 0.000000000000000000, 0.000000000000000000 ) ) ;
#28027 = ORIENTED_EDGE ( 'NONE', *, *, #29125, .T. ) ;
#28028 = CARTESIAN_POINT ( 'NONE',  ( 17.99999999999999645, -88.56657216608570593, -68.87840567546012949 ) ) ;
#28029 = CARTESIAN_POINT ( 'NONE',  ( 2.100000000000000089, 0.000000000000000000, -5.000000000000000000 ) ) ;
#28030 = CARTESIAN_POINT ( 'NONE',  ( 17.99999999999999645, -56.51398178981889941, 96.92493144647428949 ) ) ;
#28031 = ORIENTED_EDGE ( 'NONE', *, *, #411, .F. ) ;
#28032 = EDGE_CURVE ( 'NONE', #38476, #30500, #32417, .T. ) ;
#28033 = CARTESIAN_POINT ( 'NONE',  ( 17.33436897218374639, 40.00000000000000000, 22.64673195036553111 ) ) ;
#28034 = ADVANCED_FACE ( 'NONE', ( #14953 ), #1168, .T. ) ;
#28035 = CIRCLE ( 'NONE', #32888, 120.5010000000000474 ) ;
#28036 = ORIENTED_EDGE ( 'NONE', *, *, #1849, .F. ) ;
#28037 = CIRCLE ( 'NONE', #19664, 31.49899999999999878 ) ;
#28038 = VERTEX_POINT ( 'NONE', #11449 ) ;
#28039 = PLANE ( 'NONE',  #15077 ) ;
#28040 = DIRECTION ( 'NONE',  ( 1.000000000000000000, 0.000000000000000000, 0.000000000000000000 ) ) ;
#28041 = DIRECTION ( 'NONE',  ( 1.000000000000000000, 0.000000000000000000, 0.000000000000000000 ) ) ;
#28042 = CARTESIAN_POINT ( 'NONE',  ( 8.999999999999998224, 48.55277268144325120, 105.3500273609081432 ) ) ;
#28043 = EDGE_CURVE ( 'NONE', #14260, #6747, #27611, .T. ) ;
#28044 = ORIENTED_EDGE ( 'NONE', *, *, #41032, .F. ) ;
#28045 = DIRECTION ( 'NONE',  ( -0.000000000000000000, -0.000000000000000000, -1.000000000000000000 ) ) ;
#28046 = ORIENTED_EDGE ( 'NONE', *, *, #35981, .T. ) ;
#28047 = DIRECTION ( 'NONE',  ( 0.2140725878556618555, -0.9768177553304301375, -2.795573601670286284E-15 ) ) ;
#28048 = AXIS2_PLACEMENT_3D ( 'NONE', #19276, #29292, #12504 ) ;
#28049 = CYLINDRICAL_SURFACE ( 'NONE', #43018, 12.59999999999999964 ) ;
#28050 = EDGE_CURVE ( 'NONE', #5213, #1664, #5317, .T. ) ;
#28051 = DIRECTION ( 'NONE',  ( 0.000000000000000000, 0.9048270524660205760, -0.4257792915650702170 ) ) ;
#28052 = DIRECTION ( 'NONE',  ( 1.000000000000000000, 0.000000000000000000, 0.000000000000000000 ) ) ;
#28053 = VERTEX_POINT ( 'NONE', #18688 ) ;
#28054 = ORIENTED_EDGE ( 'NONE', *, *, #26401, .T. ) ;
#28055 = DIRECTION ( 'NONE',  ( -1.000000000000000000, 0.000000000000000000, 0.000000000000000000 ) ) ;
#28056 = DIRECTION ( 'NONE',  ( 0.000000000000000000, 0.000000000000000000, 1.000000000000000000 ) ) ;
#28057 = ORIENTED_EDGE ( 'NONE', *, *, #35712, .F. ) ;
#28059 = ORIENTED_EDGE ( 'NONE', *, *, #5132, .T. ) ;
#28058 = DIRECTION ( 'NONE',  ( -1.000000000000000000, -0.000000000000000000, 0.000000000000000000 ) ) ;
#28060 = CARTESIAN_POINT ( 'NONE',  ( 10.06970066534735331, 31.00000000000000355, 37.84957806120349488 ) ) ;
#28061 = DIRECTION ( 'NONE',  ( -3.996523416598930318E-16, 2.658563593772947863E-15, 1.000000000000000000 ) ) ;
#28063 = CARTESIAN_POINT ( 'NONE',  ( 17.99999999999999645, -7.220349212960190499, -35.26849241522671718 ) ) ;
#28062 = DIRECTION ( 'NONE',  ( 1.000000000000000000, 0.000000000000000000, 0.000000000000000000 ) ) ;
#28064 = ORIENTED_EDGE ( 'NONE', *, *, #42956, .F. ) ;
#28065 = AXIS2_PLACEMENT_3D ( 'NONE', #31644, #41444, #1742 ) ;
#28066 = DIRECTION ( 'NONE',  ( 0.000000000000000000, 0.000000000000000000, 1.000000000000000000 ) ) ;
#28067 = CARTESIAN_POINT ( 'NONE',  ( 51.26988013557343749, 40.00000000000000000, 45.10883117380814866 ) ) ;
#28068 = CIRCLE ( 'NONE', #34984, 120.5010000000000190 ) ;
#28069 = DIRECTION ( 'NONE',  ( -3.996523416598930318E-16, 2.658563593772947863E-15, 1.000000000000000000 ) ) ;
#28070 = AXIS2_PLACEMENT_3D ( 'NONE', #20499, #40070, #14159 ) ;
#28071 = DIRECTION ( 'NONE',  ( 0.000000000000000000, -0.5963673585384914322, -0.8027116379309710004 ) ) ;
#28072 = ORIENTED_EDGE ( 'NONE', *, *, #17600, .F. ) ;
#28073 = DIRECTION ( 'NONE',  ( -1.000000000000000000, 0.000000000000000000, -0.000000000000000000 ) ) ;
#28074 = ORIENTED_EDGE ( 'NONE', *, *, #19674, .T. ) ;
#28075 = CIRCLE ( 'NONE', #14843, 0.08000000000000020983 ) ;
#28076 = DIRECTION ( 'NONE',  ( 0.000000000000000000, 0.000000000000000000, 1.000000000000000000 ) ) ;
#28077 = DIRECTION ( 'NONE',  ( -1.000000000000000000, -0.000000000000000000, -0.000000000000000000 ) ) ;
#28078 = CARTESIAN_POINT ( 'NONE',  ( -48.53848235557606472, 31.00000000000000355, -37.22912483484027035 ) ) ;
#28079 = CARTESIAN_POINT ( 'NONE',  ( 17.99999999999999645, 87.92975456462995965, -69.68953103478068556 ) ) ;
#28080 = ORIENTED_EDGE ( 'NONE', *, *, #42423, .T. ) ;
#28081 = EDGE_CURVE ( 'NONE', #17165, #22037, #28257, .T. ) ;
#28082 = EDGE_CURVE ( 'NONE', #2217, #1510, #34532, .T. ) ;
#28083 = SURFACE_STYLE_FILL_AREA ( #8417 ) ;
#28084 = ORIENTED_EDGE ( 'NONE', *, *, #22373, .F. ) ;
#28085 = DIRECTION ( 'NONE',  ( 0.000000000000000000, 0.000000000000000000, 1.000000000000000000 ) ) ;
#28086 = DIRECTION ( 'NONE',  ( 0.000000000000000000, -0.3140767120219362663, -0.9493976084683853900 ) ) ;
#28087 = CARTESIAN_POINT ( 'NONE',  ( -65.95487968126425926, 31.00000000000000711, -50.74205456613862708 ) ) ;
#28088 = CARTESIAN_POINT ( 'NONE',  ( -78.26717753304431824, 40.00000000000000711, -26.69481836930730978 ) ) ;
#28089 = CARTESIAN_POINT ( 'NONE',  ( 0.000000000000000000, 97.89532456239497549, 54.81585448086229917 ) ) ;
#28090 = ADVANCED_FACE ( 'NONE', ( #1818 ), #11674, .T. ) ;
#28091 = CIRCLE ( 'NONE', #21833, 58.99999999999999289 ) ;
#28092 = VERTEX_POINT ( 'NONE', #8373 ) ;
#28093 = DIRECTION ( 'NONE',  ( 1.000000000000000000, 1.836909530733573776E-16, 0.000000000000000000 ) ) ;
#28094 = EDGE_LOOP ( 'NONE', ( #27004, #1914, #26190, #13807 ) ) ;
#28095 = EDGE_CURVE ( 'NONE', #40305, #9994, #38257, .T. ) ;
#28096 = DIRECTION ( 'NONE',  ( 0.000000000000000000, -0.4610925014493326146, 0.8873520750565681015 ) ) ;
#28097 = CIRCLE ( 'NONE', #5765, 120.5010000000000332 ) ;
#28099 = ORIENTED_EDGE ( 'NONE', *, *, #25812, .T. ) ;
#28098 = DIRECTION ( 'NONE',  ( 0.000000000000000000, 0.000000000000000000, -1.000000000000000000 ) ) ;
#28100 = CARTESIAN_POINT ( 'NONE',  ( 0.000000000000000000, -32.32520163883560826, -34.09746168776070618 ) ) ;
#28101 = ORIENTED_EDGE ( 'NONE', *, *, #42207, .F. ) ;
#28102 = DIRECTION ( 'NONE',  ( -1.000000000000000000, -0.000000000000000000, 0.000000000000000000 ) ) ;
#28103 = CARTESIAN_POINT ( 'NONE',  ( -68.67288961433401084, 40.00000000000000711, -60.22678404055071155 ) ) ;
#28104 = DIRECTION ( 'NONE',  ( -1.000000000000000000, -0.000000000000000000, 0.000000000000000000 ) ) ;
#28105 = ORIENTED_EDGE ( 'NONE', *, *, #33012, .F. ) ;
#28106 = CYLINDRICAL_SURFACE ( 'NONE', #37372, 14.70000000000000107 ) ;
#28107 = CARTESIAN_POINT ( 'NONE',  ( 8.919999999999996376, 1.827173024327850982E-15, -14.91999999999999815 ) ) ;
#28108 = EDGE_CURVE ( 'NONE', #69, #42811, #35246, .T. ) ;
#28110 = LINE ( 'NONE', #41375, #40794 ) ;
#28109 = CARTESIAN_POINT ( 'NONE',  ( -106.4195705685741871, -106.4195705685773135, 6.999999999999754863 ) ) ;
#28111 = ORIENTED_EDGE ( 'NONE', *, *, #20, .F. ) ;
#28112 = DIRECTION ( 'NONE',  ( 1.000000000000000000, 0.000000000000000000, 0.000000000000000000 ) ) ;
#28114 = VERTEX_POINT ( 'NONE', #4665 ) ;
#28113 = ADVANCED_FACE ( 'NONE', ( #31723 ), #40870, .F. ) ;
#28115 = DIRECTION ( 'NONE',  ( 1.000000000000000000, 0.000000000000000000, 0.000000000000000000 ) ) ;
#28116 = CARTESIAN_POINT ( 'NONE',  ( -7.793954689940647995, 40.00000000000000000, 28.94896179907301459 ) ) ;
#28117 = CARTESIAN_POINT ( 'NONE',  ( 17.99999999999999645, 115.5737863835463628, -9.934782381632540904 ) ) ;
#28118 = ADVANCED_FACE ( 'NONE', ( #31302 ), #14734, .T. ) ;
#28119 = DIRECTION ( 'NONE',  ( 0.000000000000000000, -0.5264321628773449557, -0.8502171357296209875 ) ) ;
#28120 = CARTESIAN_POINT ( 'NONE',  ( 0.000000000000000000, 0.000000000000000000, 0.000000000000000000 ) ) ;
#28121 = ORIENTED_EDGE ( 'NONE', *, *, #6366, .F. ) ;
#28123 = FACE_OUTER_BOUND ( 'NONE', #29897, .T. ) ;
#28122 = CARTESIAN_POINT ( 'NONE',  ( 130.0000000000000000, -2.127378845942280309E-13, 2.000000000000031530 ) ) ;
#28124 = ORIENTED_EDGE ( 'NONE', *, *, #23667, .T. ) ;
#28125 = AXIS2_PLACEMENT_3D ( 'NONE', #33724, #768, #19814 ) ;
#28126 = DIRECTION ( 'NONE',  ( 0.000000000000000000, -0.7525707698561306946, -0.6585113790650474197 ) ) ;
#28127 = CARTESIAN_POINT ( 'NONE',  ( -10.00000000000000000, 0.000000000000000000, 0.000000000000000000 ) ) ;
#28128 = CARTESIAN_POINT ( 'NONE',  ( 21.81281596512078025, 31.00000000000000355, -10.76194779073239083 ) ) ;
#28129 = ORIENTED_EDGE ( 'NONE', *, *, #4821, .T. ) ;
#28130 = FACE_OUTER_BOUND ( 'NONE', #42198, .T. ) ;
#28131 = LINE ( 'NONE', #29153, #2542 ) ;
#28132 = LINE ( 'NONE', #21832, #32354 ) ;
#28133 = CARTESIAN_POINT ( 'NONE',  ( -79.89583333417640176, 31.00000000000000711, 5.235987747608064957 ) ) ;
#28134 = VERTEX_POINT ( 'NONE', #5732 ) ;
#28135 = CARTESIAN_POINT ( 'NONE',  ( 18.91139405008774688, 31.00000000000000355, 55.99505798891475195 ) ) ;
#28136 = CARTESIAN_POINT ( 'NONE',  ( 89.65113856817994531, 39.99999999999999289, -30.44896562292877462 ) ) ;
#28137 = EDGE_CURVE ( 'NONE', #21211, #967, #17161, .T. ) ;
#28138 = VECTOR ( 'NONE', #40351, 1000.000000000000000 ) ;
#28139 = EDGE_CURVE ( 'NONE', #25754, #20175, #3173, .T. ) ;
#28140 = EDGE_LOOP ( 'NONE', ( #17213, #32808, #37832, #9350 ) ) ;
#28141 = DIRECTION ( 'NONE',  ( -1.000000000000000000, -0.000000000000000000, -0.000000000000000000 ) ) ;
#28142 = DIRECTION ( 'NONE',  ( 1.000000000000000000, 0.000000000000000000, 0.000000000000000000 ) ) ;
#28143 = EDGE_CURVE ( 'NONE', #27141, #15184, #3137, .T. ) ;
#28144 = CARTESIAN_POINT ( 'NONE',  ( -101.9145453900123641, 31.00000000000000355, -1.407535261550449501 ) ) ;
#28145 = CIRCLE ( 'NONE', #911, 52.00000000000000000 ) ;
#28147 = ORIENTED_EDGE ( 'NONE', *, *, #17656, .T. ) ;
#28146 = CARTESIAN_POINT ( 'NONE',  ( 9.000000000000000000, -6.007673836298252468, 35.49518073029994980 ) ) ;
#28148 = DIRECTION ( 'NONE',  ( 1.000000000000000000, 0.000000000000000000, 0.000000000000000000 ) ) ;
#28149 = CARTESIAN_POINT ( 'NONE',  ( 18.00000000000000355, 36.34385289850590794, 29.77717097092089205 ) ) ;
#28150 = CIRCLE ( 'NONE', #26731, 31.49899999999999523 ) ;
#28151 = VERTEX_POINT ( 'NONE', #22365 ) ;
#28152 = CARTESIAN_POINT ( 'NONE',  ( 64.89583333437747115, 39.99999999999999289, -4.254240043327834009 ) ) ;
#28153 = DIRECTION ( 'NONE',  ( 1.000000000000000000, -1.373900992973643249E-15, -5.551115123125812284E-16 ) ) ;
#28154 = ORIENTED_EDGE ( 'NONE', *, *, #3051, .F. ) ;
#28155 = CYLINDRICAL_SURFACE ( 'NONE', #1529, 1.000000000000000444 ) ;
#28156 = CYLINDRICAL_SURFACE ( 'NONE', #34024, 59.00000000000000000 ) ;
#28157 = MANIFOLD_SOLID_BREP ( 'EndChamfer', #6570 ) ;
#28158 = ORIENTED_EDGE ( 'NONE', *, *, #1519, .F. ) ;
#28159 = CYLINDRICAL_SURFACE ( 'NONE', #27739, 120.5010000000000190 ) ;
#28160 = ORIENTED_EDGE ( 'NONE', *, *, #15251, .T. ) ;
#28161 = STYLED_ITEM ( 'NONE', ( #22773 ), #35926 ) ;
#28162 = CARTESIAN_POINT ( 'NONE',  ( 9.999999999999998224, 1.641026710857453510E-15, 13.40000000000000213 ) ) ;
#28163 = CIRCLE ( 'NONE', #16321, 47.49900000000000233 ) ;
#28164 = ORIENTED_EDGE ( 'NONE', *, *, #27472, .T. ) ;
#28165 = CARTESIAN_POINT ( 'NONE',  ( 9.000000000000001776, 31.17727234463694330, 111.7317219465820983 ) ) ;
#28166 = CARTESIAN_POINT ( 'NONE',  ( 0.000000000000000000, 40.37724737310206535, -104.6802291180863023 ) ) ;
#28167 = ORIENTED_EDGE ( 'NONE', *, *, #14526, .T. ) ;
#28168 = EDGE_CURVE ( 'NONE', #37962, #3822, #26888, .T. ) ;
#28169 = DIRECTION ( 'NONE',  ( 1.000000000000000000, 0.000000000000000000, 0.000000000000000000 ) ) ;
#28170 = CARTESIAN_POINT ( 'NONE',  ( 17.99999999999999645, -41.62036691425453228, -113.0850832732718914 ) ) ;
#28172 = VERTEX_POINT ( 'NONE', #30119 ) ;
#28171 = AXIS2_PLACEMENT_3D ( 'NONE', #21161, #20946, #40516 ) ;
#28173 = CARTESIAN_POINT ( 'NONE',  ( 17.99999999999999645, 0.000000000000000000, 0.000000000000000000 ) ) ;
#28174 = AXIS2_PLACEMENT_3D ( 'NONE', #2278, #28943, #42850 ) ;
#28175 = CARTESIAN_POINT ( 'NONE',  ( 18.00000000000000355, 0.000000000000000000, 0.000000000000000000 ) ) ;
#28176 = VERTEX_POINT ( 'NONE', #25840 ) ;
#28177 = LINE ( 'NONE', #38397, #21841 ) ;
#28178 = AXIS2_PLACEMENT_3D ( 'NONE', #34224, #36849, #30957 ) ;
#28179 = FACE_OUTER_BOUND ( 'NONE', #27238, .T. ) ;
#28180 = APPLICATION_PROTOCOL_DEFINITION ( 'draft international standard', 'automotive_design', 1998, #15353 ) ;
#28181 = EDGE_CURVE ( 'NONE', #23479, #13925, #28314, .T. ) ;
#28183 = AXIS2_PLACEMENT_3D ( 'NONE', #21424, #1501, #21195 ) ;
#28182 = CYLINDRICAL_SURFACE ( 'NONE', #39957, 20.00000000000001066 ) ;
#28184 = CARTESIAN_POINT ( 'NONE',  ( -32.14164714139042189, 31.00000000000000355, 36.65395011347077059 ) ) ;
#28185 = EDGE_LOOP ( 'NONE', ( #15231, #12233, #12964, #4773 ) ) ;
#28187 = DIRECTION ( 'NONE',  ( 1.000000000000000000, -1.373900992973641868E-15, -6.546126324440886161E-16 ) ) ;
#28186 = CARTESIAN_POINT ( 'NONE',  ( 0.000000000000000000, 0.000000000000000000, 0.000000000000000000 ) ) ;
#28188 = ORIENTED_EDGE ( 'NONE', *, *, #37060, .T. ) ;
#28189 = CARTESIAN_POINT ( 'NONE',  ( 0.000000000000000000, 0.000000000000000000, 0.000000000000000000 ) ) ;
#28190 = CARTESIAN_POINT ( 'NONE',  ( 53.64558601427197004, 40.00000000000000000, 14.36188897069615500 ) ) ;
#28191 = AXIS2_PLACEMENT_3D ( 'NONE', #1966, #28614, #15105 ) ;
#28192 = CARTESIAN_POINT ( 'NONE',  ( 33.95200755731382714, 40.00000000000000000, -44.10258293181757949 ) ) ;
#28193 = ADVANCED_FACE ( 'NONE', ( #9223 ), #6753, .F. ) ;
#28194 = AXIS2_PLACEMENT_3D ( 'NONE', #17969, #28415, #27978 ) ;
#28195 = CYLINDRICAL_SURFACE ( 'NONE', #17264, 2.500000000000000444 ) ;
#28196 = DIRECTION ( 'NONE',  ( -1.000000000000000000, 0.000000000000000000, 0.000000000000000000 ) ) ;
#28197 = ADVANCED_FACE ( 'NONE', ( #15388 ), #33848, .T. ) ;
#28198 = CLOSED_SHELL ( 'NONE', ( #9093, #21304, #7170, #6264, #35763, #2279, #36203, #35817, #25925, #17910, #6786, #24133, #16279, #843, #28866, #31956, #23909, #34898, #2843, #35453, #15260, #20811 ) ) ;
#28199 = CARTESIAN_POINT ( 'NONE',  ( 0.000000000000000000, 92.10690493017145286, -64.06707842432085442 ) ) ;
#28200 = AXIS2_PLACEMENT_3D ( 'NONE', #26806, #19216, #6085 ) ;
#28201 = FACE_OUTER_BOUND ( 'NONE', #14004, .T. ) ;
#28202 = CIRCLE ( 'NONE', #10041, 120.5010000000000190 ) ;
#28203 = ORIENTED_EDGE ( 'NONE', *, *, #14629, .T. ) ;
#28204 = CARTESIAN_POINT ( 'NONE',  ( 34.89583333524210218, 40.00000000000000000, -2.290744634698907767 ) ) ;
#28205 = EDGE_LOOP ( 'NONE', ( #23220, #354, #24690, #487 ) ) ;
#28206 = DIRECTION ( 'NONE',  ( -1.000000000000000000, -0.000000000000000000, -0.000000000000000000 ) ) ;
#28207 = DIRECTION ( 'NONE',  ( -3.009274222672345096E-17, -1.000000000000000000, 2.455023325076455345E-18 ) ) ;
#28208 = AXIS2_PLACEMENT_3D ( 'NONE', #7401, #3069, #16443 ) ;
#28209 = EDGE_LOOP ( 'NONE', ( #30718, #33378, #6820, #1987 ) ) ;
#28210 = EDGE_CURVE ( 'NONE', #15422, #15847, #15750, .T. ) ;
#28211 = CYLINDRICAL_SURFACE ( 'NONE', #35395, 24.99999999999999289 ) ;
#28212 = AXIS2_PLACEMENT_3D ( 'NONE', #11330, #41842, #21407 ) ;
#28213 = FACE_OUTER_BOUND ( 'NONE', #8508, .T. ) ;
#28214 = ORIENTED_EDGE ( 'NONE', *, *, #38394, .T. ) ;
#28215 = DIRECTION ( 'NONE',  ( 0.000000000000000000, 0.000000000000000000, 1.000000000000000000 ) ) ;
#28216 = ORIENTED_EDGE ( 'NONE', *, *, #13847, .T. ) ;
#28217 = AXIS2_PLACEMENT_3D ( 'NONE', #30923, #24416, #7788 ) ;
#28218 = ORIENTED_EDGE ( 'NONE', *, *, #27248, .T. ) ;
#28219 = LINE ( 'NONE', #41486, #4166 ) ;
#28220 = EDGE_CURVE ( 'NONE', #25590, #40845, #23415, .T. ) ;
#28221 = CARTESIAN_POINT ( 'NONE',  ( 17.81064159971323946, 31.00000000000000355, 66.89829513328324140 ) ) ;
#28222 = ORIENTED_EDGE ( 'NONE', *, *, #14435, .F. ) ;
#28223 = CARTESIAN_POINT ( 'NONE',  ( -4.197477534772231955, 0.8522413273724368521, -3.505042416683225692 ) ) ;
#28224 = EDGE_CURVE ( 'NONE', #43124, #8862, #10886, .T. ) ;
#28225 = EDGE_CURVE ( 'NONE', #12969, #29749, #7373, .T. ) ;
#28226 = EDGE_CURVE ( 'NONE', #38713, #2041, #16835, .T. ) ;
#28227 = CARTESIAN_POINT ( 'NONE',  ( 8.999999999999998224, 35.89808275599445153, -2.706964063997355119 ) ) ;
#28228 = EDGE_LOOP ( 'NONE', ( #34350, #15683 ) ) ;
#28230 = AXIS2_PLACEMENT_3D ( 'NONE', #23047, #3115, #16486 ) ;
#28229 = DIRECTION ( 'NONE',  ( -1.000000000000000000, 0.000000000000000000, 0.000000000000000000 ) ) ;
#28231 = VERTEX_POINT ( 'NONE', #9016 ) ;
#28232 = CARTESIAN_POINT ( 'NONE',  ( -92.09225407318750456, 40.00000000000000711, -6.144973693751363264 ) ) ;
#28233 = CARTESIAN_POINT ( 'NONE',  ( 7.507699080471219588, 31.00000000000000355, 28.16210111025598195 ) ) ;
#28235 = CARTESIAN_POINT ( 'NONE',  ( 17.99999999999999645, 0.000000000000000000, 0.000000000000000000 ) ) ;
#28234 = DIRECTION ( 'NONE',  ( 0.000000000000000000, 0.000000000000000000, 1.000000000000000000 ) ) ;
#28236 = CIRCLE ( 'NONE', #4521, 13.59999999999999964 ) ;
#28237 = DIRECTION ( 'NONE',  ( 0.000000000000000000, 0.000000000000000000, 1.000000000000000000 ) ) ;
#28238 = CARTESIAN_POINT ( 'NONE',  ( 9.000000000000001776, 47.31079789947627745, -105.9135893174946119 ) ) ;
#28239 = ORIENTED_EDGE ( 'NONE', *, *, #14242, .T. ) ;
#28240 = CIRCLE ( 'NONE', #21285, 59.00000000000000000 ) ;
#28241 = DIRECTION ( 'NONE',  ( 0.000000000000000000, 0.000000000000000000, 1.000000000000000000 ) ) ;
#28242 = ORIENTED_EDGE ( 'NONE', *, *, #11311, .T. ) ;
#28243 = AXIS2_PLACEMENT_3D ( 'NONE', #35719, #2557, #15920 ) ;
#28244 = DIRECTION ( 'NONE',  ( 1.000000000000000000, 0.000000000000000000, 0.000000000000000000 ) ) ;
#28245 = CARTESIAN_POINT ( 'NONE',  ( 86.04713929520032423, 31.00000000000000000, 42.41619695850760507 ) ) ;
#28246 = CIRCLE ( 'NONE', #5231, 116.0000000000000000 ) ;
#28247 = CARTESIAN_POINT ( 'NONE',  ( 17.99999999999999645, -19.47322409167291113, 30.27859877001394295 ) ) ;
#28248 = ORIENTED_EDGE ( 'NONE', *, *, #41591, .F. ) ;
#28249 = CIRCLE ( 'NONE', #37954, 116.0000000000000000 ) ;
#28250 = CARTESIAN_POINT ( 'NONE',  ( -18.31940394017777862, 40.00000000000000000, -14.05611420671344014 ) ) ;
#28251 = AXIS2_PLACEMENT_3D ( 'NONE', #3779, #16734, #40008 ) ;
#28252 = EDGE_LOOP ( 'NONE', ( #26468, #13529, #19627, #34959 ) ) ;
#28253 = ORIENTED_EDGE ( 'NONE', *, *, #1358, .F. ) ;
#28254 = LINE ( 'NONE', #35193, #38051 ) ;
#28255 = DIRECTION ( 'NONE',  ( 1.000000000000000000, 0.000000000000000000, 0.000000000000000000 ) ) ;
#28256 = EDGE_CURVE ( 'NONE', #33331, #36755, #16469, .T. ) ;
#28257 = LINE ( 'NONE', #11233, #40810 ) ;
#28258 = LINE ( 'NONE', #28042, #23321 ) ;
#28259 = VERTEX_POINT ( 'NONE', #4110 ) ;
#28260 = LINE ( 'NONE', #34992, #31933 ) ;
#28261 = ORIENTED_EDGE ( 'NONE', *, *, #30523, .T. ) ;
#28262 = DIRECTION ( 'NONE',  ( -1.000000000000000000, 0.000000000000000000, 0.000000000000000000 ) ) ;
#28263 = AXIS2_PLACEMENT_3D ( 'NONE', #661, #10067, #23847 ) ;
#28264 = CARTESIAN_POINT ( 'NONE',  ( 9.000000000000001776, 115.6826031496113529, -8.575274253896266075 ) ) ;
#28265 = CARTESIAN_POINT ( 'NONE',  ( 18.00000000000000355, -32.00046193115124282, -34.40241257139720688 ) ) ;
#28266 =( GEOMETRIC_REPRESENTATION_CONTEXT ( 3 ) GLOBAL_UNCERTAINTY_ASSIGNED_CONTEXT ( ( #42237 ) ) GLOBAL_UNIT_ASSIGNED_CONTEXT ( ( #1625, #2629, #21328 ) ) REPRESENTATION_CONTEXT ( 'NONE', 'WORKASPACE' ) );
#28267 = DIRECTION ( 'NONE',  ( 0.000000000000000000, 0.000000000000000000, -1.000000000000000000 ) ) ;
#28268 = VERTEX_POINT ( 'NONE', #30966 ) ;
#28269 = CIRCLE ( 'NONE', #33803, 120.5010000000000474 ) ;
#28270 = ORIENTED_EDGE ( 'NONE', *, *, #33981, .T. ) ;
#28271 = DIRECTION ( 'NONE',  ( -1.000000000000000000, 0.000000000000000000, 0.000000000000000000 ) ) ;
#28272 = AXIS2_PLACEMENT_3D ( 'NONE', #28449, #11861, #19270 ) ;
#28273 = DIRECTION ( 'NONE',  ( 0.000000000000000000, 1.000000000000000000, 0.000000000000000000 ) ) ;
#28274 = AXIS2_PLACEMENT_3D ( 'NONE', #32246, #23111, #29416 ) ;
#28275 = ORIENTED_EDGE ( 'NONE', *, *, #41992, .F. ) ;
#28276 = VECTOR ( 'NONE', #10779, 1000.000000000000000 ) ;
#28278 = ORIENTED_EDGE ( 'NONE', *, *, #29830, .T. ) ;
#28277 = DIRECTION ( 'NONE',  ( -1.000000000000000000, -0.000000000000000000, 0.000000000000000000 ) ) ;
#28279 = CARTESIAN_POINT ( 'NONE',  ( 11.72132095739929625, 31.00000000000000355, -43.45763713126748229 ) ) ;
#28280 = VECTOR ( 'NONE', #28775, 1000.000000000000000 ) ;
#28281 = EDGE_LOOP ( 'NONE', ( #37107, #41427, #20191, #7084 ) ) ;
#28282 = CARTESIAN_POINT ( 'NONE',  ( 17.99999999999999645, 18.42432724429518842, -30.92804820215982886 ) ) ;
#28283 = CIRCLE ( 'NONE', #7339, 20.00000000000000355 ) ;
#28284 = EDGE_CURVE ( 'NONE', #18858, #28923, #30374, .T. ) ;
#28285 = EDGE_CURVE ( 'NONE', #22037, #30654, #14348, .T. ) ;
#28287 = CARTESIAN_POINT ( 'NONE',  ( 0.000000000000000000, 76.48293397876260258, 82.08917884620340999 ) ) ;
#28286 = CYLINDRICAL_SURFACE ( 'NONE', #25223, 20.00000000000000711 ) ;
#28288 = EDGE_CURVE ( 'NONE', #24752, #39291, #42178, .T. ) ;
#28289 = AXIS2_PLACEMENT_3D ( 'NONE', #35829, #5547, #15597 ) ;
#28290 = ORIENTED_EDGE ( 'NONE', *, *, #34136, .T. ) ;
#28291 = DIRECTION ( 'NONE',  ( -1.000000000000000000, -0.000000000000000000, -0.000000000000000000 ) ) ;
#28292 = CARTESIAN_POINT ( 'NONE',  ( 16.92944795087012722, 40.00000000000000000, -62.81076020707057950 ) ) ;
#28293 = DIRECTION ( 'NONE',  ( 0.000000000000000000, -0.9968120070307509017, 0.07978610555307336094 ) ) ;
#28294 = DIRECTION ( 'NONE',  ( 1.000000000000000000, 0.000000000000000000, 0.000000000000000000 ) ) ;
#28295 = EDGE_LOOP ( 'NONE', ( #480, #15534, #3529, #14264 ) ) ;
#28296 = CARTESIAN_POINT ( 'NONE',  ( -17.44537629401976275, 40.00000000000000000, 4.261559264950522063 ) ) ;
#28297 = VERTEX_POINT ( 'NONE', #40543 ) ;
#28298 = DIRECTION ( 'NONE',  ( -1.000000000000000000, -0.000000000000000000, -0.000000000000000000 ) ) ;
#28299 = CARTESIAN_POINT ( 'NONE',  ( 0.000000000000000000, 0.000000000000000000, -1.199999999999999956 ) ) ;
#28300 = EDGE_CURVE ( 'NONE', #170, #17739, #4565, .T. ) ;
#28301 = CARTESIAN_POINT ( 'NONE',  ( -61.47519263390311295, 31.00000000000000711, -35.49250405583519807 ) ) ;
#28302 = CARTESIAN_POINT ( 'NONE',  ( 18.00000000000000355, 0.000000000000000000, 0.000000000000000000 ) ) ;
#28303 = AXIS2_PLACEMENT_3D ( 'NONE', #34969, #28022, #31703 ) ;
#28304 = VERTEX_POINT ( 'NONE', #10679 ) ;
#28305 = VECTOR ( 'NONE', #38121, 1000.000000000000000 ) ;
#28306 = VECTOR ( 'NONE', #32750, 1000.000000000000000 ) ;
#28307 = CIRCLE ( 'NONE', #31774, 13.40000000000000213 ) ;
#28308 = DIRECTION ( 'NONE',  ( 0.000000000000000000, 3.645859508832611499E-14, -1.000000000000000000 ) ) ;
#28309 = EDGE_LOOP ( 'NONE', ( #21066, #6692 ) ) ;
#28311 = CIRCLE ( 'NONE', #5292, 58.99999999999999289 ) ;
#28310 = DIRECTION ( 'NONE',  ( -1.000000000000000000, -0.000000000000000000, -0.000000000000000000 ) ) ;
#28312 = DIRECTION ( 'NONE',  ( -1.000000000000000000, -0.000000000000000000, 0.000000000000000000 ) ) ;
#28313 = CARTESIAN_POINT ( 'NONE',  ( -62.56443097448101298, 31.00000000000000355, -55.02758207457566897 ) ) ;
#28315 = CARTESIAN_POINT ( 'NONE',  ( -74.30604906370724905, 40.00000000000000711, -36.76128443489604791 ) ) ;
#28314 = CIRCLE ( 'NONE', #17862, 139.4999999999992610 ) ;
#28316 = LINE ( 'NONE', #21582, #29271 ) ;
#28317 = EDGE_CURVE ( 'NONE', #12545, #35437, #10139, .T. ) ;
#28318 = AXIS2_PLACEMENT_3D ( 'NONE', #34089, #4393, #24527 ) ;
#28319 = ORIENTED_EDGE ( 'NONE', *, *, #19653, .T. ) ;
#28320 = DIRECTION ( 'NONE',  ( 0.000000000000000000, 0.000000000000000000, 1.000000000000000000 ) ) ;
#28321 = ORIENTED_EDGE ( 'NONE', *, *, #20020, .F. ) ;
#28322 = DIRECTION ( 'NONE',  ( -1.000000000000000000, 0.000000000000000000, -0.000000000000000000 ) ) ;
#28324 = ORIENTED_EDGE ( 'NONE', *, *, #21126, .F. ) ;
#28323 = FACE_OUTER_BOUND ( 'NONE', #29551, .T. ) ;
#28325 = CARTESIAN_POINT ( 'NONE',  ( 0.000000000000000000, 23.21237537461745859, 109.7700237000592836 ) ) ;
#28326 = ORIENTED_EDGE ( 'NONE', *, *, #10848, .F. ) ;
#28327 = DIRECTION ( 'NONE',  ( -1.000000000000000000, -0.000000000000000000, -0.000000000000000000 ) ) ;
#28328 = CARTESIAN_POINT ( 'NONE',  ( -6.381360069252544953, 40.00000000000000000, 97.60416666604666602 ) ) ;
#28329 = DIRECTION ( 'NONE',  ( 1.000000000000000000, 1.836909530733573776E-16, 0.000000000000000000 ) ) ;
#28330 = ORIENTED_EDGE ( 'NONE', *, *, #7567, .F. ) ;
#28331 = CARTESIAN_POINT ( 'NONE',  ( -15.99999999999997691, 31.00000000000000355, 5.571627607371296764E-15 ) ) ;
#28332 = FACE_OUTER_BOUND ( 'NONE', #36431, .T. ) ;
#28333 = AXIS2_PLACEMENT_3D ( 'NONE', #35720, #16574, #39205 ) ;
#28334 = EDGE_CURVE ( 'NONE', #19047, #35963, #24840, .T. ) ;
#28335 = AXIS2_PLACEMENT_3D ( 'NONE', #35962, #6941, #20301 ) ;
#28336 = VECTOR ( 'NONE', #16064, 1000.000000000000000 ) ;
#28338 = CARTESIAN_POINT ( 'NONE',  ( 0.000000000000000000, -43.83938735307280865, 18.28286404005783083 ) ) ;
#28337 = CARTESIAN_POINT ( 'NONE',  ( 0.000000000000000000, 17.33727698085173330, 110.8498592715974098 ) ) ;
#28339 = ORIENTED_EDGE ( 'NONE', *, *, #14931, .F. ) ;
#28340 = CARTESIAN_POINT ( 'NONE',  ( 17.99999999999999645, -34.78944633786285578, 9.257128253673503337 ) ) ;
#28341 = ORIENTED_EDGE ( 'NONE', *, *, #27240, .F. ) ;
#28342 = DIRECTION ( 'NONE',  ( -1.000000000000000000, 0.000000000000000000, 0.000000000000000000 ) ) ;
#28343 = CARTESIAN_POINT ( 'NONE',  ( 12.72035051019986618, 40.00000000000000000, 25.87482915247129966 ) ) ;
#28344 = CIRCLE ( 'NONE', #18583, 139.5000000000000000 ) ;
#28345 = FACE_OUTER_BOUND ( 'NONE', #9251, .T. ) ;
#28346 = PRESENTATION_LAYER_ASSIGNMENT (  '', '', ( #40113 ) ) ;
#28347 = EDGE_CURVE ( 'NONE', #33317, #30585, #5331, .T. ) ;
#28348 = CARTESIAN_POINT ( 'NONE',  ( 17.99999999999999645, -46.83041522348565167, 101.9567785075599744 ) ) ;
#28349 = DIRECTION ( 'NONE',  ( 0.000000000000000000, 0.000000000000000000, 1.000000000000000000 ) ) ;
#28350 = ORIENTED_EDGE ( 'NONE', *, *, #14875, .F. ) ;
#28351 = CARTESIAN_POINT ( 'NONE',  ( 2.807080416178989513, -3.225969019225150003, -3.502507215260505014 ) ) ;
#28352 = EDGE_CURVE ( 'NONE', #5962, #10039, #38731, .T. ) ;
#28354 = ORIENTED_EDGE ( 'NONE', *, *, #41282, .F. ) ;
#28353 = AXIS2_PLACEMENT_3D ( 'NONE', #37247, #30084, #37470 ) ;
#28355 = FACE_OUTER_BOUND ( 'NONE', #9247, .T. ) ;
#28356 = CARTESIAN_POINT ( 'NONE',  ( 17.99999999999999645, -62.45178862086279992, 93.20969140437486544 ) ) ;
#28357 = EDGE_CURVE ( 'NONE', #18949, #41859, #10173, .T. ) ;
#28358 = CARTESIAN_POINT ( 'NONE',  ( -9.824444021593908616, 31.00000000000000355, 36.70529466175499778 ) ) ;
#28359 = VERTEX_POINT ( 'NONE', #33795 ) ;
#28360 = DIRECTION ( 'NONE',  ( -1.000000000000000000, 0.000000000000000000, 0.000000000000000000 ) ) ;
#28361 = VECTOR ( 'NONE', #39349, 1000.000000000000000 ) ;
#28362 = CARTESIAN_POINT ( 'NONE',  ( 2.500000000000000888, 3.061616997868384127E-16, -4.974599999999998801 ) ) ;
#28363 = CARTESIAN_POINT ( 'NONE',  ( -51.96644965834242669, 31.00000000000000711, 59.25555446696338890 ) ) ;
#28365 = ORIENTED_EDGE ( 'NONE', *, *, #3078, .T. ) ;
#28364 = AXIS2_PLACEMENT_3D ( 'NONE', #13020, #29585, #29174 ) ;
#28366 = CARTESIAN_POINT ( 'NONE',  ( -17.30549157494827384, 31.00000000000000355, -51.24895740946764988 ) ) ;
#28367 = CARTESIAN_POINT ( 'NONE',  ( -6.054110834496889026, 40.00000000000000000, -92.39583333400220511 ) ) ;
#28368 = CIRCLE ( 'NONE', #33905, 20.00000000000000355 ) ;
#28369 = CIRCLE ( 'NONE', #2517, 52.00000000000000000 ) ;
#28370 = ORIENTED_EDGE ( 'NONE', *, *, #33158, .F. ) ;
#28371 = EDGE_CURVE ( 'NONE', #12884, #28770, #30758, .T. ) ;
#28372 = AXIS2_PLACEMENT_3D ( 'NONE', #5092, #25636, #34550 ) ;
#28373 = CARTESIAN_POINT ( 'NONE',  ( -6.599999999999994316, 4.619827469794975478E-15, 0.000000000000000000 ) ) ;
#28374 = DIRECTION ( 'NONE',  ( -3.996523416598930318E-16, 2.658563593772947863E-15, 1.000000000000000000 ) ) ;
#28375 = CARTESIAN_POINT ( 'NONE',  ( 0.000000000000000000, -42.60732521687585006, 19.80331771201644031 ) ) ;
#28377 = VERTEX_POINT ( 'NONE', #40334 ) ;
#28376 = DIRECTION ( 'NONE',  ( 0.000000000000000000, 1.505387152034110654E-14, -1.000000000000000000 ) ) ;
#28378 = CYLINDRICAL_SURFACE ( 'NONE', #28183, 59.00000000000000000 ) ;
#28379 = LINE ( 'NONE', #38161, #29306 ) ;
#28380 = AXIS2_PLACEMENT_3D ( 'NONE', #13093, #42938, #3216 ) ;
#28381 = VERTEX_POINT ( 'NONE', #37072 ) ;
#28382 = CARTESIAN_POINT ( 'NONE',  ( 4.090615425948669781, 40.00000000000000000, -62.60416666561555132 ) ) ;
#28383 = CARTESIAN_POINT ( 'NONE',  ( 17.99999999999999645, -57.40245293794601622, -96.40140491896693220 ) ) ;
#28384 = ORIENTED_EDGE ( 'NONE', *, *, #12742, .T. ) ;
#28385 = CARTESIAN_POINT ( 'NONE',  ( 9.000000000000001776, -35.11945359308084136, -38.34871548466050228 ) ) ;
#28386 = CARTESIAN_POINT ( 'NONE',  ( 0.000000000000000000, 0.000000000000000000, 0.000000000000000000 ) ) ;
#28387 = CARTESIAN_POINT ( 'NONE',  ( -10.00000000000000000, 0.000000000000000000, 0.000000000000000000 ) ) ;
#28388 = ORIENTED_EDGE ( 'NONE', *, *, #42958, .T. ) ;
#28389 = EDGE_CURVE ( 'NONE', #23370, #34135, #17272, .T. ) ;
#28390 = ORIENTED_EDGE ( 'NONE', *, *, #11595, .T. ) ;
#28391 = CYLINDRICAL_SURFACE ( 'NONE', #37196, 65.00000000000000000 ) ;
#28392 = ORIENTED_EDGE ( 'NONE', *, *, #878, .T. ) ;
#28393 = DIRECTION ( 'NONE',  ( 0.000000000000000000, 0.000000000000000000, 1.000000000000000000 ) ) ;
#28394 = DIRECTION ( 'NONE',  ( -1.000000000000000000, 0.000000000000000000, -0.000000000000000000 ) ) ;
#28395 = CIRCLE ( 'NONE', #6089, 4.500000000000000888 ) ;
#28396 = DIRECTION ( 'NONE',  ( 0.000000000000000000, 0.000000000000000000, 1.000000000000000000 ) ) ;
#28397 = DIRECTION ( 'NONE',  ( 0.000000000000000000, 0.000000000000000000, 1.000000000000000000 ) ) ;
#28398 = ORIENTED_EDGE ( 'NONE', *, *, #33637, .F. ) ;
#28399 = AXIS2_PLACEMENT_3D ( 'NONE', #8800, #35613, #22364 ) ;
#28400 = DIRECTION ( 'NONE',  ( -1.000000000000000000, -0.000000000000000000, -0.000000000000000000 ) ) ;
#28401 = EDGE_CURVE ( 'NONE', #18333, #4714, #8780, .T. ) ;
#28402 = CIRCLE ( 'NONE', #9558, 13.59999999999999787 ) ;
#28403 = AXIS2_PLACEMENT_3D ( 'NONE', #6323, #10414, #13709 ) ;
#28405 = CARTESIAN_POINT ( 'NONE',  ( 17.99999999999999645, -35.54274411427983438, -115.1399337407609949 ) ) ;
#28404 = AXIS2_PLACEMENT_3D ( 'NONE', #13887, #4448, #34352 ) ;
#28406 = EDGE_LOOP ( 'NONE', ( #9547, #6448, #33502, #30929 ) ) ;
#28407 = DIRECTION ( 'NONE',  ( 1.000000000000000000, -0.000000000000000000, -0.000000000000000000 ) ) ;
#28408 = AXIS2_PLACEMENT_3D ( 'NONE', #74, #14297, #10137 ) ;
#28409 = DIRECTION ( 'NONE',  ( -1.000000000000000000, 0.000000000000000000, 0.000000000000000000 ) ) ;
#28410 = CARTESIAN_POINT ( 'NONE',  ( 106.4195705685763471, 17.99999999999998934, 106.4195705685744855 ) ) ;
#28411 = CIRCLE ( 'NONE', #9569, 59.00000000000000711 ) ;
#28412 = CARTESIAN_POINT ( 'NONE',  ( 0.000000000000000000, -1.178949249685218748, -2.041999999999998039 ) ) ;
#28413 = CARTESIAN_POINT ( 'NONE',  ( -47.99616210117395099, 31.00000000000000355, 12.86278070621785119 ) ) ;
#28414 = ORIENTED_EDGE ( 'NONE', *, *, #20698, .T. ) ;
#28416 = DIRECTION ( 'NONE',  ( 0.000000000000000000, 0.000000000000000000, 1.000000000000000000 ) ) ;
#28415 = DIRECTION ( 'NONE',  ( -1.000000000000000000, -0.000000000000000000, -0.000000000000000000 ) ) ;
#28417 = ORIENTED_EDGE ( 'NONE', *, *, #87, .T. ) ;
#28418 = CARTESIAN_POINT ( 'NONE',  ( -54.58798567973315841, 40.00000000000000000, -26.90590473539369754 ) ) ;
#28419 = CARTESIAN_POINT ( 'NONE',  ( -56.33579487689732446, 40.00000000000000000, -27.88694065509425357 ) ) ;
#28420 = ADVANCED_FACE ( 'NONE', ( #619 ), #27937, .T. ) ;
#28421 = DIRECTION ( 'NONE',  ( 0.000000000000000000, 0.7865515558026436871, -0.6175246149461902645 ) ) ;
#28422 = DIRECTION ( 'NONE',  ( 0.000000000000000000, 0.000000000000000000, 1.000000000000000000 ) ) ;
#28423 = EDGE_CURVE ( 'NONE', #19384, #30604, #8100, .T. ) ;
#28424 = AXIS2_PLACEMENT_3D ( 'NONE', #11898, #25226, #34564 ) ;
#28425 = DIRECTION ( 'NONE',  ( -1.000000000000000000, -0.000000000000000000, 0.000000000000000000 ) ) ;
#28426 = CARTESIAN_POINT ( 'NONE',  ( 2.965790448435745574, 31.00000000000000355, -22.56328348808469997 ) ) ;
#28427 = VECTOR ( 'NONE', #31858, 1000.000000000000000 ) ;
#28428 = ORIENTED_EDGE ( 'NONE', *, *, #36402, .T. ) ;
#28429 = CARTESIAN_POINT ( 'NONE',  ( 35.10416666475790493, 40.00000000000000000, 2.290744634698880233 ) ) ;
#28430 = EDGE_LOOP ( 'NONE', ( #33909, #20048, #32223, #16342 ) ) ;
#28431 = VECTOR ( 'NONE', #40795, 1000.000000000000000 ) ;
#28432 = CYLINDRICAL_SURFACE ( 'NONE', #21537, 13.59999999999999964 ) ;
#28433 = CARTESIAN_POINT ( 'NONE',  ( 17.99999999999999645, 0.000000000000000000, 0.000000000000000000 ) ) ;
#28434 = AXIS2_PLACEMENT_3D ( 'NONE', #40929, #37663, #34181 ) ;
#28435 = ORIENTED_EDGE ( 'NONE', *, *, #30450, .F. ) ;
#28436 = AXIS2_PLACEMENT_3D ( 'NONE', #22801, #23016, #18900 ) ;
#28437 = DIRECTION ( 'NONE',  ( 0.000000000000000000, 0.3641605752528230266, -0.9313361774523382097 ) ) ;
#28438 = LINE ( 'NONE', #29438, #15087 ) ;
#28439 = ORIENTED_EDGE ( 'NONE', *, *, #27374, .T. ) ;
#28440 = CARTESIAN_POINT ( 'NONE',  ( 4.000000000000000000, 2.309401076758497151, -3.433295621305379353 ) ) ;
#28441 = ORIENTED_EDGE ( 'NONE', *, *, #8602, .T. ) ;
#28442 = EDGE_CURVE ( 'NONE', #36927, #3403, #33196, .T. ) ;
#28443 = ORIENTED_EDGE ( 'NONE', *, *, #40167, .F. ) ;
#28444 = DIRECTION ( 'NONE',  ( -1.000000000000000000, -0.000000000000000000, -0.000000000000000000 ) ) ;
#28445 = AXIS2_PLACEMENT_3D ( 'NONE', #27693, #33561, #3648 ) ;
#28446 = CARTESIAN_POINT ( 'NONE',  ( 25.34170449640226508, 31.00000000000000355, 74.97748276543396173 ) ) ;
#28447 = ORIENTED_EDGE ( 'NONE', *, *, #5491, .F. ) ;
#28448 = CARTESIAN_POINT ( 'NONE',  ( -4.000000000000000000, -0.8232339106130515116, -3.430630286862743183 ) ) ;
#28449 = CARTESIAN_POINT ( 'NONE',  ( 17.99999999999999645, 11.41303419184972689, 111.6154788735836405 ) ) ;
#28450 = VERTEX_POINT ( 'NONE', #20763 ) ;
#28451 = DIRECTION ( 'NONE',  ( -3.009274222672345096E-17, -1.000000000000000000, 2.455023325076454960E-18 ) ) ;
#28452 = EDGE_CURVE ( 'NONE', #17938, #10707, #34021, .T. ) ;
#28453 = DIRECTION ( 'NONE',  ( 0.000000000000000000, 1.000000000000000000, -1.224646799147353207E-16 ) ) ;
#28454 = CARTESIAN_POINT ( 'NONE',  ( -101.9959696149863788, 40.00000000000000711, -0.1269066430510139010 ) ) ;
#28455 = ADVANCED_FACE ( 'NONE', ( #17694, #14406, #27717 ), #28790, .T. ) ;
#28456 = AXIS2_PLACEMENT_3D ( 'NONE', #9183, #1777, #41910 ) ;
#28458 = DIRECTION ( 'NONE',  ( 0.000000000000000000, 0.000000000000000000, -1.000000000000000000 ) ) ;
#28457 = CARTESIAN_POINT ( 'NONE',  ( 17.99999999999999645, 0.000000000000000000, 0.000000000000000000 ) ) ;
#28459 = CARTESIAN_POINT ( 'NONE',  ( 17.99999999999999645, 46.12538073176347808, 111.3235835452212825 ) ) ;
#28460 = CARTESIAN_POINT ( 'NONE',  ( 0.000000000000000000, -107.5680526044921947, 31.89649718262059608 ) ) ;
#28461 = AXIS2_PLACEMENT_3D ( 'NONE', #32098, #13544, #6324 ) ;
#28462 = ORIENTED_EDGE ( 'NONE', *, *, #10671, .T. ) ;
#28463 = CIRCLE ( 'NONE', #27773, 20.00000000000001066 ) ;
#28464 = SURFACE_STYLE_FILL_AREA ( #12297 ) ;
#28465 = CIRCLE ( 'NONE', #15242, 100.0000000000000711 ) ;
#28466 = DIRECTION ( 'NONE',  ( 0.000000000000000000, -0.5528000653612000770, 0.8333139190825105125 ) ) ;
#28467 = VECTOR ( 'NONE', #3362, 1000.000000000000000 ) ;
#28468 = EDGE_LOOP ( 'NONE', ( #30573, #16461, #24210, #3023 ) ) ;
#28469 = CARTESIAN_POINT ( 'NONE',  ( 8.999999999999998224, -90.81729652456118629, -72.16798910853708549 ) ) ;
#28470 = CARTESIAN_POINT ( 'NONE',  ( 84.73112319332513209, 31.00000000000000000, -41.78253223598262167 ) ) ;
#28471 = CARTESIAN_POINT ( 'NONE',  ( 9.000000000000001776, 24.47917365149946534, 45.87777302070942653 ) ) ;
#28473 = ORIENTED_EDGE ( 'NONE', *, *, #13122, .F. ) ;
#28472 = AXIS2_PLACEMENT_3D ( 'NONE', #12057, #15757, #39055 ) ;
#28474 = CARTESIAN_POINT ( 'NONE',  ( 25.13348990051749965, 40.00000000000000000, -8.510361017570636122 ) ) ;
#28475 = ORIENTED_EDGE ( 'NONE', *, *, #28050, .F. ) ;
#28476 = ADVANCED_FACE ( 'NONE', ( #5632 ), #12206, .T. ) ;
#28477 = ORIENTED_EDGE ( 'NONE', *, *, #24741, .F. ) ;
#28478 = DIRECTION ( 'NONE',  ( -1.000000000000000000, 0.000000000000000000, 0.000000000000000000 ) ) ;
#28479 = CARTESIAN_POINT ( 'NONE',  ( 0.000000000000000000, 21.55123232222474172, 118.5581519187672654 ) ) ;
#28480 = ADVANCED_FACE ( 'NONE', ( #31406 ), #42050, .F. ) ;
#28481 = CARTESIAN_POINT ( 'NONE',  ( 17.99999999999999645, -88.56657216608662964, 68.87840567545892156 ) ) ;
#28482 = CIRCLE ( 'NONE', #19418, 47.49900000000000233 ) ;
#28483 = EDGE_CURVE ( 'NONE', #25300, #42489, #24878, .T. ) ;
#28484 = ADVANCED_FACE ( 'NONE', ( #11999, #28581 ), #8919, .T. ) ;
#28485 = FACE_BOUND ( 'NONE', #1092, .T. ) ;
#28486 = CARTESIAN_POINT ( 'NONE',  ( 17.99999999999999645, 35.89808275599445153, 2.706964063997355119 ) ) ;
#28487 = ORIENTED_EDGE ( 'NONE', *, *, #5677, .T. ) ;
#28488 = CARTESIAN_POINT ( 'NONE',  ( 17.99999999999999645, 19.69434969228073484, 24.58291258574055860 ) ) ;
#28489 = VERTEX_POINT ( 'NONE', #22268 ) ;
#28490 = CARTESIAN_POINT ( 'NONE',  ( 0.000000000000000000, 30.01658535635262481, 108.1077105353199102 ) ) ;
#28491 = DIRECTION ( 'NONE',  ( -1.000000000000000000, -0.000000000000000000, -0.000000000000000000 ) ) ;
#28492 = AXIS2_PLACEMENT_3D ( 'NONE', #6768, #23380, #20336 ) ;
#28493 = AXIS2_PLACEMENT_3D ( 'NONE', #22060, #38801, #32058 ) ;
#28494 = DIRECTION ( 'NONE',  ( 0.000000000000000000, -0.6845471059286791782, -0.7289686274214204342 ) ) ;
#28495 = CARTESIAN_POINT ( 'NONE',  ( 0.000000000000000000, 41.20225022064636278, 23.63323037071415911 ) ) ;
#28496 = VERTEX_POINT ( 'NONE', #1709 ) ;
#28497 = ORIENTED_EDGE ( 'NONE', *, *, #1749, .T. ) ;
#28498 = DIRECTION ( 'NONE',  ( 0.000000000000000000, 0.000000000000000000, 1.000000000000000000 ) ) ;
#28499 = CIRCLE ( 'NONE', #36792, 120.5010000000000190 ) ;
#28500 = DIRECTION ( 'NONE',  ( -1.000000000000000000, 0.000000000000000000, -0.000000000000000000 ) ) ;
#28501 = AXIS2_PLACEMENT_3D ( 'NONE', #19518, #10082, #13387 ) ;
#28502 = EDGE_LOOP ( 'NONE', ( #3644, #27341, #30783, #7781 ) ) ;
#28504 = ORIENTED_EDGE ( 'NONE', *, *, #32982, .T. ) ;
#28503 = CARTESIAN_POINT ( 'NONE',  ( 1.798435537469519230E-14, -1.196353617197826191E-13, -44.99999999999999289 ) ) ;
#28505 = CARTESIAN_POINT ( 'NONE',  ( 27.80911911935152503, 31.00000000000000355, -47.97225535896787108 ) ) ;
#28506 = ORIENTED_EDGE ( 'NONE', *, *, #34824, .F. ) ;
#28507 = DIRECTION ( 'NONE',  ( 0.000000000000000000, -0.6736956436465479925, -0.7390089172206675272 ) ) ;
#28508 = CARTESIAN_POINT ( 'NONE',  ( 0.000000000000000000, 56.51398178981825993, 96.92493144647468739 ) ) ;
#28509 = EDGE_CURVE ( 'NONE', #30296, #3075, #40843, .T. ) ;
#28510 = VERTEX_POINT ( 'NONE', #35517 ) ;
#28511 = CARTESIAN_POINT ( 'NONE',  ( 57.21690105882998267, 39.99999999999999289, -50.04162206025958426 ) ) ;
#28512 = EDGE_CURVE ( 'NONE', #3798, #38781, #7403, .T. ) ;
#28513 = CYLINDRICAL_SURFACE ( 'NONE', #8141, 13.59999999999999787 ) ;
#28514 = DIRECTION ( 'NONE',  ( -1.000000000000000000, -0.000000000000000000, -0.000000000000000000 ) ) ;
#28515 = ORIENTED_EDGE ( 'NONE', *, *, #681, .T. ) ;
#28516 = DIRECTION ( 'NONE',  ( 0.000000000000000000, 0.000000000000000000, -1.000000000000000000 ) ) ;
#28517 = ORIENTED_EDGE ( 'NONE', *, *, #4140, .F. ) ;
#28518 =( NAMED_UNIT ( * ) SI_UNIT ( $, .STERADIAN. ) SOLID_ANGLE_UNIT ( ) );
#28519 = CARTESIAN_POINT ( 'NONE',  ( 17.99999999999999645, 12.43843445475317822, 111.5058645182329968 ) ) ;
#28520 = DIRECTION ( 'NONE',  ( 0.000000000000000000, 0.000000000000000000, 1.000000000000000000 ) ) ;
#28521 = CARTESIAN_POINT ( 'NONE',  ( 4.417864660711233959, 31.00000000000000355, 67.39583333436242185 ) ) ;
#28522 = CARTESIAN_POINT ( 'NONE',  ( 5.560781378645573980, 6.809993116116507654E-16, -4.000000000000000000 ) ) ;
#28523 = VECTOR ( 'NONE', #82, 1000.000000000000000 ) ;
#28524 = ORIENTED_EDGE ( 'NONE', *, *, #7235, .T. ) ;
#28525 = AXIS2_PLACEMENT_3D ( 'NONE', #27834, #41087, #37824 ) ;
#28526 = ORIENTED_EDGE ( 'NONE', *, *, #28951, .F. ) ;
#28527 = DIRECTION ( 'NONE',  ( -3.996523416598930318E-16, 2.658563593772947863E-15, 1.000000000000000000 ) ) ;
#28528 = DIRECTION ( 'NONE',  ( -1.000000000000000000, -0.000000000000000000, -0.000000000000000000 ) ) ;
#28529 = ADVANCED_FACE ( 'NONE', ( #15063 ), #9122, .T. ) ;
#28530 = CARTESIAN_POINT ( 'NONE',  ( -82.09281090897877675, 31.00000000000000711, -5.486092462564049477 ) ) ;
#28531 = CARTESIAN_POINT ( 'NONE',  ( 56.68048384767583769, 39.99999999999999289, -64.44707192207098956 ) ) ;
#28532 = EDGE_CURVE ( 'NONE', #16968, #16491, #35950, .T. ) ;
#28533 = ADVANCED_FACE ( 'NONE', ( #38999 ), #2331, .F. ) ;
#28534 = DIRECTION ( 'NONE',  ( 1.000000000000000000, 0.000000000000000000, 0.000000000000000000 ) ) ;
#28535 = ADVANCED_FACE ( 'NONE', ( #11788 ), #15698, .T. ) ;
#28536 = ORIENTED_EDGE ( 'NONE', *, *, #39383, .F. ) ;
#28537 = DIRECTION ( 'NONE',  ( 1.000000000000000000, 0.000000000000000000, 0.000000000000000000 ) ) ;
#28538 = ORIENTED_EDGE ( 'NONE', *, *, #21991, .T. ) ;
#28539 = DIRECTION ( 'NONE',  ( -1.000000000000000000, -0.000000000000000000, -0.000000000000000000 ) ) ;
#28540 = LINE ( 'NONE', #25271, #10138 ) ;
#28542 = VERTEX_POINT ( 'NONE', #29000 ) ;
#28541 = LINE ( 'NONE', #31794, #17218 ) ;
#28543 = FACE_OUTER_BOUND ( 'NONE', #24401, .T. ) ;
#28544 = EDGE_LOOP ( 'NONE', ( #39450, #25089 ) ) ;
#28545 = DIRECTION ( 'NONE',  ( 1.000000000000000000, 0.000000000000000000, 0.000000000000000000 ) ) ;
#28546 = CARTESIAN_POINT ( 'NONE',  ( 0.000000000000000000, -82.63181128086679905, -81.41243003647058174 ) ) ;
#28547 = DIRECTION ( 'NONE',  ( 0.000000000000000000, 0.000000000000000000, 1.000000000000000000 ) ) ;
#28548 = ORIENTED_EDGE ( 'NONE', *, *, #17198, .T. ) ;
#28549 = EDGE_CURVE ( 'NONE', #36814, #33745, #42271, .T. ) ;
#28550 = DIRECTION ( 'NONE',  ( 1.000000000000000000, 0.000000000000000000, 0.000000000000000000 ) ) ;
#28551 = CIRCLE ( 'NONE', #9702, 31.49900000000000588 ) ;
#28552 = CARTESIAN_POINT ( 'NONE',  ( 17.99999999999999645, 111.2721026680458749, 14.38025178762809908 ) ) ;
#28553 = AXIS2_PLACEMENT_3D ( 'NONE', #33206, #39938, #6799 ) ;
#28555 = CARTESIAN_POINT ( 'NONE',  ( 42.80287614962790599, -12.05525454449572464, 69.29271901957253021 ) ) ;
#28554 = CARTESIAN_POINT ( 'NONE',  ( 1.798435537469519230E-14, -1.196353617197826191E-13, -44.99999999999999289 ) ) ;
#28556 = ORIENTED_EDGE ( 'NONE', *, *, #11522, .T. ) ;
#28557 = DIRECTION ( 'NONE',  ( 0.000000000000000000, 0.000000000000000000, -1.000000000000000000 ) ) ;
#28558 = ORIENTED_EDGE ( 'NONE', *, *, #11867, .F. ) ;
#28559 = DIRECTION ( 'NONE',  ( 1.000000000000000000, 0.000000000000000000, -6.546126324440850663E-16 ) ) ;
#28560 = CARTESIAN_POINT ( 'NONE',  ( -26.24023198663969580, 40.00000000000000000, -20.19409642360271917 ) ) ;
#28561 = DIRECTION ( 'NONE',  ( 0.000000000000000000, 0.000000000000000000, 1.000000000000000000 ) ) ;
#28562 = LINE ( 'NONE', #8253, #1211 ) ;
#28563 = LINE ( 'NONE', #32442, #36657 ) ;
#28564 = VERTEX_POINT ( 'NONE', #15289 ) ;
#28565 = CARTESIAN_POINT ( 'NONE',  ( 9.000000000000001776, 50.95304419620823921, 10.38206564895679307 ) ) ;
#28566 = EDGE_LOOP ( 'NONE', ( #18881, #29653, #28154, #14317 ) ) ;
#28567 = CARTESIAN_POINT ( 'NONE',  ( 0.000000000000000000, -35.20873326984057883, -31.88259874184068465 ) ) ;
#28568 = DIRECTION ( 'NONE',  ( -1.000000000000000000, -0.000000000000000000, -0.000000000000000000 ) ) ;
#28569 = CARTESIAN_POINT ( 'NONE',  ( 4.888094100070568437, 31.00000000000000355, 37.04995123692341252 ) ) ;
#28570 = ORIENTED_EDGE ( 'NONE', *, *, #25287, .F. ) ;
#28571 = FACE_OUTER_BOUND ( 'NONE', #41440, .T. ) ;
#28572 = DIRECTION ( 'NONE',  ( 0.000000000000000000, 0.000000000000000000, 1.000000000000000000 ) ) ;
#28573 = CARTESIAN_POINT ( 'NONE',  ( 73.00591898829820536, 31.00000000000000000, 19.54754034098114701 ) ) ;
#28574 = CIRCLE ( 'NONE', #16045, 158.4999999999992042 ) ;
#28575 = AXIS2_PLACEMENT_3D ( 'NONE', #30407, #481, #13841 ) ;
#28576 = ORIENTED_EDGE ( 'NONE', *, *, #14600, .F. ) ;
#28577 = CARTESIAN_POINT ( 'NONE',  ( -42.11670055801651102, 31.00000000000000355, -32.42481051985740237 ) ) ;
#28578 = EDGE_CURVE ( 'NONE', #6694, #14987, #22768, .T. ) ;
#28579 = CARTESIAN_POINT ( 'NONE',  ( -54.00384411202717416, 40.00000000000000711, 70.40394205935166383 ) ) ;
#28580 = VERTEX_POINT ( 'NONE', #1494 ) ;
#28581 = FACE_OUTER_BOUND ( 'NONE', #9035, .T. ) ;
#28582 = LINE ( 'NONE', #11559, #30562 ) ;
#28583 = CARTESIAN_POINT ( 'NONE',  ( 17.99999999999999645, 6.486220790508443912, 112.0098273076987567 ) ) ;
#28585 = ORIENTED_EDGE ( 'NONE', *, *, #33274, .T. ) ;
#28584 = DIRECTION ( 'NONE',  ( -1.000000000000000000, -0.000000000000000000, -0.000000000000000000 ) ) ;
#28586 = DIRECTION ( 'NONE',  ( 1.000000000000000000, -0.000000000000000000, -0.000000000000000000 ) ) ;
#28587 = LINE ( 'NONE', #8698, #2087 ) ;
#28588 = ADVANCED_FACE ( 'NONE', ( #14844 ), #34642, .F. ) ;
#28589 = ORIENTED_EDGE ( 'NONE', *, *, #4009, .F. ) ;
#28590 = CARTESIAN_POINT ( 'NONE',  ( -65.92798595308768483, 40.00000000000000711, 22.39357416381200849 ) ) ;
#28591 = CYLINDRICAL_SURFACE ( 'NONE', #19457, 139.5000000000000000 ) ;
#28592 = ORIENTED_EDGE ( 'NONE', *, *, #10275, .F. ) ;
#28593 = EDGE_CURVE ( 'NONE', #37390, #32317, #26371, .T. ) ;
#28594 = LINE ( 'NONE', #8289, #21809 ) ;
#28595 = DIRECTION ( 'NONE',  ( -1.000000000000000000, -0.000000000000000000, -0.000000000000000000 ) ) ;
#28596 = FACE_OUTER_BOUND ( 'NONE', #21905, .T. ) ;
#28597 = ORIENTED_EDGE ( 'NONE', *, *, #27484, .T. ) ;
#28598 = ORIENTED_EDGE ( 'NONE', *, *, #4376, .T. ) ;
#28599 = DIRECTION ( 'NONE',  ( -1.000000000000000000, -0.000000000000000000, 0.000000000000000000 ) ) ;
#28601 = VERTEX_POINT ( 'NONE', #2967 ) ;
#28600 = AXIS2_PLACEMENT_3D ( 'NONE', #12004, #38364, #38158 ) ;
#28602 = DIRECTION ( 'NONE',  ( -1.000000000000000000, -0.000000000000000000, -0.000000000000000000 ) ) ;
#28603 = CIRCLE ( 'NONE', #9044, 20.00000000000000711 ) ;
#28604 = DIRECTION ( 'NONE',  ( 1.000000000000000000, 0.000000000000000000, 0.000000000000000000 ) ) ;
#28605 = AXIS2_PLACEMENT_3D ( 'NONE', #19479, #22751, #15984 ) ;
#28606 = DIRECTION ( 'NONE',  ( 0.000000000000000000, 1.000000000000000000, -1.060184893785364939E-15 ) ) ;
#28607 = CYLINDRICAL_SURFACE ( 'NONE', #19926, 47.49900000000000233 ) ;
#28608 = ORIENTED_EDGE ( 'NONE', *, *, #23258, .T. ) ;
#28609 = CARTESIAN_POINT ( 'NONE',  ( 17.99999999999999645, 84.62908780824871258, 85.78116633471321961 ) ) ;
#28610 = DIRECTION ( 'NONE',  ( -1.000000000000000000, 0.000000000000000000, 0.000000000000000000 ) ) ;
#28611 = ORIENTED_EDGE ( 'NONE', *, *, #18780, .T. ) ;
#28612 = DIRECTION ( 'NONE',  ( 0.000000000000000000, 0.000000000000000000, 1.000000000000000000 ) ) ;
#28613 = CARTESIAN_POINT ( 'NONE',  ( 0.000000000000000000, 101.1403355683153933, -56.80345518653383152 ) ) ;
#28614 = DIRECTION ( 'NONE',  ( 4.329780281177459034E-17, 1.000000000000000000, -4.329780281177474441E-17 ) ) ;
#28615 = DIRECTION ( 'NONE',  ( 0.000000000000000000, 0.000000000000000000, 1.000000000000000000 ) ) ;
#28616 = CARTESIAN_POINT ( 'NONE',  ( -25.89845354150052259, 31.00000000000000355, -44.83417823681238445 ) ) ;
#28617 = VERTEX_POINT ( 'NONE', #5842 ) ;
#28619 = DIRECTION ( 'NONE',  ( 0.000000000000000000, 0.000000000000000000, 1.000000000000000000 ) ) ;
#28618 = DIRECTION ( 'NONE',  ( 0.000000000000000000, 0.2631025642275152676, 0.9647678688145175929 ) ) ;
#28620 = AXIS2_PLACEMENT_3D ( 'NONE', #2167, #8953, #1965 ) ;
#28621 = EDGE_LOOP ( 'NONE', ( #33990, #20584, #37726, #34472 ) ) ;
#28622 = CARTESIAN_POINT ( 'NONE',  ( 25.16436199730139123, 40.00000000000000000, 51.02488717759543135 ) ) ;
#28623 = AXIS2_PLACEMENT_3D ( 'NONE', #33948, #4035, #13685 ) ;
#28624 = EDGE_CURVE ( 'NONE', #30653, #6921, #22913, .T. ) ;
#28625 = AXIS2_PLACEMENT_3D ( 'NONE', #10381, #20238, #33499 ) ;
#28626 = CARTESIAN_POINT ( 'NONE',  ( -24.74979319748359785, -2.055254544495722868, 2.972870684497277427 ) ) ;
#28627 = CARTESIAN_POINT ( 'NONE',  ( 17.99999999999999645, 0.000000000000000000, 0.000000000000000000 ) ) ;
#28628 = AXIS2_PLACEMENT_3D ( 'NONE', #17505, #37734, #10937 ) ;
#28629 = FACE_OUTER_BOUND ( 'NONE', #32359, .T. ) ;
#28630 = CARTESIAN_POINT ( 'NONE',  ( 17.99999999999999645, -26.29521155129837595, -17.34211205339375184 ) ) ;
#28631 = EDGE_CURVE ( 'NONE', #38008, #40762, #31091, .T. ) ;
#28632 = ORIENTED_EDGE ( 'NONE', *, *, #31800, .T. ) ;
#28633 = CARTESIAN_POINT ( 'NONE',  ( -12.24460912605626106, 40.00000000000000000, 36.08157028455360660 ) ) ;
#28634 = ORIENTED_EDGE ( 'NONE', *, *, #7944, .T. ) ;
#28635 = LINE ( 'NONE', #42333, #8339 ) ;
#28636 = DIRECTION ( 'NONE',  ( -1.000000000000000000, -0.000000000000000000, -0.000000000000000000 ) ) ;
#28637 = ORIENTED_EDGE ( 'NONE', *, *, #29504, .F. ) ;
#28638 = EDGE_CURVE ( 'NONE', #8430, #3574, #22684, .T. ) ;
#28639 = CARTESIAN_POINT ( 'NONE',  ( 18.00000000000000355, -34.03046037009231384, -33.13733193845841640 ) ) ;
#28640 = EDGE_CURVE ( 'NONE', #37184, #170, #22474, .T. ) ;
#28641 = ORIENTED_EDGE ( 'NONE', *, *, #41534, .F. ) ;
#28642 = CARTESIAN_POINT ( 'NONE',  ( 17.99999999999999645, 0.000000000000000000, 0.000000000000000000 ) ) ;
#28643 = VERTEX_POINT ( 'NONE', #3413 ) ;
#28644 = EDGE_LOOP ( 'NONE', ( #9525, #42222 ) ) ;
#28645 = CARTESIAN_POINT ( 'NONE',  ( 17.99999999999999645, -92.25992191227442163, 77.51514567967366531 ) ) ;
#28647 = CIRCLE ( 'NONE', #17423, 116.0000000000000000 ) ;
#28646 = CARTESIAN_POINT ( 'NONE',  ( -60.98551593175036345, 31.00000000000000711, 53.34359504441579247 ) ) ;
#28648 = ORIENTED_EDGE ( 'NONE', *, *, #1490, .T. ) ;
#28649 = DIRECTION ( 'NONE',  ( 1.058513553088275437E-16, 1.000000000000000000, -8.813324511995299047E-17 ) ) ;
#28650 = AXIS2_PLACEMENT_3D ( 'NONE', #36500, #43058, #6622 ) ;
#28651 = DIRECTION ( 'NONE',  ( -1.000000000000000000, 0.000000000000000000, 0.000000000000000000 ) ) ;
#28652 = ORIENTED_EDGE ( 'NONE', *, *, #30164, .F. ) ;
#28653 = CARTESIAN_POINT ( 'NONE',  ( 8.999999999999998224, 112.8457601792515419, 26.86697618949414945 ) ) ;
#28654 = CARTESIAN_POINT ( 'NONE',  ( 26.80287614962791309, -12.05525454449572464, 69.29271901957253021 ) ) ;
#28656 = EDGE_CURVE ( 'NONE', #33767, #23951, #3891, .T. ) ;
#28655 = CIRCLE ( 'NONE', #34202, 31.49900000000000233 ) ;
#28657 = AXIS2_PLACEMENT_3D ( 'NONE', #21701, #1139, #5067 ) ;
#28658 = CARTESIAN_POINT ( 'NONE',  ( 24.91045342551303321, 31.00000000000000355, 12.31387362277163433 ) ) ;
#28659 = EDGE_CURVE ( 'NONE', #20160, #4825, #15781, .T. ) ;
#28661 = CARTESIAN_POINT ( 'NONE',  ( 17.99999999999999645, 0.000000000000000000, 0.000000000000000000 ) ) ;
#28660 = DIRECTION ( 'NONE',  ( 1.000000000000000000, 0.000000000000000000, 0.000000000000000000 ) ) ;
#28662 = MANIFOLD_SOLID_BREP ( 'RollersSimplified', #11473 ) ;
#28663 = AXIS2_PLACEMENT_3D ( 'NONE', #17442, #30285, #33544 ) ;
#28664 = DIRECTION ( 'NONE',  ( 0.000000000000000000, 0.5528000653611888637, 0.8333139190825180620 ) ) ;
#28665 = DIRECTION ( 'NONE',  ( 0.000000000000000000, 0.9826841245925214130, -0.1852887240871113894 ) ) ;
#28666 = ORIENTED_EDGE ( 'NONE', *, *, #12087, .T. ) ;
#28667 = CYLINDRICAL_SURFACE ( 'NONE', #30406, 2.500000000000000444 ) ;
#28668 = VECTOR ( 'NONE', #6943, 1000.000000000000000 ) ;
#28669 = EDGE_LOOP ( 'NONE', ( #30503, #30699, #18261, #32498 ) ) ;
#28670 = DIRECTION ( 'NONE',  ( 1.000000000000000000, 0.000000000000000000, 0.000000000000000000 ) ) ;
#28671 = CARTESIAN_POINT ( 'NONE',  ( 74.70319961851696178, 31.00000000000000000, -57.31929289364909152 ) ) ;
#28672 = DIRECTION ( 'NONE',  ( 0.000000000000000000, -0.3681245526846653737, -0.9297764858882564543 ) ) ;
#28673 = ORIENTED_EDGE ( 'NONE', *, *, #32377, .T. ) ;
#28674 = VECTOR ( 'NONE', #25829, 1000.000000000000000 ) ;
#28675 = CARTESIAN_POINT ( 'NONE',  ( -14.19360040536685830, 40.00000000000000000, 24.59234967646941783 ) ) ;
#28676 = EDGE_CURVE ( 'NONE', #17094, #17808, #33886, .T. ) ;
#28677 = CARTESIAN_POINT ( 'NONE',  ( -32.60815990948594134, 40.00000000000000000, 24.92795611697640368 ) ) ;
#28678 = ORIENTED_EDGE ( 'NONE', *, *, #2558, .T. ) ;
#28679 = VERTEX_POINT ( 'NONE', #16123 ) ;
#28680 = CYLINDRICAL_SURFACE ( 'NONE', #14375, 47.49900000000000233 ) ;
#28681 = CYLINDRICAL_SURFACE ( 'NONE', #5356, 13.59999999999999964 ) ;
#28682 = DIRECTION ( 'NONE',  ( 0.000000000000000000, 0.000000000000000000, 1.000000000000000000 ) ) ;
#28683 = CARTESIAN_POINT ( 'NONE',  ( -4.000000000000000000, -2.309401076758515803, -0.4999999999999995559 ) ) ;
#28684 = EDGE_CURVE ( 'NONE', #24642, #7094, #15116, .T. ) ;
#28685 = EDGE_CURVE ( 'NONE', #13380, #20648, #20689, .T. ) ;
#28686 = LINE ( 'NONE', #19947, #11180 ) ;
#28687 = ORIENTED_EDGE ( 'NONE', *, *, #19564, .F. ) ;
#28688 = DIRECTION ( 'NONE',  ( 1.000000000000000000, 0.000000000000000000, 0.000000000000000000 ) ) ;
#28689 = ORIENTED_EDGE ( 'NONE', *, *, #6964, .T. ) ;
#28690 = CARTESIAN_POINT ( 'NONE',  ( 2.500000000000000000, -2.357898499370432166, 3.035766082959412415E-15 ) ) ;
#28691 = AXIS2_PLACEMENT_3D ( 'NONE', #6351, #22131, #2204 ) ;
#28692 = DIRECTION ( 'NONE',  ( -1.000000000000000000, -0.000000000000000000, -0.000000000000000000 ) ) ;
#28693 = AXIS2_PLACEMENT_3D ( 'NONE', #32747, #15358, #39268 ) ;
#28694 = EDGE_CURVE ( 'NONE', #30637, #27094, #23755, .T. ) ;
#28695 = DIRECTION ( 'NONE',  ( 0.000000000000000000, 2.305124076552231752E-14, -1.000000000000000000 ) ) ;
#28696 = CIRCLE ( 'NONE', #16838, 120.5010000000000190 ) ;
#28697 = DIRECTION ( 'NONE',  ( -1.000000000000000000, 0.000000000000000000, 0.000000000000000000 ) ) ;
#28698 = ADVANCED_FACE ( 'NONE', ( #14145 ), #10417, .T. ) ;
#28699 = ORIENTED_EDGE ( 'NONE', *, *, #650, .F. ) ;
#28700 = ORIENTED_EDGE ( 'NONE', *, *, #15582, .F. ) ;
#28701 = DIRECTION ( 'NONE',  ( 0.000000000000000000, -1.224646799147359124E-16, 1.000000000000000000 ) ) ;
#28702 = CIRCLE ( 'NONE', #29405, 52.00000000000000000 ) ;
#28703 = VERTEX_POINT ( 'NONE', #33537 ) ;
#28705 = ORIENTED_EDGE ( 'NONE', *, *, #28210, .F. ) ;
#28704 = DIRECTION ( 'NONE',  ( -1.000000000000000000, 0.000000000000000000, 0.000000000000000000 ) ) ;
#28706 = CARTESIAN_POINT ( 'NONE',  ( 43.74200748489511881, 31.00000000000000355, 38.49442098324159645 ) ) ;
#28707 = VERTEX_POINT ( 'NONE', #20485 ) ;
#28708 = DIRECTION ( 'NONE',  ( 1.000000000000000000, 0.000000000000000000, 0.000000000000000000 ) ) ;
#28709 = DIRECTION ( 'NONE',  ( 0.000000000000000000, 0.9996456111234526265, -0.02662052143777152158 ) ) ;
#28710 = ORIENTED_EDGE ( 'NONE', *, *, #40596, .F. ) ;
#28711 = CARTESIAN_POINT ( 'NONE',  ( 74.15939217265263039, 39.99999999999999289, -19.75058139460558237 ) ) ;
#28712 = EDGE_CURVE ( 'NONE', #38951, #27883, #40871, .T. ) ;
#28713 = EDGE_CURVE ( 'NONE', #24613, #15816, #27225, .T. ) ;
#28714 = CARTESIAN_POINT ( 'NONE',  ( 0.000000000000000000, 17.77780072541695944, 114.6296200873376563 ) ) ;
#28715 = EDGE_CURVE ( 'NONE', #20659, #6259, #23967, .T. ) ;
#28716 = EDGE_CURVE ( 'NONE', #35102, #31882, #33973, .T. ) ;
#28717 = CARTESIAN_POINT ( 'NONE',  ( 17.99999999999999645, -80.74349901498355564, -77.90224541347362219 ) ) ;
#28718 = VERTEX_POINT ( 'NONE', #20274 ) ;
#28719 = DIRECTION ( 'NONE',  ( 0.000000000000000000, 0.000000000000000000, 1.000000000000000000 ) ) ;
#28720 = EDGE_LOOP ( 'NONE', ( #1714, #3174, #16839, #13281 ) ) ;
#28721 =( NAMED_UNIT ( * ) PLANE_ANGLE_UNIT ( ) SI_UNIT ( $, .RADIAN. ) );
#28722 = VECTOR ( 'NONE', #7045, 1000.000000000000000 ) ;
#28723 =( REPRESENTATION_RELATIONSHIP ('NONE','NONE', #330, #15194 ) REPRESENTATION_RELATIONSHIP_WITH_TRANSFORMATION ( #22512 )SHAPE_REPRESENTATION_RELATIONSHIP( ) );
#28724 = CARTESIAN_POINT ( 'NONE',  ( 17.99999999999999645, 0.000000000000000000, 0.000000000000000000 ) ) ;
#28725 = CARTESIAN_POINT ( 'NONE',  ( 0.000000000000000000, 11.65176648921033298, 115.4133282497342918 ) ) ;
#28726 = CIRCLE ( 'NONE', #38430, 12.59999999999999964 ) ;
#28727 = CARTESIAN_POINT ( 'NONE',  ( 31.73387399974884104, 31.00000000000000355, -54.96645564127986461 ) ) ;
#28728 = DIRECTION ( 'NONE',  ( 0.000000000000000000, 0.000000000000000000, -1.000000000000000000 ) ) ;
#28729 = EDGE_LOOP ( 'NONE', ( #40425, #42932, #10258, #34251 ) ) ;
#28730 = VECTOR ( 'NONE', #39906, 1000.000000000000000 ) ;
#28731 = ORIENTED_EDGE ( 'NONE', *, *, #23161, .F. ) ;
#28732 = CARTESIAN_POINT ( 'NONE',  ( 0.000000000000000000, 17.77780072541854040, -114.6296200873374147 ) ) ;
#28733 = FACE_OUTER_BOUND ( 'NONE', #29456, .T. ) ;
#28734 = CARTESIAN_POINT ( 'NONE',  ( 5.735608225908778834, 31.00000000000000355, 89.40012361740336644 ) ) ;
#28735 = CARTESIAN_POINT ( 'NONE',  ( -68.52217190868857699, 40.00000000000000711, 59.94826526062049510 ) ) ;
#28736 = CYLINDRICAL_SURFACE ( 'NONE', #3446, 47.49900000000000233 ) ;
#28737 = EDGE_CURVE ( 'NONE', #16328, #11213, #17435, .T. ) ;
#28738 = ORIENTED_EDGE ( 'NONE', *, *, #23676, .T. ) ;
#28739 = CARTESIAN_POINT ( 'NONE',  ( 4.000000000000000000, 2.309401076758515803, -0.4999999999999995559 ) ) ;
#28740 = EDGE_LOOP ( 'NONE', ( #27104, #11783, #28988, #15412 ) ) ;
#28741 = DIRECTION ( 'NONE',  ( -1.000000000000000000, -0.000000000000000000, -0.000000000000000000 ) ) ;
#28742 = EDGE_CURVE ( 'NONE', #5471, #39523, #10951, .T. ) ;
#28744 = ORIENTED_EDGE ( 'NONE', *, *, #16655, .T. ) ;
#28743 = FACE_OUTER_BOUND ( 'NONE', #2129, .T. ) ;
#28745 = CARTESIAN_POINT ( 'NONE',  ( 0.000000000000000000, -46.19362259308827845, -8.585149169758995669 ) ) ;
#28746 = ORIENTED_EDGE ( 'NONE', *, *, #19883, .T. ) ;
#28747 = CARTESIAN_POINT ( 'NONE',  ( 17.99999999999999645, 0.000000000000000000, 0.000000000000000000 ) ) ;
#28748 = CARTESIAN_POINT ( 'NONE',  ( 25.26056536696837185, 115.2644951289906885, 0.000000000000000000 ) ) ;
#28749 = AXIS2_PLACEMENT_3D ( 'NONE', #35343, #27967, #11161 ) ;
#28750 = FACE_OUTER_BOUND ( 'NONE', #27061, .T. ) ;
#28751 = AXIS2_PLACEMENT_3D ( 'NONE', #2162, #25561, #5236 ) ;
#28752 = VECTOR ( 'NONE', #20673, 1000.000000000000000 ) ;
#28753 = ORIENTED_EDGE ( 'NONE', *, *, #22784, .F. ) ;
#28754 = CARTESIAN_POINT ( 'NONE',  ( 26.10672890669568602, 31.00000000000000355, 8.893381768403882504 ) ) ;
#28755 = DIRECTION ( 'NONE',  ( 1.000000000000000000, 0.000000000000000000, 0.000000000000000000 ) ) ;
#28757 = CYLINDRICAL_SURFACE ( 'NONE', #33833, 139.4999999999992610 ) ;
#28756 = FACE_OUTER_BOUND ( 'NONE', #9940, .T. ) ;
#28758 = ORIENTED_EDGE ( 'NONE', *, *, #24530, .F. ) ;
#28759 = DIRECTION ( 'NONE',  ( 0.000000000000000000, 1.541976423090494253E-15, 1.000000000000000000 ) ) ;
#28760 = DIRECTION ( 'NONE',  ( -1.000000000000000000, -0.000000000000000000, -0.000000000000000000 ) ) ;
#28762 = CARTESIAN_POINT ( 'NONE',  ( -37.12595630543398073, 40.00000000000000000, 18.22532657727797911 ) ) ;
#28761 = AXIS2_PLACEMENT_3D ( 'NONE', #25352, #19448, #32713 ) ;
#28763 = DIRECTION ( 'NONE',  ( -1.000000000000000000, 0.000000000000000000, 0.000000000000000000 ) ) ;
#28764 = ADVANCED_FACE ( 'NONE', ( #1234 ), #579, .F. ) ;
#28765 = ADVANCED_FACE ( 'NONE', ( #34183 ), #7784, .F. ) ;
#28766 = LINE ( 'NONE', #42028, #27753 ) ;
#28767 = EDGE_CURVE ( 'NONE', #13442, #32233, #15148, .T. ) ;
#28768 = EDGE_CURVE ( 'NONE', #31266, #1103, #40286, .T. ) ;
#28769 = CYLINDRICAL_SURFACE ( 'NONE', #41562, 116.0000000000000000 ) ;
#28770 = VERTEX_POINT ( 'NONE', #36807 ) ;
#28771 = DIRECTION ( 'NONE',  ( 0.000000000000000000, -0.000000000000000000, 1.000000000000000000 ) ) ;
#28772 = EDGE_CURVE ( 'NONE', #12547, #41527, #20723, .T. ) ;
#28773 = VERTEX_POINT ( 'NONE', #787 ) ;
#28774 = DIRECTION ( 'NONE',  ( -1.000000000000000000, 0.000000000000000000, 0.000000000000000000 ) ) ;
#28775 = DIRECTION ( 'NONE',  ( 1.000000000000000000, -0.000000000000000000, -0.000000000000000000 ) ) ;
#28776 = CARTESIAN_POINT ( 'NONE',  ( -16.93500259178182432, 31.00000000000000355, 34.36424406943201149 ) ) ;
#28777 = ORIENTED_EDGE ( 'NONE', *, *, #26850, .F. ) ;
#28778 = CARTESIAN_POINT ( 'NONE',  ( 0.000000000000000000, 0.000000000000000000, 0.000000000000000000 ) ) ;
#28779 = VERTEX_POINT ( 'NONE', #33746 ) ;
#28780 = EDGE_CURVE ( 'NONE', #39186, #31919, #14409, .T. ) ;
#28781 = CARTESIAN_POINT ( 'NONE',  ( 8.999999999999998224, -94.52951811191606168, 67.23221107124869889 ) ) ;
#28782 = AXIS2_PLACEMENT_3D ( 'NONE', #4037, #30051, #33517 ) ;
#28783 = CARTESIAN_POINT ( 'NONE',  ( -84.90650804512098659, 31.00000000000000711, 28.83788733109305014 ) ) ;
#28784 = ORIENTED_EDGE ( 'NONE', *, *, #36479, .T. ) ;
#28785 = CARTESIAN_POINT ( 'NONE',  ( -30.89738163651153258, 31.00000000000000355, 40.13100860029957317 ) ) ;
#28786 = CIRCLE ( 'NONE', #21838, 120.5010000000000190 ) ;
#28787 = CARTESIAN_POINT ( 'NONE',  ( -72.39171112334068425, 40.00000000000000711, -55.52881859171880308 ) ) ;
#28788 = ORIENTED_EDGE ( 'NONE', *, *, #6810, .F. ) ;
#28789 = CIRCLE ( 'NONE', #17662, 4.250000000000000000 ) ;
#28790 = PLANE ( 'NONE',  #41535 ) ;
#28791 = DIRECTION ( 'NONE',  ( -1.000000000000000000, -0.000000000000000000, -0.000000000000000000 ) ) ;
#28792 = CARTESIAN_POINT ( 'NONE',  ( 0.000000000000000000, 0.000000000000000000, 0.000000000000000000 ) ) ;
#28794 = ORIENTED_EDGE ( 'NONE', *, *, #2403, .T. ) ;
#28793 = CARTESIAN_POINT ( 'NONE',  ( 17.99999999999999645, -16.77566611177856615, 119.3275660838941832 ) ) ;
#28795 = DIRECTION ( 'NONE',  ( 0.000000000000000000, 0.000000000000000000, 1.000000000000000000 ) ) ;
#28796 = LINE ( 'NONE', #9774, #11943 ) ;
#28797 = EDGE_LOOP ( 'NONE', ( #4951, #29569, #29969, #42805 ) ) ;
#28798 = CARTESIAN_POINT ( 'NONE',  ( -52.79687664379660816, 40.00000000000000000, -30.48099731442381710 ) ) ;
#28799 = DIRECTION ( 'NONE',  ( 1.000000000000000000, 0.000000000000000000, 0.000000000000000000 ) ) ;
#28800 = ORIENTED_EDGE ( 'NONE', *, *, #9863, .T. ) ;
#28801 = CARTESIAN_POINT ( 'NONE',  ( 8.999999999999998224, -59.47573314508669284, -99.59235496188668435 ) ) ;
#28802 = MANIFOLD_SOLID_BREP ( 'TeethCuts', #37943 ) ;
#28803 = EDGE_LOOP ( 'NONE', ( #38536, #31228, #39491 ) ) ;
#28804 = CIRCLE ( 'NONE', #18403, 120.5010000000000190 ) ;
#28805 = VERTEX_POINT ( 'NONE', #34613 ) ;
#28806 = CARTESIAN_POINT ( 'NONE',  ( 17.99999999999999645, -88.00363688980490906, -82.31555682352745862 ) ) ;
#28807 = ORIENTED_EDGE ( 'NONE', *, *, #24944, .F. ) ;
#28808 = DIRECTION ( 'NONE',  ( 0.000000000000000000, 0.000000000000000000, 1.000000000000000000 ) ) ;
#28809 = DIRECTION ( 'NONE',  ( 1.000000000000000000, 0.000000000000000000, -0.000000000000000000 ) ) ;
#28810 = DIRECTION ( 'NONE',  ( -1.000000000000000000, 0.000000000000000000, 0.000000000000000000 ) ) ;
#28811 = EDGE_CURVE ( 'NONE', #5335, #26178, #40497, .T. ) ;
#28812 = EDGE_CURVE ( 'NONE', #36747, #41807, #38518, .T. ) ;
#28813 = FACE_OUTER_BOUND ( 'NONE', #4284, .T. ) ;
#28814 = ORIENTED_EDGE ( 'NONE', *, *, #751, .T. ) ;
#28815 = CYLINDRICAL_SURFACE ( 'NONE', #36286, 129.9999999999993463 ) ;
#28816 = EDGE_CURVE ( 'NONE', #9979, #39267, #14444, .T. ) ;
#28817 = ORIENTED_EDGE ( 'NONE', *, *, #32254, .T. ) ;
#28818 = CIRCLE ( 'NONE', #18413, 59.00000000000001421 ) ;
#28819 = CARTESIAN_POINT ( 'NONE',  ( 18.00000000000000355, -49.65209126885751800, -15.44894276735603178 ) ) ;
#28820 = EDGE_LOOP ( 'NONE', ( #21687, #8120, #12061, #19985 ) ) ;
#28821 = CARTESIAN_POINT ( 'NONE',  ( 17.99999999999999645, 0.000000000000000000, 0.000000000000000000 ) ) ;
#28822 = DIRECTION ( 'NONE',  ( 0.000000000000000000, 0.000000000000000000, 1.000000000000000000 ) ) ;
#28823 = EDGE_CURVE ( 'NONE', #6504, #10645, #9533, .T. ) ;
#28824 = CARTESIAN_POINT ( 'NONE',  ( -106.4195705685748550, 17.99999999999998934, 106.4195705685759776 ) ) ;
#28825 = CARTESIAN_POINT ( 'NONE',  ( 17.99999999999999645, 0.000000000000000000, 0.000000000000000000 ) ) ;
#28826 = CARTESIAN_POINT ( 'NONE',  ( 39.77940265867437120, 31.00000000000000355, 22.96373720238702276 ) ) ;
#28827 = VERTEX_POINT ( 'NONE', #2284 ) ;
#28828 = DIRECTION ( 'NONE',  ( -1.000000000000000000, 0.000000000000000000, 0.000000000000000000 ) ) ;
#28829 = ADVANCED_FACE ( 'NONE', ( #24848 ), #4946, .T. ) ;
#28830 = ORIENTED_EDGE ( 'NONE', *, *, #21888, .T. ) ;
#28831 = CIRCLE ( 'NONE', #7209, 51.99999999999999289 ) ;
#28832 = CARTESIAN_POINT ( 'NONE',  ( 7.506055610550203205, 40.00000000000000000, 56.92102948000351148 ) ) ;
#28833 = AXIS2_PLACEMENT_3D ( 'NONE', #42101, #32728, #3015 ) ;
#28834 = CYLINDRICAL_SURFACE ( 'NONE', #3235, 120.5010000000000190 ) ;
#28835 = DIRECTION ( 'NONE',  ( -1.000000000000000000, -0.000000000000000000, -0.000000000000000000 ) ) ;
#28836 = CARTESIAN_POINT ( 'NONE',  ( 18.00000000000000355, 45.78515115856043138, 12.64416602183680993 ) ) ;
#28837 = DIRECTION ( 'NONE',  ( -1.000000000000000000, -0.000000000000000000, -0.000000000000000000 ) ) ;
#28838 = COLOUR_RGB ( '', 0.40784314, 0.44705882, 0.49803922) ;
#28839 = ORIENTED_EDGE ( 'NONE', *, *, #18791, .T. ) ;
#28840 = CARTESIAN_POINT ( 'NONE',  ( 22.22924588317381023, 40.00000000000000000, -25.35314793696836588 ) ) ;
#28841 = VERTEX_POINT ( 'NONE', #41586 ) ;
#28842 = CARTESIAN_POINT ( 'NONE',  ( 17.99999999999999645, 16.77727049691149475, -27.19001440037526862 ) ) ;
#28843 = CIRCLE ( 'NONE', #40662, 116.0000000000000000 ) ;
#28844 = DIRECTION ( 'NONE',  ( -1.000000000000000000, -0.000000000000000000, -0.000000000000000000 ) ) ;
#28845 = VERTEX_POINT ( 'NONE', #8228 ) ;
#28846 = CARTESIAN_POINT ( 'NONE',  ( 17.99999999999999645, 111.2721026680460596, -14.38025178762657852 ) ) ;
#28847 = ORIENTED_EDGE ( 'NONE', *, *, #22749, .T. ) ;
#28848 = CARTESIAN_POINT ( 'NONE',  ( 0.000000000000000000, -15.21076497709793252, 119.5371223922154797 ) ) ;
#28849 = VERTEX_POINT ( 'NONE', #12157 ) ;
#28850 = CIRCLE ( 'NONE', #37165, 120.5010000000000190 ) ;
#28851 = ORIENTED_EDGE ( 'NONE', *, *, #32284, .F. ) ;
#28852 = CYLINDRICAL_SURFACE ( 'NONE', #18170, 51.99999999999999289 ) ;
#28853 = CARTESIAN_POINT ( 'NONE',  ( -5.321195512787073589, 31.00000000000000355, 79.59297073838583003 ) ) ;
#28854 = ORIENTED_EDGE ( 'NONE', *, *, #24742, .F. ) ;
#28855 = DIRECTION ( 'NONE',  ( -1.000000000000000000, 0.000000000000000000, 0.000000000000000000 ) ) ;
#28856 = VECTOR ( 'NONE', #14884, 1000.000000000000000 ) ;
#28857 = EDGE_CURVE ( 'NONE', #1613, #13871, #32511, .T. ) ;
#28858 = FACE_OUTER_BOUND ( 'NONE', #37914, .T. ) ;
#28859 = ORIENTED_EDGE ( 'NONE', *, *, #4256, .F. ) ;
#28860 = CARTESIAN_POINT ( 'NONE',  ( -10.00000000000000000, 0.000000000000000000, 0.000000000000000000 ) ) ;
#28861 = AXIS2_PLACEMENT_3D ( 'NONE', #33107, #3194, #7135 ) ;
#28862 = DIRECTION ( 'NONE',  ( 0.000000000000000000, 0.7705132427757861446, 0.6374239897486935202 ) ) ;
#28863 = CARTESIAN_POINT ( 'NONE',  ( -17.43724119492662794, 31.00000000000000355, -15.29674861594511448 ) ) ;
#28865 = DIRECTION ( 'NONE',  ( 1.000000000000000000, 0.000000000000000000, 0.000000000000000000 ) ) ;
#28864 = CARTESIAN_POINT ( 'NONE',  ( 9.000000000000001776, -23.85344185397118011, -113.5209818126993611 ) ) ;
#28866 = ADVANCED_FACE ( 'NONE', ( #32205 ), #8865, .T. ) ;
#28867 = CARTESIAN_POINT ( 'NONE',  ( -2.924622967158192921, 31.00000000000000355, -22.14664255385889291 ) ) ;
#28868 = CARTESIAN_POINT ( 'NONE',  ( 17.99999999999999645, -105.3681574666261298, -38.54638589714993202 ) ) ;
#28869 = ORIENTED_EDGE ( 'NONE', *, *, #1603, .T. ) ;
#28870 = ADVANCED_FACE ( 'NONE', ( #32000 ), #25073, .T. ) ;
#28871 =( NAMED_UNIT ( * ) SI_UNIT ( $, .STERADIAN. ) SOLID_ANGLE_UNIT ( ) );
#28872 = PRESENTATION_STYLE_ASSIGNMENT (( #2216 ) ) ;
#28873 = AXIS2_PLACEMENT_3D ( 'NONE', #6932, #30728, #30935 ) ;
#28874 = VERTEX_POINT ( 'NONE', #7996 ) ;
#28875 = CARTESIAN_POINT ( 'NONE',  ( 17.99999999999999645, 0.000000000000000000, 0.000000000000000000 ) ) ;
#28876 = EDGE_CURVE ( 'NONE', #6899, #5227, #38761, .T. ) ;
#28877 = DIRECTION ( 'NONE',  ( 0.000000000000000000, 0.000000000000000000, 1.000000000000000000 ) ) ;
#28878 = ORIENTED_EDGE ( 'NONE', *, *, #3936, .F. ) ;
#28879 = CARTESIAN_POINT ( 'NONE',  ( 3.579113344806025054, 40.00000000000000000, 27.11441211503905535 ) ) ;
#28880 = CIRCLE ( 'NONE', #34430, 20.00000000000000355 ) ;
#28881 = CARTESIAN_POINT ( 'NONE',  ( 21.72498709343026846, 40.00000000000000000, -28.22316639787646864 ) ) ;
#28882 = CIRCLE ( 'NONE', #16362, 120.5010000000000332 ) ;
#28883 = ORIENTED_EDGE ( 'NONE', *, *, #39383, .T. ) ;
#28884 = CIRCLE ( 'NONE', #10043, 120.5010000000000332 ) ;
#28885 = ORIENTED_EDGE ( 'NONE', *, *, #39091, .F. ) ;
#28886 = DIRECTION ( 'NONE',  ( -1.000000000000000000, -0.000000000000000000, -0.000000000000000000 ) ) ;
#28887 = DIRECTION ( 'NONE',  ( 0.000000000000000000, 0.000000000000000000, 1.000000000000000000 ) ) ;
#28888 = DIRECTION ( 'NONE',  ( -1.000000000000000000, -0.000000000000000000, -0.000000000000000000 ) ) ;
#28889 = AXIS2_PLACEMENT_3D ( 'NONE', #9549, #19405, #23107 ) ;
#28890 = CYLINDRICAL_SURFACE ( 'NONE', #4496, 120.5010000000000190 ) ;
#28891 = EDGE_CURVE ( 'NONE', #3075, #35838, #26267, .T. ) ;
#28892 = LINE ( 'NONE', #32576, #42475 ) ;
#28893 = CIRCLE ( 'NONE', #32358, 59.00000000000000000 ) ;
#28894 = ORIENTED_EDGE ( 'NONE', *, *, #13539, .T. ) ;
#28895 = CARTESIAN_POINT ( 'NONE',  ( 0.000000000000000000, 0.000000000000000000, 0.000000000000000000 ) ) ;
#28896 = VERTEX_POINT ( 'NONE', #38740 ) ;
#28897 = DIRECTION ( 'NONE',  ( 1.000000000000000000, 0.000000000000000000, -3.273063162220425331E-16 ) ) ;
#28898 = EDGE_CURVE ( 'NONE', #9338, #8713, #7437, .T. ) ;
#28899 = CARTESIAN_POINT ( 'NONE',  ( 17.99999999999999645, 19.69434969228107946, -24.58291258574028504 ) ) ;
#28900 = EDGE_CURVE ( 'NONE', #4294, #5519, #31566, .T. ) ;
#28901 = CARTESIAN_POINT ( 'NONE',  ( 0.000000000000000000, -103.1672962317648512, -44.09967643725973119 ) ) ;
#28902 = CYLINDRICAL_SURFACE ( 'NONE', #31755, 20.00000000000000711 ) ;
#28903 = VERTEX_POINT ( 'NONE', #8433 ) ;
#28904 = ORIENTED_EDGE ( 'NONE', *, *, #6996, .F. ) ;
#28905 = CARTESIAN_POINT ( 'NONE',  ( -147.8500000000000227, -5.254679414958916394E-13, 6.999999999999998224 ) ) ;
#28906 = DIRECTION ( 'NONE',  ( 0.000000000000000000, 0.000000000000000000, 1.000000000000000000 ) ) ;
#28907 = EDGE_LOOP ( 'NONE', ( #23553, #22015, #36964, #18352 ) ) ;
#28909 = VERTEX_POINT ( 'NONE', #11950 ) ;
#28908 = LINE ( 'NONE', #42172, #34118 ) ;
#28910 = CARTESIAN_POINT ( 'NONE',  ( 24.55685208794459129, 31.00000000000000355, -49.59815698162134368 ) ) ;
#28911 = ORIENTED_EDGE ( 'NONE', *, *, #22970, .T. ) ;
#28912 = DIRECTION ( 'NONE',  ( 0.000000000000000000, -0.8993121301712231341, 0.4373073204588475704 ) ) ;
#28913 = CIRCLE ( 'NONE', #30987, 20.00000000000000711 ) ;
#28914 = EDGE_CURVE ( 'NONE', #1568, #34811, #8133, .T. ) ;
#28915 = FACE_BOUND ( 'NONE', #40657, .T. ) ;
#28916 = ORIENTED_EDGE ( 'NONE', *, *, #3912, .F. ) ;
#28917 = CARTESIAN_POINT ( 'NONE',  ( -9.616483412535155040, 40.00000000000000000, -73.82325415887568454 ) ) ;
#28918 = VECTOR ( 'NONE', #38899, 1000.000000000000000 ) ;
#28920 = CARTESIAN_POINT ( 'NONE',  ( 42.80287614962790599, -12.05525454449571932, 69.29271901957253021 ) ) ;
#28919 = CARTESIAN_POINT ( 'NONE',  ( 17.99999999999999645, 103.1672962317657323, -44.09967643725766351 ) ) ;
#28921 = CIRCLE ( 'NONE', #11510, 59.00000000000000711 ) ;
#28922 = DIRECTION ( 'NONE',  ( 1.000000000000000000, 0.000000000000000000, 0.000000000000000000 ) ) ;
#28923 = VERTEX_POINT ( 'NONE', #29378 ) ;
#28924 = DIRECTION ( 'NONE',  ( 1.000000000000000000, -3.035766082959412415E-17, 0.000000000000000000 ) ) ;
#28925 = VERTEX_POINT ( 'NONE', #36110 ) ;
#28926 = EDGE_CURVE ( 'NONE', #36617, #41769, #18655, .T. ) ;
#28927 = CIRCLE ( 'NONE', #10080, 2.499999999999999556 ) ;
#28928 = DIRECTION ( 'NONE',  ( 0.000000000000000000, 0.000000000000000000, 1.000000000000000000 ) ) ;
#28929 = PLANE ( 'NONE',  #42893 ) ;
#28930 = CARTESIAN_POINT ( 'NONE',  ( 38.75409931461306456, 31.00000000000000355, -50.52625141960567134 ) ) ;
#28932 = DIRECTION ( 'NONE',  ( 1.000000000000000000, -0.000000000000000000, -0.000000000000000000 ) ) ;
#28931 = CARTESIAN_POINT ( 'NONE',  ( 17.99999999999999645, 22.66088087769211157, -21.87856208362532939 ) ) ;
#28933 = VERTEX_POINT ( 'NONE', #29812 ) ;
#28934 = EDGE_CURVE ( 'NONE', #6975, #41781, #40150, .T. ) ;
#28935 = VECTOR ( 'NONE', #5307, 1000.000000000000000 ) ;
#28936 = DIRECTION ( 'NONE',  ( 0.000000000000000000, 0.000000000000000000, 1.000000000000000000 ) ) ;
#28937 = EDGE_LOOP ( 'NONE', ( #5179, #1439, #7345, #18715 ) ) ;
#28938 = DIRECTION ( 'NONE',  ( -1.000000000000000000, -0.000000000000000000, -0.000000000000000000 ) ) ;
#28939 = CARTESIAN_POINT ( 'NONE',  ( 17.99999999999999645, 59.47573314508733944, 99.59235496188628645 ) ) ;
#28940 = CARTESIAN_POINT ( 'NONE',  ( 42.30527206516848082, 31.00000000000000355, -85.53883208674149330 ) ) ;
#28941 = CARTESIAN_POINT ( 'NONE',  ( 76.36627019849126441, 39.99999999999999289, -58.43797548694632127 ) ) ;
#28942 = STYLED_ITEM ( 'NONE', ( #18273 ), #112 ) ;
#28943 = DIRECTION ( 'NONE',  ( 1.000000000000000000, 0.000000000000000000, 0.000000000000000000 ) ) ;
#28944 = CIRCLE ( 'NONE', #28272, 59.00000000000002132 ) ;
#28945 = ORIENTED_EDGE ( 'NONE', *, *, #30231, .F. ) ;
#28946 = DIRECTION ( 'NONE',  ( -1.000000000000000000, -0.000000000000000000, 0.000000000000000000 ) ) ;
#28947 = ORIENTED_EDGE ( 'NONE', *, *, #42657, .F. ) ;
#28948 = EDGE_CURVE ( 'NONE', #14958, #37380, #21421, .T. ) ;
#28949 = DIRECTION ( 'NONE',  ( -1.000000000000000000, 0.000000000000000000, -0.000000000000000000 ) ) ;
#28950 = VECTOR ( 'NONE', #16125, 999.9999999999998863 ) ;
#28951 = EDGE_CURVE ( 'NONE', #27015, #4469, #39367, .T. ) ;
#28952 = AXIS2_PLACEMENT_3D ( 'NONE', #23902, #19771, #33035 ) ;
#28954 = ORIENTED_EDGE ( 'NONE', *, *, #4324, .T. ) ;
#28953 = CARTESIAN_POINT ( 'NONE',  ( -6.999999999999992006, 18.77999999999999758, 0.000000000000000000 ) ) ;
#28955 = CARTESIAN_POINT ( 'NONE',  ( 0.000000000000000000, 2.007101075700416182, -31.43498920425967569 ) ) ;
#28956 = VERTEX_POINT ( 'NONE', #42437 ) ;
#28957 = CARTESIAN_POINT ( 'NONE',  ( 0.000000000000000000, 0.000000000000000000, 9.999999999999998224 ) ) ;
#28958 = CARTESIAN_POINT ( 'NONE',  ( 17.99999999999999645, -91.65951123222436081, -71.09524597798180423 ) ) ;
#28959 = CIRCLE ( 'NONE', #1770, 59.00000000000000000 ) ;
#28960 = DIRECTION ( 'NONE',  ( 1.000000000000000000, 0.000000000000000000, 0.000000000000000000 ) ) ;
#28961 = VERTEX_POINT ( 'NONE', #43082 ) ;
#28962 = CARTESIAN_POINT ( 'NONE',  ( -6.473970235329672780E-16, -4.862606272033106691, -3.745885042887442395 ) ) ;
#28963 = CARTESIAN_POINT ( 'NONE',  ( 0.000000000000000000, 24.22031524825977300, 109.5520369638038289 ) ) ;
#28964 = EDGE_CURVE ( 'NONE', #18580, #15011, #5362, .T. ) ;
#28966 = VERTEX_POINT ( 'NONE', #13231 ) ;
#28965 = CARTESIAN_POINT ( 'NONE',  ( 18.00000000000000355, 25.61928775981044026, 45.25098998563485964 ) ) ;
#28967 = EDGE_LOOP ( 'NONE', ( #27167, #37218 ) ) ;
#28968 = DIRECTION ( 'NONE',  ( -1.000000000000000000, -0.000000000000000000, -0.000000000000000000 ) ) ;
#28969 = DIRECTION ( 'NONE',  ( 0.000000000000000000, 0.000000000000000000, -1.000000000000000000 ) ) ;
#28970 = CARTESIAN_POINT ( 'NONE',  ( -40.27082278478597033, 40.00000000000000000, 10.71261860272680977 ) ) ;
#28971 = DIRECTION ( 'NONE',  ( -1.000000000000000000, 0.000000000000000000, 0.000000000000000000 ) ) ;
#28972 = AXIS2_PLACEMENT_3D ( 'NONE', #37205, #30475, #4033 ) ;
#28973 = CYLINDRICAL_SURFACE ( 'NONE', #7506, 120.5010000000000190 ) ;
#28974 = VECTOR ( 'NONE', #2171, 1000.000000000000000 ) ;
#28975 = DIRECTION ( 'NONE',  ( -1.000000000000000000, 0.000000000000000000, -0.000000000000000000 ) ) ;
#28977 = EDGE_LOOP ( 'NONE', ( #18308, #24317, #32829, #5039 ) ) ;
#28976 = AXIS2_PLACEMENT_3D ( 'NONE', #3272, #26439, #29938 ) ;
#28978 = CARTESIAN_POINT ( 'NONE',  ( -1.144235203016679359, -3.958177651039096911, -0.09382832055446428676 ) ) ;
#28979 = AXIS2_PLACEMENT_3D ( 'NONE', #4831, #18188, #14891 ) ;
#28980 = VERTEX_POINT ( 'NONE', #26523 ) ;
#28981 = EDGE_CURVE ( 'NONE', #25259, #39678, #29584, .T. ) ;
#28982 = AXIS2_PLACEMENT_3D ( 'NONE', #41143, #8229, #25074 ) ;
#28983 = LINE ( 'NONE', #12406, #27364 ) ;
#28984 = LINE ( 'NONE', #15280, #10817 ) ;
#28985 = AXIS2_PLACEMENT_3D ( 'NONE', #7320, #4260, #7762 ) ;
#28986 = EDGE_CURVE ( 'NONE', #24696, #40959, #24904, .T. ) ;
#28987 = CARTESIAN_POINT ( 'NONE',  ( -40.10416666498607441, 31.00000000000000355, -2.617993869485698344 ) ) ;
#28988 = ORIENTED_EDGE ( 'NONE', *, *, #15390, .T. ) ;
#28989 = DIRECTION ( 'NONE',  ( -1.000000000000000000, 0.000000000000000000, 0.000000000000000000 ) ) ;
#28991 = EDGE_LOOP ( 'NONE', ( #21860, #14963, #19558, #31489 ) ) ;
#28990 = AXIS2_PLACEMENT_3D ( 'NONE', #10465, #3665, #8046 ) ;
#28993 = AXIS2_PLACEMENT_3D ( 'NONE', #16343, #26383, #42700 ) ;
#28992 = CARTESIAN_POINT ( 'NONE',  ( -10.00000000000000000, 0.000000000000000000, 0.000000000000000000 ) ) ;
#28994 = CARTESIAN_POINT ( 'NONE',  ( 70.70367055548476287, 31.00000000000000000, -62.02616482874480397 ) ) ;
#28995 = CARTESIAN_POINT ( 'NONE',  ( 0.000000000000000000, -112.1427988504408120, 3.502162136923045566 ) ) ;
#28996 = ORIENTED_EDGE ( 'NONE', *, *, #43033, .F. ) ;
#28997 = CARTESIAN_POINT ( 'NONE',  ( -61.79211991636739754, 31.00000000000000711, -8.240724169199884486 ) ) ;
#28998 = CARTESIAN_POINT ( 'NONE',  ( 31.25450476884064699, 40.00000000000000000, 92.02345382966369414 ) ) ;
#28999 = VERTEX_POINT ( 'NONE', #23068 ) ;
#29000 = CARTESIAN_POINT ( 'NONE',  ( 0.000000000000000000, 19.12429268481864142, -114.4126803693777248 ) ) ;
#29001 = EDGE_CURVE ( 'NONE', #31415, #39812, #26321, .T. ) ;
#29002 = CARTESIAN_POINT ( 'NONE',  ( 0.000000000000000000, 0.000000000000000000, 0.000000000000000000 ) ) ;
#29003 = DIRECTION ( 'NONE',  ( -1.000000000000000000, 0.000000000000000000, 0.000000000000000000 ) ) ;
#29004 = EDGE_CURVE ( 'NONE', #40767, #18955, #41604, .T. ) ;
#29005 = AXIS2_PLACEMENT_3D ( 'NONE', #37153, #33895, #27361 ) ;
#29006 = EDGE_CURVE ( 'NONE', #29967, #5490, #26105, .T. ) ;
#29007 = EDGE_CURVE ( 'NONE', #40494, #4914, #39497, .T. ) ;
#29009 = ORIENTED_EDGE ( 'NONE', *, *, #17609, .T. ) ;
#29008 = DIRECTION ( 'NONE',  ( -1.000000000000000000, 0.000000000000000000, -0.000000000000000000 ) ) ;
#29010 = LINE ( 'NONE', #29219, #8625 ) ;
#29011 = CIRCLE ( 'NONE', #38044, 36.00000000000000000 ) ;
#29012 = LINE ( 'NONE', #12847, #10514 ) ;
#29013 = CIRCLE ( 'NONE', #7365, 158.5000000000000284 ) ;
#29014 = EDGE_LOOP ( 'NONE', ( #19331, #11195, #41357, #40862 ) ) ;
#29015 = CARTESIAN_POINT ( 'NONE',  ( 19.99305134020393382, 40.00000000000000000, 74.61661993947731730 ) ) ;
#29016 = CYLINDRICAL_SURFACE ( 'NONE', #5476, 2.649999999999985700 ) ;
#29017 = VECTOR ( 'NONE', #40435, 1000.000000000000000 ) ;
#29018 = ORIENTED_EDGE ( 'NONE', *, *, #11768, .F. ) ;
#29019 = CARTESIAN_POINT ( 'NONE',  ( 155.7547826636224499, -12.05525454449572820, 15.74958860255448734 ) ) ;
#29020 = AXIS2_PLACEMENT_3D ( 'NONE', #18792, #35309, #11558 ) ;
#29021 = AXIS2_PLACEMENT_3D ( 'NONE', #30791, #1085, #20564 ) ;
#29022 = ORIENTED_EDGE ( 'NONE', *, *, #8471, .T. ) ;
#29023 = ORIENTED_EDGE ( 'NONE', *, *, #29202, .F. ) ;
#29024 = DIRECTION ( 'NONE',  ( -1.000000000000000000, 0.000000000000000000, -0.000000000000000000 ) ) ;
#29025 = ORIENTED_EDGE ( 'NONE', *, *, #17151, .T. ) ;
#29026 = DIRECTION ( 'NONE',  ( 0.000000000000000000, 0.000000000000000000, 1.000000000000000000 ) ) ;
#29027 = DIRECTION ( 'NONE',  ( 0.000000000000000000, 0.4610925014493207352, 0.8873520750565743187 ) ) ;
#29028 = CYLINDRICAL_SURFACE ( 'NONE', #7964, 116.0000000000000000 ) ;
#29029 = LINE ( 'NONE', #17018, #6674 ) ;
#29030 = EDGE_LOOP ( 'NONE', ( #16352, #23213, #25871, #2730 ) ) ;
#29031 = CARTESIAN_POINT ( 'NONE',  ( 18.00000000000000355, 47.22458491092827160, -5.098390039073737334 ) ) ;
#29032 = UNCERTAINTY_MEASURE_WITH_UNIT (LENGTH_MEASURE( 1.000000000000000082E-05 ), #12352, 'distance_accuracy_value', 'NONE');
#29033 = ORIENTED_EDGE ( 'NONE', *, *, #23518, .T. ) ;
#29034 = DIRECTION ( 'NONE',  ( 1.000000000000000000, 0.000000000000000000, 0.000000000000000000 ) ) ;
#29035 = EDGE_CURVE ( 'NONE', #35216, #22361, #10981, .T. ) ;
#29037 = VERTEX_POINT ( 'NONE', #9070 ) ;
#29036 = CIRCLE ( 'NONE', #429, 47.49900000000000233 ) ;
#29038 = CARTESIAN_POINT ( 'NONE',  ( 18.00000000000000355, -19.74581912682875284, 48.10512059033386123 ) ) ;
#29039 = AXIS2_PLACEMENT_3D ( 'NONE', #35590, #39075, #15362 ) ;
#29040 = DIRECTION ( 'NONE',  ( 0.000000000000000000, 0.000000000000000000, 1.000000000000000000 ) ) ;
#29041 = VECTOR ( 'NONE', #20678, 1000.000000000000000 ) ;
#29042 = CIRCLE ( 'NONE', #3920, 20.00000000000000711 ) ;
#29043 =( LENGTH_UNIT ( ) NAMED_UNIT ( * ) SI_UNIT ( .MILLI., .METRE. ) );
#29044 = FACE_OUTER_BOUND ( 'NONE', #42545, .T. ) ;
#29045 = CARTESIAN_POINT ( 'NONE',  ( -57.43240763726046794, 31.00000000000000355, -19.49446143887317717 ) ) ;
#29046 = ORIENTED_EDGE ( 'NONE', *, *, #18809, .T. ) ;
#29047 = CARTESIAN_POINT ( 'NONE',  ( -6.075999999999999623, 1.847259681127465666E-15, -15.08402000000000065 ) ) ;
#29048 = ORIENTED_EDGE ( 'NONE', *, *, #12799, .T. ) ;
#29049 = CARTESIAN_POINT ( 'NONE',  ( -47.15756294055117337, 40.00000000000000000, -53.75246728999482571 ) ) ;
#29050 = VECTOR ( 'NONE', #13309, 1000.000000000000000 ) ;
#29051 = FACE_OUTER_BOUND ( 'NONE', #31375, .T. ) ;
#29052 = CARTESIAN_POINT ( 'NONE',  ( 17.99999999999999645, 0.000000000000000000, 0.000000000000000000 ) ) ;
#29053 = AXIS2_PLACEMENT_3D ( 'NONE', #28030, #4423, #11660 ) ;
#29054 = EDGE_CURVE ( 'NONE', #40989, #7683, #42986, .T. ) ;
#29055 = EDGE_CURVE ( 'NONE', #7775, #10543, #36316, .T. ) ;
#29056 = FACE_OUTER_BOUND ( 'NONE', #6879, .T. ) ;
#29057 = DIRECTION ( 'NONE',  ( 0.000000000000000000, 0.000000000000000000, 1.000000000000000000 ) ) ;
#29058 = PRODUCT ( 'housing right', 'housing right', '', ( #21458 ) ) ;
#29059 = ADVANCED_FACE ( 'NONE', ( #9283 ), #6433, .F. ) ;
#29060 = VERTEX_POINT ( 'NONE', #25901 ) ;
#29061 = CARTESIAN_POINT ( 'NONE',  ( 34.77048308403384169, 40.00000000000000000, 30.48958026498159768 ) ) ;
#29062 = DIRECTION ( 'NONE',  ( 0.000000000000000000, 0.4610925014493207352, 0.8873520750565742077 ) ) ;
#29063 = DIRECTION ( 'NONE',  ( -0.2604563316218753699, 0.000000000000000000, -0.9654856287475622745 ) ) ;
#29064 = ORIENTED_EDGE ( 'NONE', *, *, #13849, .F. ) ;
#29065 = CIRCLE ( 'NONE', #13032, 47.49900000000000233 ) ;
#29066 = CARTESIAN_POINT ( 'NONE',  ( 0.000000000000000000, 8.827181066047511848, -120.1772519049558667 ) ) ;
#29067 = ORIENTED_EDGE ( 'NONE', *, *, #21426, .T. ) ;
#29068 = VERTEX_POINT ( 'NONE', #3135 ) ;
#29069 = CIRCLE ( 'NONE', #32533, 15.08402000000000065 ) ;
#29070 = VERTEX_POINT ( 'NONE', #39157 ) ;
#29071 = AXIS2_PLACEMENT_3D ( 'NONE', #7017, #40165, #23647 ) ;
#29072 = DIRECTION ( 'NONE',  ( 0.3211947320043963550, 0.000000000000000000, -0.9470131699890049770 ) ) ;
#29073 = CIRCLE ( 'NONE', #37423, 47.49900000000000233 ) ;
#29074 = EDGE_CURVE ( 'NONE', #31975, #36084, #22636, .T. ) ;
#29075 = CARTESIAN_POINT ( 'NONE',  ( -65.95487968126425926, 31.00000000000000711, -50.74205456613862708 ) ) ;
#29076 = ORIENTED_EDGE ( 'NONE', *, *, #30741, .F. ) ;
#29077 = DIRECTION ( 'NONE',  ( -1.000000000000000000, 0.000000000000000000, -0.000000000000000000 ) ) ;
#29078 = CARTESIAN_POINT ( 'NONE',  ( 42.80287614962796994, -2.055254544495723756, 69.29271901957280022 ) ) ;
#29079 = ORIENTED_EDGE ( 'NONE', *, *, #41089, .T. ) ;
#29080 = DIRECTION ( 'NONE',  ( 0.000000000000000000, 0.4817536741017102164, 0.8763066800438664705 ) ) ;
#29081 = CIRCLE ( 'NONE', #15180, 20.00000000000000711 ) ;
#29082 = CARTESIAN_POINT ( 'NONE',  ( -101.9001375415117963, 40.00000000000000711, 6.549163350515033066 ) ) ;
#29083 = AXIS2_PLACEMENT_3D ( 'NONE', #3981, #33459, #36495 ) ;
#29084 = DIRECTION ( 'NONE',  ( -1.000000000000000000, 0.000000000000000000, -0.000000000000000000 ) ) ;
#29086 = CARTESIAN_POINT ( 'NONE',  ( 17.99999999999999645, 104.6166166098445416, 50.11350645393712000 ) ) ;
#29085 = DIRECTION ( 'NONE',  ( -1.000000000000000000, 0.000000000000000000, -0.000000000000000000 ) ) ;
#29087 = DIRECTION ( 'NONE',  ( 0.000000000000000000, 0.6845471059286899473, -0.7289686274214103312 ) ) ;
#29088 = ADVANCED_FACE ( 'NONE', ( #16074 ), #20432, .T. ) ;
#29089 = DIRECTION ( 'NONE',  ( 1.000000000000000000, 0.000000000000000000, 0.000000000000000000 ) ) ;
#29090 = ORIENTED_EDGE ( 'NONE', *, *, #10874, .F. ) ;
#29091 = CARTESIAN_POINT ( 'NONE',  ( -27.97094176822542977, 31.00000000000000355, 9.504947828999611659 ) ) ;
#29092 = ORIENTED_EDGE ( 'NONE', *, *, #3346, .T. ) ;
#29093 = CARTESIAN_POINT ( 'NONE',  ( 0.000000000000000000, -3.803237743091689715, -31.26855263151018960 ) ) ;
#29094 = CARTESIAN_POINT ( 'NONE',  ( 106.4195705685763471, -106.4195705685744855, 9.999999999999998224 ) ) ;
#29095 = AXIS2_PLACEMENT_3D ( 'NONE', #31313, #14530, #31092 ) ;
#29096 = EDGE_LOOP ( 'NONE', ( #14030, #26019, #17618, #6765, #1843 ) ) ;
#29097 = CARTESIAN_POINT ( 'NONE',  ( -23.46968090759046888, 40.00000000000000000, -20.57717900685300449 ) ) ;
#29098 = AXIS2_PLACEMENT_3D ( 'NONE', #28627, #28835, #38207 ) ;
#29099 = CARTESIAN_POINT ( 'NONE',  ( -4.434938641671375414, 40.00000000000000000, -34.07637162044569834 ) ) ;
#29100 = CIRCLE ( 'NONE', #17986, 31.49899999999999523 ) ;
#29101 = AXIS2_PLACEMENT_3D ( 'NONE', #33045, #29581, #19567 ) ;
#29102 = ORIENTED_EDGE ( 'NONE', *, *, #12238, .F. ) ;
#29103 = AXIS2_PLACEMENT_3D ( 'NONE', #11041, #4236, #7086 ) ;
#29104 = ORIENTED_EDGE ( 'NONE', *, *, #29165, .F. ) ;
#29105 = EDGE_CURVE ( 'NONE', #7662, #31862, #21456, .T. ) ;
#29106 = CARTESIAN_POINT ( 'NONE',  ( 8.999999999999998224, 54.09091620264857880, -102.6166301549512525 ) ) ;
#29107 = DIRECTION ( 'NONE',  ( 0.000000000000000000, 0.9968120070307504577, -0.07978610555307970309 ) ) ;
#29108 = AXIS2_PLACEMENT_3D ( 'NONE', #42592, #19098, #26473 ) ;
#29109 = EDGE_CURVE ( 'NONE', #36509, #34854, #24939, .T. ) ;
#29110 = FACE_OUTER_BOUND ( 'NONE', #33338, .T. ) ;
#29111 = DIRECTION ( 'NONE',  ( -3.009274222672345096E-17, -1.000000000000000000, 2.455023325076454960E-18 ) ) ;
#29112 = CARTESIAN_POINT ( 'NONE',  ( 0.000000000000000000, 96.25468616236763353, -72.49500943364391503 ) ) ;
#29113 = ORIENTED_EDGE ( 'NONE', *, *, #28914, .F. ) ;
#29114 = CARTESIAN_POINT ( 'NONE',  ( 18.00000000000000355, 11.90021268425555512, 45.45261810511218670 ) ) ;
#29115 = VERTEX_POINT ( 'NONE', #10367 ) ;
#29116 = CARTESIAN_POINT ( 'NONE',  ( 17.99999999999999645, -91.51415974874635140, 64.91094698989267897 ) ) ;
#29117 = CARTESIAN_POINT ( 'NONE',  ( 21.00000000000000355, 0.000000000000000000, 2.055000000000000160 ) ) ;
#29118 = EDGE_CURVE ( 'NONE', #4572, #28151, #26304, .T. ) ;
#29119 = DIRECTION ( 'NONE',  ( 1.000000000000000000, 0.000000000000000000, 0.000000000000000000 ) ) ;
#29120 = CARTESIAN_POINT ( 'NONE',  ( 17.99999999999999645, -59.07817985939071548, 105.0250430397506847 ) ) ;
#29121 = ORIENTED_EDGE ( 'NONE', *, *, #16862, .T. ) ;
#29122 = CARTESIAN_POINT ( 'NONE',  ( -81.55297449308174862, 40.00000000000000711, -40.20044092665353475 ) ) ;
#29123 = ORIENTED_EDGE ( 'NONE', *, *, #8092, .F. ) ;
#29124 = CARTESIAN_POINT ( 'NONE',  ( 1.600000000000000089, -12.75000000000000000, 0.000000000000000000 ) ) ;
#29125 = EDGE_CURVE ( 'NONE', #11603, #9979, #27386, .T. ) ;
#29126 = ORIENTED_EDGE ( 'NONE', *, *, #6545, .F. ) ;
#29128 = EDGE_LOOP ( 'NONE', ( #35680, #28111, #28807, #17313 ) ) ;
#29127 = CARTESIAN_POINT ( 'NONE',  ( 23.00000000000000000, 2.816687638038912352E-15, -20.00000000000000000 ) ) ;
#29129 = EDGE_CURVE ( 'NONE', #34690, #12201, #37613, .T. ) ;
#29130 = CARTESIAN_POINT ( 'NONE',  ( 7.251580242022521716, 31.00000000000000355, -54.34182998361462325 ) ) ;
#29131 = VERTEX_POINT ( 'NONE', #40879 ) ;
#29132 = DIRECTION ( 'NONE',  ( 0.000000000000000000, 0.000000000000000000, 1.000000000000000000 ) ) ;
#29133 = AXIS2_PLACEMENT_3D ( 'NONE', #9875, #13610, #10529 ) ;
#29134 = VECTOR ( 'NONE', #10914, 1000.000000000000000 ) ;
#29135 = AXIS2_PLACEMENT_3D ( 'NONE', #24689, #38584, #8707 ) ;
#29136 = DIRECTION ( 'NONE',  ( -1.000000000000000000, -0.000000000000000000, 0.000000000000000000 ) ) ;
#29137 = EDGE_LOOP ( 'NONE', ( #36688, #40641, #8163, #26378 ) ) ;
#29138 = AXIS2_PLACEMENT_3D ( 'NONE', #26446, #39716, #29945 ) ;
#29139 = CARTESIAN_POINT ( 'NONE',  ( 58.79931003850258975, 40.00000000000000000, 51.72161244498203558 ) ) ;
#29140 = CIRCLE ( 'NONE', #22225, 59.00000000000000711 ) ;
#29142 = CARTESIAN_POINT ( 'NONE',  ( -109.0695705685748464, -106.4195705685759776, 10.00000000000000000 ) ) ;
#29141 = DIRECTION ( 'NONE',  ( 0.000000000000000000, 0.000000000000000000, 1.000000000000000000 ) ) ;
#29143 = FACE_OUTER_BOUND ( 'NONE', #3972, .T. ) ;
#29144 = ORIENTED_EDGE ( 'NONE', *, *, #4134, .F. ) ;
#29145 = DIRECTION ( 'NONE',  ( -1.000000000000000000, -0.000000000000000000, -0.000000000000000000 ) ) ;
#29146 = VERTEX_POINT ( 'NONE', #11032 ) ;
#29147 = EDGE_CURVE ( 'NONE', #28134, #1396, #11675, .T. ) ;
#29148 = DIRECTION ( 'NONE',  ( 1.000000000000000000, -1.373900992973641868E-15, -3.469446951953632924E-16 ) ) ;
#29149 = CARTESIAN_POINT ( 'NONE',  ( 2.600000000000000533, -12.75000000000000000, 0.000000000000000000 ) ) ;
#29150 = VECTOR ( 'NONE', #315, 1000.000000000000000 ) ;
#29151 = CARTESIAN_POINT ( 'NONE',  ( -77.03666156126601550, 31.00000000000000711, 20.64125776147949409 ) ) ;
#29153 = CARTESIAN_POINT ( 'NONE',  ( 18.00000000000000355, 26.17370628620709638, -39.63700417846136048 ) ) ;
#29152 = CARTESIAN_POINT ( 'NONE',  ( 0.000000000000000000, -75.72520367775034345, -82.78868281116056949 ) ) ;
#29154 = ORIENTED_EDGE ( 'NONE', *, *, #32458, .T. ) ;
#29155 = CARTESIAN_POINT ( 'NONE',  ( 8.999999999999998224, 115.9750404417044081, -2.406240749597859718 ) ) ;
#29156 = ORIENTED_EDGE ( 'NONE', *, *, #9722, .T. ) ;
#29157 = FACE_OUTER_BOUND ( 'NONE', #4977, .T. ) ;
#29158 = CARTESIAN_POINT ( 'NONE',  ( 9.000000000000001776, -115.9387338813861987, 3.769613505535687636 ) ) ;
#29159 = AXIS2_PLACEMENT_3D ( 'NONE', #34296, #40604, #34088 ) ;
#29160 = CARTESIAN_POINT ( 'NONE',  ( -30.16842255227261660, 31.00000000000000355, -89.21315370691763746 ) ) ;
#29161 = AXIS2_PLACEMENT_3D ( 'NONE', #17489, #10690, #11141 ) ;
#29162 = CARTESIAN_POINT ( 'NONE',  ( -70.09526419943651376, 40.00000000000000711, -61.63891210109846241 ) ) ;
#29163 = CARTESIAN_POINT ( 'NONE',  ( 2.500000000000000000, 1.178949249685212974, -2.042000000000001148 ) ) ;
#29164 = AXIS2_PLACEMENT_3D ( 'NONE', #9765, #23322, #36580 ) ;
#29165 = EDGE_CURVE ( 'NONE', #35443, #30139, #24132, .T. ) ;
#29166 = ADVANCED_BREP_SHAPE_REPRESENTATION ( '', ( #27879, #13552 ), #21242 ) ;
#29167 = ORIENTED_EDGE ( 'NONE', *, *, #20931, .F. ) ;
#29168 = CYLINDRICAL_SURFACE ( 'NONE', #40214, 59.00000000000000000 ) ;
#29169 = AXIS2_PLACEMENT_3D ( 'NONE', #27362, #31704, #14934 ) ;
#29170 = EDGE_LOOP ( 'NONE', ( #7314, #1642, #11287, #9243 ) ) ;
#29171 = VECTOR ( 'NONE', #2668, 1000.000000000000000 ) ;
#29172 = DIRECTION ( 'NONE',  ( 1.000000000000000000, 0.000000000000000000, 0.000000000000000000 ) ) ;
#29173 = VECTOR ( 'NONE', #2716, 1000.000000000000000 ) ;
#29174 = DIRECTION ( 'NONE',  ( 0.000000000000000000, 2.305124076552231752E-14, -1.000000000000000000 ) ) ;
#29175 = CARTESIAN_POINT ( 'NONE',  ( 0.000000000000000000, 94.83915810436481308, -59.94836581341496640 ) ) ;
#29176 = ORIENTED_EDGE ( 'NONE', *, *, #29222, .F. ) ;
#29177 = CARTESIAN_POINT ( 'NONE',  ( 17.99999999999999645, 0.000000000000000000, 0.000000000000000000 ) ) ;
#29178 = CARTESIAN_POINT ( 'NONE',  ( 8.999999999999998224, 1.832071611524440088E-15, -14.91999999999999993 ) ) ;
#29179 = EDGE_CURVE ( 'NONE', #39420, #37944, #8882, .T. ) ;
#29180 = DIRECTION ( 'NONE',  ( 0.000000000000000000, 0.000000000000000000, -1.000000000000000000 ) ) ;
#29181 = VERTEX_POINT ( 'NONE', #4228 ) ;
#29182 = DIRECTION ( 'NONE',  ( 0.000000000000000000, 0.9510565162951521989, 0.3090169943749515036 ) ) ;
#29183 = CYLINDRICAL_SURFACE ( 'NONE', #39198, 11.00000000000000000 ) ;
#29185 = VERTEX_POINT ( 'NONE', #33921 ) ;
#29184 = DIRECTION ( 'NONE',  ( -1.000000000000000000, 0.000000000000000000, 0.000000000000000000 ) ) ;
#29186 = ORIENTED_EDGE ( 'NONE', *, *, #8214, .T. ) ;
#29187 = DIRECTION ( 'NONE',  ( 0.000000000000000000, -0.8951632913550663373, 0.4457383557765300375 ) ) ;
#29188 = CARTESIAN_POINT ( 'NONE',  ( -10.00000000000000000, 0.000000000000000000, 0.000000000000000000 ) ) ;
#29189 = CARTESIAN_POINT ( 'NONE',  ( 46.49836147156941735, 40.00000000000000000, -6.043767708841586206 ) ) ;
#29190 = DIRECTION ( 'NONE',  ( 0.000000000000000000, -0.3641605752528294659, 0.9313361774523355452 ) ) ;
#29191 = AXIS2_PLACEMENT_3D ( 'NONE', #37467, #587, #27896 ) ;
#29192 = CARTESIAN_POINT ( 'NONE',  ( 17.99999999999999645, 51.27532863109503580, -99.79535634195073612 ) ) ;
#29193 = DIRECTION ( 'NONE',  ( 1.000000000000000000, 0.000000000000000000, 0.000000000000000000 ) ) ;
#29194 = VERTEX_POINT ( 'NONE', #30446 ) ;
#29195 = AXIS2_PLACEMENT_3D ( 'NONE', #6172, #16026, #19097 ) ;
#29196 = CARTESIAN_POINT ( 'NONE',  ( -2.688821387764050996E-14, -4.618802153517012954, -0.4999999999999995559 ) ) ;
#29197 = EDGE_LOOP ( 'NONE', ( #40075, #34101, #36420, #42342 ) ) ;
#29198 = EDGE_CURVE ( 'NONE', #32870, #32579, #4008, .T. ) ;
#29199 = DIRECTION ( 'NONE',  ( 0.000000000000000000, 0.000000000000000000, 1.000000000000000000 ) ) ;
#29200 = DIRECTION ( 'NONE',  ( 1.000000000000000000, 0.000000000000000000, 0.000000000000000000 ) ) ;
#29202 = EDGE_CURVE ( 'NONE', #25212, #21757, #13881, .T. ) ;
#29201 = CARTESIAN_POINT ( 'NONE',  ( -36.61132647064156487, 31.00000000000000355, -18.04288060775211378 ) ) ;
#29203 = CARTESIAN_POINT ( 'NONE',  ( -1.999999999999999556, 3.464101615137754830, -3.142992957459232795 ) ) ;
#29204 = VERTEX_POINT ( 'NONE', #7517 ) ;
#29205 = DIRECTION ( 'NONE',  ( 3.009274222672345096E-17, 1.000000000000000000, -2.455023325076454960E-18 ) ) ;
#29206 = CARTESIAN_POINT ( 'NONE',  ( 24.08498528996878107, 31.00000000000000355, -89.94621034038658536 ) ) ;
#29207 = LINE ( 'NONE', #22467, #17155 ) ;
#29208 = ORIENTED_EDGE ( 'NONE', *, *, #2675, .T. ) ;
#29209 = CARTESIAN_POINT ( 'NONE',  ( -47.50570208456527155, 31.00000000000000355, -41.80188021843024160 ) ) ;
#29210 = CARTESIAN_POINT ( 'NONE',  ( -28.16914340537297434, 40.00000000000000000, -57.36152490105313007 ) ) ;
#29211 = CARTESIAN_POINT ( 'NONE',  ( 94.17930118497612568, 39.99999999999999289, -12.41473344271720691 ) ) ;
#29212 = ORIENTED_EDGE ( 'NONE', *, *, #41815, .F. ) ;
#29213 = CARTESIAN_POINT ( 'NONE',  ( -1.390230914382372118, -4.043987460488664532, -3.502507215260523665 ) ) ;
#29214 = CARTESIAN_POINT ( 'NONE',  ( 17.99999999999999645, -100.8494052988166345, -65.95368414179013428 ) ) ;
#29215 = LINE ( 'NONE', #22477, #37980 ) ;
#29216 = VECTOR ( 'NONE', #5390, 1000.000000000000000 ) ;
#29218 = ORIENTED_EDGE ( 'NONE', *, *, #632, .F. ) ;
#29217 = CARTESIAN_POINT ( 'NONE',  ( 0.000000000000000000, -96.25468616236712194, 72.49500943364459715 ) ) ;
#29219 = CARTESIAN_POINT ( 'NONE',  ( -132.0000507999999968, 0.000000000000000000, -11.00000000000000000 ) ) ;
#29220 = DIRECTION ( 'NONE',  ( -3.996523416598930318E-16, 2.658563593772947863E-15, 1.000000000000000000 ) ) ;
#29221 = CIRCLE ( 'NONE', #38939, 116.0000000000000000 ) ;
#29222 = EDGE_CURVE ( 'NONE', #12187, #26511, #20757, .T. ) ;
#29223 = ORIENTED_EDGE ( 'NONE', *, *, #39160, .T. ) ;
#29224 = CARTESIAN_POINT ( 'NONE',  ( 18.89933391970155085, 40.00000000000000000, -70.58587736658564893 ) ) ;
#29225 = DIRECTION ( 'NONE',  ( -1.000000000000000000, 0.000000000000000000, 0.000000000000000000 ) ) ;
#29226 = ORIENTED_EDGE ( 'NONE', *, *, #24492, .T. ) ;
#29227 = DIRECTION ( 'NONE',  ( 0.000000000000000000, 0.000000000000000000, 1.000000000000000000 ) ) ;
#29228 = EDGE_CURVE ( 'NONE', #7044, #4975, #22842, .T. ) ;
#29229 = DIRECTION ( 'NONE',  ( 1.000000000000000000, 0.000000000000000000, 0.000000000000000000 ) ) ;
#29230 = EDGE_CURVE ( 'NONE', #23893, #27109, #1201, .T. ) ;
#29231 = ORIENTED_EDGE ( 'NONE', *, *, #21891, .T. ) ;
#29232 = ORIENTED_EDGE ( 'NONE', *, *, #3084, .T. ) ;
#29233 = CARTESIAN_POINT ( 'NONE',  ( 0.000000000000000000, -87.74575819880217864, 75.87280091124446813 ) ) ;
#29234 = ORIENTED_EDGE ( 'NONE', *, *, #9204, .T. ) ;
#29235 = CARTESIAN_POINT ( 'NONE',  ( 17.99999999999999645, 107.5680526044915410, 31.89649718262280231 ) ) ;
#29236 = CARTESIAN_POINT ( 'NONE',  ( 8.999999999999998224, 64.69195966009891663, 96.28577441832274530 ) ) ;
#29237 = CARTESIAN_POINT ( 'NONE',  ( 17.99999999999999645, -107.2885202478269946, 54.86040852957277281 ) ) ;
#29238 = DIRECTION ( 'NONE',  ( 0.000000000000000000, 0.000000000000000000, 1.000000000000000000 ) ) ;
#29239 = ORIENTED_EDGE ( 'NONE', *, *, #26610, .T. ) ;
#29240 = DIRECTION ( 'NONE',  ( 0.000000000000000000, -0.1062934856473723849, 0.9943348002101364269 ) ) ;
#29241 = ORIENTED_EDGE ( 'NONE', *, *, #9323, .T. ) ;
#29242 = AXIS2_PLACEMENT_3D ( 'NONE', #9302, #28971, #42243 ) ;
#29243 = CARTESIAN_POINT ( 'NONE',  ( -10.00000000000000000, 0.000000000000000000, 0.000000000000000000 ) ) ;
#29244 = ADVANCED_FACE ( 'NONE', ( #20223 ), #13443, .F. ) ;
#29246 = EDGE_CURVE ( 'NONE', #41404, #42055, #16942, .T. ) ;
#29245 = CIRCLE ( 'NONE', #10453, 31.49899999999999523 ) ;
#29247 = EDGE_LOOP ( 'NONE', ( #26064, #27147, #36123, #40395 ) ) ;
#29248 = AXIS2_PLACEMENT_3D ( 'NONE', #16215, #10298, #23643 ) ;
#29249 = CARTESIAN_POINT ( 'NONE',  ( 17.99999999999999645, -80.02407177073008882, 78.64108602299921813 ) ) ;
#29250 = ADVANCED_FACE ( 'NONE', ( #13658 ), #26956, .T. ) ;
#29251 = ADVANCED_FACE ( 'NONE', ( #27175 ), #15396, .F. ) ;
#29252 = ADVANCED_FACE ( 'NONE', ( #5101, #4675 ), #11242, .F. ) ;
#29253 = DIRECTION ( 'NONE',  ( 0.000000000000000000, 0.8443279255020126328, 0.5358267949790005424 ) ) ;
#29254 = AXIS2_PLACEMENT_3D ( 'NONE', #39903, #38165, #7841 ) ;
#29255 = CONTEXT_DEPENDENT_SHAPE_REPRESENTATION ( #8616, #26631 ) ;
#29256 = DIRECTION ( 'NONE',  ( -1.000000000000000000, 0.000000000000000000, 0.000000000000000000 ) ) ;
#29257 = CARTESIAN_POINT ( 'NONE',  ( 55.68207322489292466, 31.00000000000000000, -32.16283696845439266 ) ) ;
#29258 = DIRECTION ( 'NONE',  ( 3.009274222672345096E-17, 1.000000000000000000, -2.455023325076455345E-18 ) ) ;
#29259 = ORIENTED_EDGE ( 'NONE', *, *, #15817, .F. ) ;
#29260 = CARTESIAN_POINT ( 'NONE',  ( 35.42814233785335176, 31.00000000000000355, -9.427541829740359702 ) ) ;
#29261 = CARTESIAN_POINT ( 'NONE',  ( 18.89933391970155085, 40.00000000000000000, -70.58587736658564893 ) ) ;
#29262 = CYLINDRICAL_SURFACE ( 'NONE', #14440, 120.5010000000000190 ) ;
#29263 = DIRECTION ( 'NONE',  ( -1.000000000000000000, 0.000000000000000000, -0.000000000000000000 ) ) ;
#29264 = LINE ( 'NONE', #25990, #8595 ) ;
#29265 = DIRECTION ( 'NONE',  ( 0.000000000000000000, 0.000000000000000000, 1.000000000000000000 ) ) ;
#29266 = EDGE_CURVE ( 'NONE', #30887, #31904, #1892, .T. ) ;
#29267 = ORIENTED_EDGE ( 'NONE', *, *, #32087, .F. ) ;
#29268 = CARTESIAN_POINT ( 'NONE',  ( -6.238242335983215092, 40.00000000000000000, 47.40213128959678102 ) ) ;
#29269 = DIRECTION ( 'NONE',  ( 0.000000000000000000, 0.2486898871648552389, -0.9685831611286310761 ) ) ;
#29270 = CARTESIAN_POINT ( 'NONE',  ( 0.000000000000000000, 14.84191762912315049, 27.78316904333131276 ) ) ;
#29271 = VECTOR ( 'NONE', #41353, 1000.000000000000000 ) ;
#29272 = ORIENTED_EDGE ( 'NONE', *, *, #35516, .F. ) ;
#29273 = EDGE_CURVE ( 'NONE', #17801, #27564, #4666, .T. ) ;
#29274 = CIRCLE ( 'NONE', #2753, 116.0000000000000000 ) ;
#29275 = CARTESIAN_POINT ( 'NONE',  ( 18.00000000000000355, 19.44205635905601781, -43.33776004284589334 ) ) ;
#29276 = CARTESIAN_POINT ( 'NONE',  ( 9.000000000000000000, -34.78944633786272789, -9.257128253673986507 ) ) ;
#29277 = VERTEX_POINT ( 'NONE', #41531 ) ;
#29278 = DIRECTION ( 'NONE',  ( 0.000000000000000000, 0.000000000000000000, 1.000000000000000000 ) ) ;
#29279 = ORIENTED_EDGE ( 'NONE', *, *, #15882, .F. ) ;
#29280 = ORIENTED_EDGE ( 'NONE', *, *, #10787, .T. ) ;
#29281 = CARTESIAN_POINT ( 'NONE',  ( 18.00000000000000355, 0.000000000000000000, 0.000000000000000000 ) ) ;
#29282 = CARTESIAN_POINT ( 'NONE',  ( -50.81742119984753714, 31.00000000000000355, -66.42451308377114572 ) ) ;
#29283 = VERTEX_POINT ( 'NONE', #25427 ) ;
#29284 = FACE_OUTER_BOUND ( 'NONE', #28209, .T. ) ;
#29285 = DIRECTION ( 'NONE',  ( 0.000000000000000000, 0.000000000000000000, 1.000000000000000000 ) ) ;
#29286 = DIRECTION ( 'NONE',  ( -1.000000000000000000, -0.000000000000000000, -0.000000000000000000 ) ) ;
#29287 = EDGE_LOOP ( 'NONE', ( #8732, #32763, #13139, #25402 ) ) ;
#29288 = DIRECTION ( 'NONE',  ( 0.000000000000000000, 0.000000000000000000, 1.000000000000000000 ) ) ;
#29289 = CARTESIAN_POINT ( 'NONE',  ( 17.99999999999999645, 0.000000000000000000, 0.000000000000000000 ) ) ;
#29290 = DIRECTION ( 'NONE',  ( -1.000000000000000000, 0.000000000000000000, 0.000000000000000000 ) ) ;
#29291 = ADVANCED_FACE ( 'NONE', ( #8587 ), #18047, .T. ) ;
#29293 = CARTESIAN_POINT ( 'NONE',  ( 0.000000000000000000, 104.2166695095720854, -60.49278301857700768 ) ) ;
#29292 = DIRECTION ( 'NONE',  ( -1.000000000000000000, -0.000000000000000000, -0.000000000000000000 ) ) ;
#29294 = EDGE_CURVE ( 'NONE', #42378, #37373, #12361, .T. ) ;
#29295 = EDGE_CURVE ( 'NONE', #3091, #6921, #24240, .T. ) ;
#29296 = DIRECTION ( 'NONE',  ( 0.000000000000000000, 0.000000000000000000, 1.000000000000000000 ) ) ;
#29297 = ORIENTED_EDGE ( 'NONE', *, *, #2975, .F. ) ;
#29298 = DIRECTION ( 'NONE',  ( 1.000000000000000000, 0.000000000000000000, 0.000000000000000000 ) ) ;
#29299 = EDGE_CURVE ( 'NONE', #38233, #22186, #11895, .T. ) ;
#29300 = CARTESIAN_POINT ( 'NONE',  ( -28.96462450050677973, 31.00000000000000355, -9.827991688575851370 ) ) ;
#29301 = ORIENTED_EDGE ( 'NONE', *, *, #42164, .T. ) ;
#29302 = FACE_OUTER_BOUND ( 'NONE', #20429, .T. ) ;
#29303 = CIRCLE ( 'NONE', #28628, 59.00000000000000000 ) ;
#29304 = DIRECTION ( 'NONE',  ( 1.000000000000000000, 0.000000000000000000, 0.000000000000000000 ) ) ;
#29305 = VERTEX_POINT ( 'NONE', #4894 ) ;
#29306 = VECTOR ( 'NONE', #37935, 1000.000000000000000 ) ;
#29307 = CARTESIAN_POINT ( 'NONE',  ( 8.999999999999998224, 19.47322409167312429, -30.27859877001379374 ) ) ;
#29308 = CARTESIAN_POINT ( 'NONE',  ( 18.38119342899891961, 40.00000000000000000, 31.81670425098764099 ) ) ;
#29309 = CARTESIAN_POINT ( 'NONE',  ( 35.58384423644164229, 40.00000000000000000, 12.14845634898874494 ) ) ;
#29310 = ORIENTED_EDGE ( 'NONE', *, *, #27414, .T. ) ;
#29311 = ORIENTED_EDGE ( 'NONE', *, *, #16732, .F. ) ;
#29312 = DIRECTION ( 'NONE',  ( 0.000000000000000000, 0.000000000000000000, 1.000000000000000000 ) ) ;
#29313 = DIRECTION ( 'NONE',  ( 1.000000000000000000, 0.000000000000000000, 0.000000000000000000 ) ) ;
#29314 = DIRECTION ( 'NONE',  ( 1.000000000000000000, -0.000000000000000000, -0.000000000000000000 ) ) ;
#29315 = LINE ( 'NONE', #39531, #22505 ) ;
#29316 = CARTESIAN_POINT ( 'NONE',  ( 18.00000000000000355, -2.123073309835499245, 47.45152853935333326 ) ) ;
#29317 = EDGE_LOOP ( 'NONE', ( #9685, #10240, #9867, #35740 ) ) ;
#29318 = CARTESIAN_POINT ( 'NONE',  ( 9.000000000000001776, -24.47917365149977798, 45.87777302070926311 ) ) ;
#29319 = ORIENTED_EDGE ( 'NONE', *, *, #27354, .F. ) ;
#29320 = CARTESIAN_POINT ( 'NONE',  ( 17.99999999999999645, 31.80866420683995699, -2.997093558040963224 ) ) ;
#29321 = DIRECTION ( 'NONE',  ( 1.000000000000000000, 0.000000000000000000, 0.000000000000000000 ) ) ;
#29322 = AXIS2_PLACEMENT_3D ( 'NONE', #391, #35973, #6513 ) ;
#29323 = ADVANCED_FACE ( 'NONE', ( #35204 ), #21948, .F. ) ;
#29324 = DIRECTION ( 'NONE',  ( 1.000000000000000000, 0.000000000000000000, 0.000000000000000000 ) ) ;
#29325 = DIRECTION ( 'NONE',  ( -1.000000000000000000, 0.000000000000000000, 0.000000000000000000 ) ) ;
#29326 = ORIENTED_EDGE ( 'NONE', *, *, #17310, .F. ) ;
#29327 = CARTESIAN_POINT ( 'NONE',  ( 18.00000000000000355, -22.82995208772716467, 41.06517797613655318 ) ) ;
#29328 = ORIENTED_EDGE ( 'NONE', *, *, #25976, .T. ) ;
#29329 = AXIS2_PLACEMENT_3D ( 'NONE', #16309, #29614, #32444 ) ;
#29330 = EDGE_CURVE ( 'NONE', #40120, #710, #40179, .T. ) ;
#29331 = DIRECTION ( 'NONE',  ( 1.000000000000000000, 0.000000000000000000, 0.000000000000000000 ) ) ;
#29332 = AXIS2_PLACEMENT_3D ( 'NONE', #39811, #35896, #23287 ) ;
#29333 = ORIENTED_EDGE ( 'NONE', *, *, #17549, .T. ) ;
#29335 = EDGE_LOOP ( 'NONE', ( #21063, #10003, #32266, #29582 ) ) ;
#29334 = DIRECTION ( 'NONE',  ( -3.996523416598930318E-16, 2.658563593772947863E-15, 1.000000000000000000 ) ) ;
#29336 = CIRCLE ( 'NONE', #39045, 13.59999999999999787 ) ;
#29337 = CARTESIAN_POINT ( 'NONE',  ( -7.015336270751801884, 31.00000000000000355, -53.95087245963820521 ) ) ;
#29339 = ORIENTED_EDGE ( 'NONE', *, *, #20884, .F. ) ;
#29338 = AXIS2_PLACEMENT_3D ( 'NONE', #15467, #8665, #5176 ) ;
#29340 = CARTESIAN_POINT ( 'NONE',  ( 17.99999999999999645, -75.03166794516737070, -94.29071961951585479 ) ) ;
#29341 = AXIS2_PLACEMENT_3D ( 'NONE', #32053, #12433, #19003 ) ;
#29342 = ORIENTED_EDGE ( 'NONE', *, *, #9407, .T. ) ;
#29343 = LINE ( 'NONE', #32600, #9133 ) ;
#29344 = ORIENTED_EDGE ( 'NONE', *, *, #6001, .F. ) ;
#29345 = CARTESIAN_POINT ( 'NONE',  ( 24.27443280711675655, 40.00000000000000000, -71.15176282235543681 ) ) ;
#29346 = CIRCLE ( 'NONE', #37012, 13.59999999999999787 ) ;
#29348 = CARTESIAN_POINT ( 'NONE',  ( 0.000000000000000000, -112.1427988504407551, -3.502162136924565239 ) ) ;
#29347 = DIRECTION ( 'NONE',  ( -1.000000000000000000, 0.000000000000000000, 0.000000000000000000 ) ) ;
#29349 = EDGE_CURVE ( 'NONE', #9628, #38193, #2559, .T. ) ;
#29350 = CARTESIAN_POINT ( 'NONE',  ( 17.99999999999999645, 0.5156212287279957618, 112.1962860721878172 ) ) ;
#29351 = ORIENTED_EDGE ( 'NONE', *, *, #42625, .F. ) ;
#29352 = CYLINDRICAL_SURFACE ( 'NONE', #3525, 4.500000000000002665 ) ;
#29353 = ORIENTED_EDGE ( 'NONE', *, *, #23698, .T. ) ;
#29354 =( NAMED_UNIT ( * ) PLANE_ANGLE_UNIT ( ) SI_UNIT ( $, .RADIAN. ) );
#29355 = ADVANCED_FACE ( 'NONE', ( #41961, #1393 ), #11684, .T. ) ;
#29356 = CARTESIAN_POINT ( 'NONE',  ( 0.000000000000000000, 95.31344542257821217, -66.11616384574354299 ) ) ;
#29357 = CARTESIAN_POINT ( 'NONE',  ( 0.000000000000000000, 0.000000000000000000, 0.000000000000000000 ) ) ;
#29358 = CARTESIAN_POINT ( 'NONE',  ( 57.37208743749949491, 31.00000000000000355, 50.31438278193533620 ) ) ;
#29360 = CARTESIAN_POINT ( 'NONE',  ( 18.00000000000000355, -17.08890430202718491, -43.76671000081963570 ) ) ;
#29359 = CARTESIAN_POINT ( 'NONE',  ( 17.99999999999999645, 71.21168426767107462, 86.70160608319346807 ) ) ;
#29361 = ORIENTED_EDGE ( 'NONE', *, *, #34845, .F. ) ;
#29362 = EDGE_CURVE ( 'NONE', #30346, #38270, #21312, .T. ) ;
#29363 = DIRECTION ( 'NONE',  ( -1.000000000000000000, -0.000000000000000000, -0.000000000000000000 ) ) ;
#29364 = CIRCLE ( 'NONE', #24504, 116.0000000000000000 ) ;
#29365 = CIRCLE ( 'NONE', #28693, 116.0000000000000000 ) ;
#29366 = EDGE_CURVE ( 'NONE', #13380, #41947, #36011, .T. ) ;
#29367 = ORIENTED_EDGE ( 'NONE', *, *, #22087, .F. ) ;
#29368 = DIRECTION ( 'NONE',  ( -1.000000000000000000, 0.000000000000000000, 0.000000000000000000 ) ) ;
#29369 = DIRECTION ( 'NONE',  ( 0.000000000000000000, 0.7865515558026394682, 0.6175246149461958156 ) ) ;
#29370 = CARTESIAN_POINT ( 'NONE',  ( 47.87658044097961607, 31.00000000000000000, -82.67148682534870829 ) ) ;
#29371 = CARTESIAN_POINT ( 'NONE',  ( -44.52253807734693680, 40.00000000000000000, 90.03212995793734308 ) ) ;
#29372 = CIRCLE ( 'NONE', #35596, 20.00000000000000000 ) ;
#29373 = DIRECTION ( 'NONE',  ( 1.000000000000000000, 0.000000000000000000, 0.000000000000000000 ) ) ;
#29374 = EDGE_LOOP ( 'NONE', ( #6537, #15665 ) ) ;
#29375 = CARTESIAN_POINT ( 'NONE',  ( 0.000000000000000000, -13.57797752207946829, 33.34124362422470256 ) ) ;
#29376 = EDGE_LOOP ( 'NONE', ( #6011, #29767, #12489, #12132 ) ) ;
#29377 = VECTOR ( 'NONE', #26179, 1000.000000000000000 ) ;
#29378 = CARTESIAN_POINT ( 'NONE',  ( 18.00000000000000355, 40.47821179127761582, -32.64221760512715065 ) ) ;
#29379 = DIRECTION ( 'NONE',  ( -1.058513553088275437E-16, -1.000000000000000000, 8.813324511995299047E-17 ) ) ;
#29380 = DIRECTION ( 'NONE',  ( 0.000000000000000000, 0.000000000000000000, 1.000000000000000000 ) ) ;
#29381 = ORIENTED_EDGE ( 'NONE', *, *, #24709, .T. ) ;
#29382 = DIRECTION ( 'NONE',  ( -1.000000000000000000, 0.000000000000000000, -0.000000000000000000 ) ) ;
#29383 = CARTESIAN_POINT ( 'NONE',  ( 17.99999999999999645, -34.03109950475653989, -115.5957406979053133 ) ) ;
#29384 = DIRECTION ( 'NONE',  ( 0.000000000000000000, 0.1253332335643045359, -0.9921147013144778759 ) ) ;
#29386 = ORIENTED_EDGE ( 'NONE', *, *, #31777, .T. ) ;
#29385 = FACE_OUTER_BOUND ( 'NONE', #30922, .T. ) ;
#29387 = CARTESIAN_POINT ( 'NONE',  ( 16.96065435355024320, 31.00000000000000355, -19.31014141889295388 ) ) ;
#29388 = CARTESIAN_POINT ( 'NONE',  ( -10.00000000000000000, 0.000000000000000000, 0.000000000000000000 ) ) ;
#29390 = ORIENTED_EDGE ( 'NONE', *, *, #20427, .F. ) ;
#29389 = CARTESIAN_POINT ( 'NONE',  ( 65.39325745242679488, -2.055254544495723756, 58.58409293616905700 ) ) ;
#29391 = ORIENTED_EDGE ( 'NONE', *, *, #41286, .F. ) ;
#29392 = DIRECTION ( 'NONE',  ( -1.000000000000000000, 0.000000000000000000, 0.000000000000000000 ) ) ;
#29393 = AXIS2_PLACEMENT_3D ( 'NONE', #36934, #3330, #700 ) ;
#29394 = DIRECTION ( 'NONE',  ( -1.000000000000000000, 0.000000000000000000, 0.000000000000000000 ) ) ;
#29395 = CARTESIAN_POINT ( 'NONE',  ( 29.49207856986237530, 40.00000000000000000, 38.57905506995709288 ) ) ;
#29396 = DIRECTION ( 'NONE',  ( 0.000000000000000000, 0.000000000000000000, 1.000000000000000000 ) ) ;
#29397 = CIRCLE ( 'NONE', #34263, 13.59999999999999787 ) ;
#29398 = DIRECTION ( 'NONE',  ( -1.000000000000000000, 0.000000000000000000, 0.000000000000000000 ) ) ;
#29399 = AXIS2_PLACEMENT_3D ( 'NONE', #29481, #9182, #35771 ) ;
#29400 = ADVANCED_FACE ( 'NONE', ( #1177 ), #28049, .F. ) ;
#29401 = CARTESIAN_POINT ( 'NONE',  ( 9.000000000000001776, -44.25018368420761306, 27.31155879685165644 ) ) ;
#29402 = ORIENTED_EDGE ( 'NONE', *, *, #3401, .T. ) ;
#29403 = CYLINDRICAL_SURFACE ( 'NONE', #16101, 59.00000000000000000 ) ;
#29404 = ORIENTED_EDGE ( 'NONE', *, *, #7738, .T. ) ;
#29405 = AXIS2_PLACEMENT_3D ( 'NONE', #6616, #29778, #12985 ) ;
#29406 = DIRECTION ( 'NONE',  ( -1.000000000000000000, 0.000000000000000000, 0.000000000000000000 ) ) ;
#29407 = CARTESIAN_POINT ( 'NONE',  ( 18.00000000000000355, 51.19683565102443623, 9.104066087303637644 ) ) ;
#29408 = CARTESIAN_POINT ( 'NONE',  ( -31.39472673864601049, 31.00000000000000355, -40.91112553188754930 ) ) ;
#29409 = DIRECTION ( 'NONE',  ( 0.000000000000000000, 0.3140767120219495334, -0.9493976084683810601 ) ) ;
#29410 = ORIENTED_EDGE ( 'NONE', *, *, #17961, .T. ) ;
#29411 = ADVANCED_FACE ( 'NONE', ( #31521 ), #1608, .T. ) ;
#29412 = PRODUCT ( 'circlip for shafts normal_din_Circlip DIN 471 - 22 x 1.2', 'circlip for shafts normal_din_Circlip DIN 471 - 22 x 1.2', '', ( #34920 ) ) ;
#29413 = CARTESIAN_POINT ( 'NONE',  ( 53.80287614962789178, -14.05525454449572109, 69.29271901957253021 ) ) ;
#29414 = CARTESIAN_POINT ( 'NONE',  ( 81.15556025174309696, 31.00000000000000000, 27.54985289775053658 ) ) ;
#29415 = EDGE_CURVE ( 'NONE', #8485, #2740, #21486, .T. ) ;
#29416 = DIRECTION ( 'NONE',  ( 0.000000000000000000, 0.000000000000000000, -1.000000000000000000 ) ) ;
#29417 = ORIENTED_EDGE ( 'NONE', *, *, #30910, .T. ) ;
#29418 = CARTESIAN_POINT ( 'NONE',  ( 8.965261019430212031, 31.00000000000000355, 68.85524230650666766 ) ) ;
#29419 = CARTESIAN_POINT ( 'NONE',  ( -71.33925323115938966, 40.00000000000000711, 9.290813765102964084 ) ) ;
#29420 = CARTESIAN_POINT ( 'NONE',  ( 92.36625196220676060, 39.99999999999999289, 24.73319171124347093 ) ) ;
#29421 = AXIS2_PLACEMENT_3D ( 'NONE', #9361, #12458, #6304 ) ;
#29422 = ORIENTED_EDGE ( 'NONE', *, *, #23142, .F. ) ;
#29423 = VECTOR ( 'NONE', #1523, 1000.000000000000000 ) ;
#29424 = VECTOR ( 'NONE', #29111, 1000.000000000000000 ) ;
#29425 = DIRECTION ( 'NONE',  ( -0.000000000000000000, -0.000000000000000000, -1.000000000000000000 ) ) ;
#29426 = DIRECTION ( 'NONE',  ( 0.000000000000000000, 0.000000000000000000, 1.000000000000000000 ) ) ;
#29427 = CIRCLE ( 'NONE', #34989, 47.49899999999999523 ) ;
#29429 = VERTEX_POINT ( 'NONE', #2869 ) ;
#29428 = CARTESIAN_POINT ( 'NONE',  ( 17.99999999999999645, 103.5682682299988500, -43.14958040911561454 ) ) ;
#29430 = DIRECTION ( 'NONE',  ( 3.009274222672345096E-17, 1.000000000000000000, -2.455023325076455345E-18 ) ) ;
#29431 = FACE_BOUND ( 'NONE', #34111, .T. ) ;
#29432 = ADVANCED_FACE ( 'NONE', ( #3077 ), #12957, .F. ) ;
#29433 = CARTESIAN_POINT ( 'NONE',  ( 55.63593431945896839, 39.99999999999999289, -48.80962981700470493 ) ) ;
#29434 = LINE ( 'NONE', #39858, #13150 ) ;
#29435 = EDGE_CURVE ( 'NONE', #38773, #30637, #17995, .T. ) ;
#29436 = CIRCLE ( 'NONE', #19669, 59.00000000000000711 ) ;
#29437 = ORIENTED_EDGE ( 'NONE', *, *, #15377, .F. ) ;
#29438 = CARTESIAN_POINT ( 'NONE',  ( 9.000000000000001776, 13.56094713063641599, -50.20060470671725739 ) ) ;
#29439 = ADVANCED_FACE ( 'NONE', ( #19310 ), #5743, .F. ) ;
#29440 = CARTESIAN_POINT ( 'NONE',  ( -126.0000000000000284, 4.615443851143735910E-16, 367.6955262170047263 ) ) ;
#29441 = ORIENTED_EDGE ( 'NONE', *, *, #7287, .F. ) ;
#29442 = ORIENTED_EDGE ( 'NONE', *, *, #26579, .F. ) ;
#29443 = LINE ( 'NONE', #12861, #5160 ) ;
#29444 = ORIENTED_EDGE ( 'NONE', *, *, #14582, .T. ) ;
#29445 = DIRECTION ( 'NONE',  ( 0.000000000000000000, -0.4610925014493143514, -0.8873520750565775383 ) ) ;
#29446 = FACE_OUTER_BOUND ( 'NONE', #1134, .T. ) ;
#29447 = LINE ( 'NONE', #6090, #26817 ) ;
#29448 = CARTESIAN_POINT ( 'NONE',  ( 9.000000000000001776, -115.0622509503833442, 14.72000021165104755 ) ) ;
#29449 = EDGE_LOOP ( 'NONE', ( #27863, #13793, #11928, #20339 ) ) ;
#29450 = DIRECTION ( 'NONE',  ( 1.000000000000000000, -0.000000000000000000, -0.000000000000000000 ) ) ;
#29451 = ADVANCED_FACE ( 'NONE', ( #22583 ), #39109, .F. ) ;
#29452 = PRODUCT_DEFINITION_CONTEXT ( 'detailed design', #15353, 'design' ) ;
#29453 = VERTEX_POINT ( 'NONE', #36261 ) ;
#29454 = AXIS2_PLACEMENT_3D ( 'NONE', #5616, #35916, #29199 ) ;
#29455 = CARTESIAN_POINT ( 'NONE',  ( 6.908545562266867002, -14.05525454449572820, -74.83297477053821467 ) ) ;
#29456 = EDGE_LOOP ( 'NONE', ( #2452, #7556, #28526, #6566 ) ) ;
#29457 = DIRECTION ( 'NONE',  ( -1.000000000000000000, -0.000000000000000000, -0.000000000000000000 ) ) ;
#29458 = VECTOR ( 'NONE', #30292, 1000.000000000000000 ) ;
#29459 = CARTESIAN_POINT ( 'NONE',  ( 5.657435538624008755E-15, 4.615443851143735910E-16, -20.00000000000000000 ) ) ;
#29460 = SHAPE_DEFINITION_REPRESENTATION ( #30124, #41895 ) ;
#29461 = EDGE_CURVE ( 'NONE', #9021, #25059, #11711, .T. ) ;
#29462 = FACE_BOUND ( 'NONE', #40430, .T. ) ;
#29463 = CARTESIAN_POINT ( 'NONE',  ( -59.82155519080263417, 31.00000000000000711, -7.874468279917395286 ) ) ;
#29464 = VECTOR ( 'NONE', #34703, 1000.000000000000000 ) ;
#29465 = CARTESIAN_POINT ( 'NONE',  ( 150.0000507999999968, 0.000000000000000000, 7.500000000000000000 ) ) ;
#29466 = EDGE_CURVE ( 'NONE', #30185, #10881, #5425, .T. ) ;
#29467 = ORIENTED_EDGE ( 'NONE', *, *, #31274, .F. ) ;
#29468 = CARTESIAN_POINT ( 'NONE',  ( -30.84436395684956977, 31.00000000000000355, -10.52363363425319243 ) ) ;
#29469 = CARTESIAN_POINT ( 'NONE',  ( 58.80104710710317306, 39.99999999999999289, -45.11949705600698479 ) ) ;
#29470 = CARTESIAN_POINT ( 'NONE',  ( 18.00000000000000355, 32.32520163883631170, -34.09746168776002406 ) ) ;
#29471 = CARTESIAN_POINT ( 'NONE',  ( 17.99999999999999645, -105.7179949885865256, -37.57629584241794163 ) ) ;
#29472 = CARTESIAN_POINT ( 'NONE',  ( -2.095696658341510008E-13, 150.5000000000013642, 7.000000000000419220 ) ) ;
#29473 = DIRECTION ( 'NONE',  ( 0.000000000000000000, 0.2486898871648483278, 0.9685831611286327414 ) ) ;
#29474 = CIRCLE ( 'NONE', #30900, 36.00000000000000000 ) ;
#29475 = EDGE_LOOP ( 'NONE', ( #18425, #11906, #8928, #23764 ) ) ;
#29476 = CARTESIAN_POINT ( 'NONE',  ( -35.44024466369167925, 40.00000000000000000, -20.45798383175513635 ) ) ;
#29477 = CARTESIAN_POINT ( 'NONE',  ( 0.000000000000000000, 45.89132998248186368, -102.3829004574625401 ) ) ;
#29478 = CARTESIAN_POINT ( 'NONE',  ( -100.0589655806010967, 17.11489954122028578, 21.59728106529621883 ) ) ;
#29479 = VERTEX_POINT ( 'NONE', #29753 ) ;
#29480 = EDGE_CURVE ( 'NONE', #8238, #30765, #34664, .T. ) ;
#29481 = CARTESIAN_POINT ( 'NONE',  ( 17.99999999999999645, -11.49545354908914518, -29.80986809967271967 ) ) ;
#29482 = CARTESIAN_POINT ( 'NONE',  ( -8.749793197483594298, -2.055254544495723756, 2.972870684497274762 ) ) ;
#29483 = EDGE_CURVE ( 'NONE', #39739, #967, #5541, .T. ) ;
#29484 = VERTEX_POINT ( 'NONE', #12321 ) ;
#29485 = CARTESIAN_POINT ( 'NONE',  ( 0.000000000000000000, 0.000000000000000000, -6.000000000000000000 ) ) ;
#29486 = ORIENTED_EDGE ( 'NONE', *, *, #14932, .F. ) ;
#29487 = AXIS2_PLACEMENT_3D ( 'NONE', #35345, #5667, #19025 ) ;
#29488 = ORIENTED_EDGE ( 'NONE', *, *, #29851, .T. ) ;
#29489 = CYLINDRICAL_SURFACE ( 'NONE', #30675, 100.0000000000000711 ) ;
#29490 = CARTESIAN_POINT ( 'NONE',  ( 42.30527206516848082, 31.00000000000000355, -85.53883208674149330 ) ) ;
#29491 = ORIENTED_EDGE ( 'NONE', *, *, #36502, .F. ) ;
#29492 = CARTESIAN_POINT ( 'NONE',  ( 17.99999999999999645, 0.000000000000000000, 0.000000000000000000 ) ) ;
#29493 = CARTESIAN_POINT ( 'NONE',  ( 17.99999999999999645, -83.49789599728724454, -86.88263557826851979 ) ) ;
#29494 = CARTESIAN_POINT ( 'NONE',  ( 17.99999999999999645, 100.8494052988179561, -65.95368414178808791 ) ) ;
#29495 = ORIENTED_EDGE ( 'NONE', *, *, #22622, .T. ) ;
#29496 = DIRECTION ( 'NONE',  ( 0.000000000000000000, 0.000000000000000000, 1.000000000000000000 ) ) ;
#29497 = EDGE_CURVE ( 'NONE', #37944, #2980, #6173, .T. ) ;
#29498 = CARTESIAN_POINT ( 'NONE',  ( -6.075999999999997847, 0.000000000000000000, 0.000000000000000000 ) ) ;
#29500 = FACE_OUTER_BOUND ( 'NONE', #18033, .T. ) ;
#29499 = CARTESIAN_POINT ( 'NONE',  ( -2.797566391619251075E-15, 1.860994515641065082E-14, 7.000000000000002665 ) ) ;
#29501 = AXIS2_PLACEMENT_3D ( 'NONE', #21977, #2478, #29148 ) ;
#29502 = CYLINDRICAL_SURFACE ( 'NONE', #36038, 116.0000000000000000 ) ;
#29503 = EDGE_LOOP ( 'NONE', ( #26305, #17714, #16025, #9676 ) ) ;
#29504 = EDGE_CURVE ( 'NONE', #38227, #17128, #19521, .T. ) ;
#29505 = VECTOR ( 'NONE', #9815, 1000.000000000000000 ) ;
#29506 = CARTESIAN_POINT ( 'NONE',  ( -17.40445659762299968, 31.00000000000000355, 22.69748452323785060 ) ) ;
#29507 = ORIENTED_EDGE ( 'NONE', *, *, #3562, .T. ) ;
#29508 = DIRECTION ( 'NONE',  ( 3.009274222672345096E-17, 1.000000000000000000, -2.455023325076454960E-18 ) ) ;
#29509 = EDGE_CURVE ( 'NONE', #30609, #24319, #38149, .T. ) ;
#29510 = CYLINDRICAL_SURFACE ( 'NONE', #26048, 116.0000000000000000 ) ;
#29511 = ORIENTED_EDGE ( 'NONE', *, *, #31620, .F. ) ;
#29512 = DIRECTION ( 'NONE',  ( 0.000000000000000000, 0.8443279255020126328, 0.5358267949790005424 ) ) ;
#29513 = CARTESIAN_POINT ( 'NONE',  ( -33.98628324864968420, 40.00000000000000000, 19.63407011443918293 ) ) ;
#29514 = CARTESIAN_POINT ( 'NONE',  ( 17.75583184595346964, 40.00000000000000000, -30.63479189996225216 ) ) ;
#29515 = VERTEX_POINT ( 'NONE', #5950 ) ;
#29516 = EDGE_LOOP ( 'NONE', ( #40088, #8887, #28447, #17677 ) ) ;
#29517 = DIRECTION ( 'NONE',  ( 0.000000000000000000, 0.000000000000000000, -1.000000000000000000 ) ) ;
#29518 = DIRECTION ( 'NONE',  ( 1.000000000000000000, 0.000000000000000000, 0.000000000000000000 ) ) ;
#29519 = ADVANCED_FACE ( 'NONE', ( #29528 ), #32363, .T. ) ;
#29520 = CYLINDRICAL_SURFACE ( 'NONE', #30990, 120.5010000000000190 ) ;
#29521 = AXIS2_PLACEMENT_3D ( 'NONE', #19965, #15818, #9030 ) ;
#29522 = DIRECTION ( 'NONE',  ( 0.000000000000000000, 0.000000000000000000, 1.000000000000000000 ) ) ;
#29523 = DIRECTION ( 'NONE',  ( -1.000000000000000000, 0.000000000000000000, -0.000000000000000000 ) ) ;
#29524 = ORIENTED_EDGE ( 'NONE', *, *, #28742, .F. ) ;
#29525 = DIRECTION ( 'NONE',  ( 1.000000000000000000, 0.000000000000000000, 0.000000000000000000 ) ) ;
#29526 = EDGE_LOOP ( 'NONE', ( #16287, #29437, #592, #5909 ) ) ;
#29527 = CARTESIAN_POINT ( 'NONE',  ( 0.000000000000000000, 46.87740477351712798, 3.172455868806036694 ) ) ;
#29528 = FACE_OUTER_BOUND ( 'NONE', #2714, .T. ) ;
#29529 =( REPRESENTATION_RELATIONSHIP ('NONE','NONE', #330, #18009 ) REPRESENTATION_RELATIONSHIP_WITH_TRANSFORMATION ( #14395 )SHAPE_REPRESENTATION_RELATIONSHIP( ) );
#29530 = EDGE_CURVE ( 'NONE', #21935, #3796, #32581, .T. ) ;
#29531 = ADVANCED_FACE ( 'NONE', ( #25647, #38905 ), #9023, .T. ) ;
#29532 = CARTESIAN_POINT ( 'NONE',  ( 18.00000000000000355, -11.90021268425586953, 45.45261810511210143 ) ) ;
#29533 = EDGE_CURVE ( 'NONE', #7030, #43001, #29829, .T. ) ;
#29534 = EDGE_CURVE ( 'NONE', #3223, #7181, #30820, .T. ) ;
#29535 = CIRCLE ( 'NONE', #24705, 59.00000000000001421 ) ;
#29536 = DIRECTION ( 'NONE',  ( 0.000000000000000000, -0.05322217484216513333, -0.9985826956767627216 ) ) ;
#29537 = ORIENTED_EDGE ( 'NONE', *, *, #12324, .F. ) ;
#29538 = DIRECTION ( 'NONE',  ( 0.000000000000000000, 0.000000000000000000, 1.000000000000000000 ) ) ;
#29539 = ORIENTED_EDGE ( 'NONE', *, *, #13196, .F. ) ;
#29540 = CYLINDRICAL_SURFACE ( 'NONE', #27443, 13.60000000000000142 ) ;
#29541 = CIRCLE ( 'NONE', #3704, 59.00000000000000711 ) ;
#29542 = VERTEX_POINT ( 'NONE', #30613 ) ;
#29544 = EDGE_LOOP ( 'NONE', ( #38384, #13286, #37419, #39617 ) ) ;
#29543 = LINE ( 'NONE', #25657, #37570 ) ;
#29545 = CARTESIAN_POINT ( 'NONE',  ( 63.11376326756305843, 31.00000000000000000, -21.32174659671377626 ) ) ;
#29546 = ORIENTED_EDGE ( 'NONE', *, *, #10010, .F. ) ;
#29547 = DIRECTION ( 'NONE',  ( -1.000000000000000000, -0.000000000000000000, 0.000000000000000000 ) ) ;
#29548 = AXIS2_PLACEMENT_3D ( 'NONE', #26020, #39283, #9418 ) ;
#29549 = ORIENTED_EDGE ( 'NONE', *, *, #36715, .F. ) ;
#29550 = CARTESIAN_POINT ( 'NONE',  ( 42.80287614962723808, -35.35525454449572180, 69.29271901957299917 ) ) ;
#29551 = EDGE_LOOP ( 'NONE', ( #42422, #22167, #13906, #13979 ) ) ;
#29553 = CARTESIAN_POINT ( 'NONE',  ( -79.74759331938361129, 40.00000000000000711, -21.47736420602193874 ) ) ;
#29552 = AXIS2_PLACEMENT_3D ( 'NONE', #31344, #34161, #1426 ) ;
#29555 = CARTESIAN_POINT ( 'NONE',  ( 17.99999999999999645, -109.4038418350907023, 50.51029986767514401 ) ) ;
#29554 = DIRECTION ( 'NONE',  ( -1.000000000000000000, -0.000000000000000000, -0.000000000000000000 ) ) ;
#29556 = CARTESIAN_POINT ( 'NONE',  ( 0.000000000000000000, -44.61570720899106846, 14.73072383765551940 ) ) ;
#29557 = ORIENTED_EDGE ( 'NONE', *, *, #6683, .F. ) ;
#29558 = DIRECTION ( 'NONE',  ( -3.009274222672345096E-17, -1.000000000000000000, 2.455023325076454960E-18 ) ) ;
#29559 = AXIS2_PLACEMENT_3D ( 'NONE', #23339, #36601, #6723 ) ;
#29560 = VERTEX_POINT ( 'NONE', #27335 ) ;
#29561 =( NAMED_UNIT ( * ) SI_UNIT ( $, .STERADIAN. ) SOLID_ANGLE_UNIT ( ) );
#29562 = CARTESIAN_POINT ( 'NONE',  ( 0.000000000000000000, -101.1249659627859216, 48.60055280209385842 ) ) ;
#29563 = AXIS2_PLACEMENT_3D ( 'NONE', #40226, #23484, #17152 ) ;
#29564 = CARTESIAN_POINT ( 'NONE',  ( 17.99999999999999645, 109.3506818544115617, -38.70953859160899668 ) ) ;
#29565 = CARTESIAN_POINT ( 'NONE',  ( 72.19657831791809599, 31.00000000000000000, -19.34484491892447622 ) ) ;
#29566 = EDGE_CURVE ( 'NONE', #9805, #12272, #30508, .T. ) ;
#29568 = DIRECTION ( 'NONE',  ( -1.000000000000000000, -0.000000000000000000, -0.000000000000000000 ) ) ;
#29567 = DIRECTION ( 'NONE',  ( 0.000000000000000000, 0.000000000000000000, 1.000000000000000000 ) ) ;
#29569 = ORIENTED_EDGE ( 'NONE', *, *, #10007, .F. ) ;
#29570 = VECTOR ( 'NONE', #31831, 1000.000000000000114 ) ;
#29571 =( NAMED_UNIT ( * ) PLANE_ANGLE_UNIT ( ) SI_UNIT ( $, .RADIAN. ) );
#29572 = AXIS2_PLACEMENT_3D ( 'NONE', #8282, #14849, #27723 ) ;
#29573 = VERTEX_POINT ( 'NONE', #233 ) ;
#29574 = LINE ( 'NONE', #42842, #15072 ) ;
#29575 = CYLINDRICAL_SURFACE ( 'NONE', #35272, 20.00000000000000355 ) ;
#29576 = CARTESIAN_POINT ( 'NONE',  ( -86.84058463553202500, 31.00000000000000711, 29.36381822872188607 ) ) ;
#29577 = CARTESIAN_POINT ( 'NONE',  ( -46.83686391397709770, 40.00000000000000000, -81.34213072392142863 ) ) ;
#29578 = DIRECTION ( 'NONE',  ( -1.000000000000000000, -0.000000000000000000, -0.000000000000000000 ) ) ;
#29579 = FACE_OUTER_BOUND ( 'NONE', #29014, .T. ) ;
#29580 = VERTEX_POINT ( 'NONE', #896 ) ;
#29581 = DIRECTION ( 'NONE',  ( 1.058513553088275437E-16, 1.000000000000000000, -8.813324511995299047E-17 ) ) ;
#29582 = ORIENTED_EDGE ( 'NONE', *, *, #10424, .F. ) ;
#29583 = AXIS2_PLACEMENT_3D ( 'NONE', #11605, #5249, #21879 ) ;
#29584 = LINE ( 'NONE', #42858, #19312 ) ;
#29585 = DIRECTION ( 'NONE',  ( -1.000000000000000000, -0.000000000000000000, -0.000000000000000000 ) ) ;
#29586 = EDGE_CURVE ( 'NONE', #4825, #12961, #24275, .T. ) ;
#29587 = EDGE_CURVE ( 'NONE', #11136, #18380, #37346, .T. ) ;
#29588 = DIRECTION ( 'NONE',  ( -1.000000000000000000, 0.000000000000000000, 0.000000000000000000 ) ) ;
#29589 = ORIENTED_EDGE ( 'NONE', *, *, #34123, .T. ) ;
#29590 = CARTESIAN_POINT ( 'NONE',  ( 0.000000000000000000, -3.840921266749489860, -47.34345070675173872 ) ) ;
#29591 = CIRCLE ( 'NONE', #37228, 4.500000000000002665 ) ;
#29592 = LINE ( 'NONE', #29383, #4661 ) ;
#29593 = EDGE_CURVE ( 'NONE', #21090, #5484, #11017, .T. ) ;
#29594 = CYLINDRICAL_SURFACE ( 'NONE', #41719, 59.00000000000000000 ) ;
#29596 = ORIENTED_EDGE ( 'NONE', *, *, #2741, .T. ) ;
#29595 = LINE ( 'NONE', #9729, #15960 ) ;
#29597 = CARTESIAN_POINT ( 'NONE',  ( -1.240299975428113101E-15, -4.647091401871173311, -3.572172305156514849 ) ) ;
#29598 = CARTESIAN_POINT ( 'NONE',  ( 18.00000000000000355, -50.95304419620816105, -10.38206564895716610 ) ) ;
#29599 = VECTOR ( 'NONE', #21181, 1000.000000000000000 ) ;
#29601 = ORIENTED_EDGE ( 'NONE', *, *, #11472, .F. ) ;
#29600 = FACE_OUTER_BOUND ( 'NONE', #13716, .T. ) ;
#29602 = UNCERTAINTY_MEASURE_WITH_UNIT (LENGTH_MEASURE( 1.000000000000000082E-05 ), #26675, 'distance_accuracy_value', 'NONE');
#29603 = CIRCLE ( 'NONE', #40717, 120.5010000000000190 ) ;
#29604 = VERTEX_POINT ( 'NONE', #3722 ) ;
#29605 = FACE_OUTER_BOUND ( 'NONE', #27553, .T. ) ;
#29606 = FACE_OUTER_BOUND ( 'NONE', #26059, .T. ) ;
#29607 = CARTESIAN_POINT ( 'NONE',  ( -21.81649963859176822, 40.00000000000000000, -37.93159502954524243 ) ) ;
#29608 = FACE_OUTER_BOUND ( 'NONE', #4119, .T. ) ;
#29609 = EDGE_CURVE ( 'NONE', #30056, #37428, #36045, .T. ) ;
#29610 = DIRECTION ( 'NONE',  ( 0.000000000000000000, -0.9996456111234528485, 0.02662052143776447166 ) ) ;
#29611 = DIRECTION ( 'NONE',  ( 0.000000000000000000, 0.000000000000000000, 1.000000000000000000 ) ) ;
#29612 = ORIENTED_EDGE ( 'NONE', *, *, #25146, .F. ) ;
#29613 = VERTEX_POINT ( 'NONE', #805 ) ;
#29614 = DIRECTION ( 'NONE',  ( -1.000000000000000000, 0.000000000000000000, 0.000000000000000000 ) ) ;
#29615 = CIRCLE ( 'NONE', #28230, 116.0000000000000000 ) ;
#29616 = ORIENTED_EDGE ( 'NONE', *, *, #1170, .T. ) ;
#29617 = CARTESIAN_POINT ( 'NONE',  ( 17.99999999999999645, 112.1702510623870381, -2.471285140322999840 ) ) ;
#29618 = CARTESIAN_POINT ( 'NONE',  ( 17.99999999999999645, -84.62908780824814414, -85.78116633471378805 ) ) ;
#29619 = CARTESIAN_POINT ( 'NONE',  ( 43.15607885788778475, 31.00000000000000355, -11.56636786368396486 ) ) ;
#29620 = DIRECTION ( 'NONE',  ( 0.000000000000000000, -0.9407002666710297945, -0.3392388661180402165 ) ) ;
#29621 = VERTEX_POINT ( 'NONE', #13832 ) ;
#29622 = VECTOR ( 'NONE', #6988, 1000.000000000000000 ) ;
#29623 = CIRCLE ( 'NONE', #10808, 2.500000000000000888 ) ;
#29624 = AXIS2_PLACEMENT_3D ( 'NONE', #23992, #40731, #30303 ) ;
#29625 = CARTESIAN_POINT ( 'NONE',  ( 17.99999999999999645, 88.56657216608705596, -68.87840567545838155 ) ) ;
#29626 = CARTESIAN_POINT ( 'NONE',  ( 28.03234818517180216, 31.00000000000000355, 82.53419278363811884 ) ) ;
#29627 = CIRCLE ( 'NONE', #17130, 1.999999999999998668 ) ;
#29628 = DIRECTION ( 'NONE',  ( 0.000000000000000000, 0.000000000000000000, 1.000000000000000000 ) ) ;
#29629 = ORIENTED_EDGE ( 'NONE', *, *, #8110, .F. ) ;
#29630 = CARTESIAN_POINT ( 'NONE',  ( 64.47787635702036368, 31.00000000000000000, -17.16423577041365789 ) ) ;
#29632 = VECTOR ( 'NONE', #21576, 1000.000000000000000 ) ;
#29631 = CARTESIAN_POINT ( 'NONE',  ( -8.314562429032193336, 40.00000000000000000, -63.88718494337742015 ) ) ;
#29633 = CARTESIAN_POINT ( 'NONE',  ( -86.05617919112455638, 40.00000000000000711, 49.70311056393224192 ) ) ;
#29634 = VECTOR ( 'NONE', #30027, 1000.000000000000000 ) ;
#29635 = EDGE_LOOP ( 'NONE', ( #7727, #42454 ) ) ;
#29636 = DIRECTION ( 'NONE',  ( 0.000000000000000000, -0.9911528310040056411, -0.1327255272837324085 ) ) ;
#29637 = CARTESIAN_POINT ( 'NONE',  ( 17.99999999999999645, -34.74871106919691499, 106.6808302961370600 ) ) ;
#29638 = CARTESIAN_POINT ( 'NONE',  ( 17.99999999999999645, 58.30069736313799211, -100.2847380560561419 ) ) ;
#29640 = ORIENTED_EDGE ( 'NONE', *, *, #2174, .F. ) ;
#29639 = LINE ( 'NONE', #9770, #1817 ) ;
#29641 = EDGE_CURVE ( 'NONE', #4444, #8807, #10085, .T. ) ;
#29642 = DIRECTION ( 'NONE',  ( -1.000000000000000000, -0.000000000000000000, -0.000000000000000000 ) ) ;
#29643 = VERTEX_POINT ( 'NONE', #14247 ) ;
#29644 = CARTESIAN_POINT ( 'NONE',  ( 4.197393957002303999, 0.8151795401431359833, -3.503767560748935139 ) ) ;
#29645 = CARTESIAN_POINT ( 'NONE',  ( -47.90394619311608437, 40.00000000000000000, 62.45286580340285099 ) ) ;
#29646 = LINE ( 'NONE', #39648, #31957 ) ;
#29647 = VECTOR ( 'NONE', #22352, 1000.000000000000000 ) ;
#29648 = ORIENTED_EDGE ( 'NONE', *, *, #5293, .F. ) ;
#29649 = CARTESIAN_POINT ( 'NONE',  ( 17.99999999999999645, -117.9424311864590891, 24.69967462998996766 ) ) ;
#29650 = CARTESIAN_POINT ( 'NONE',  ( 17.99999999999999645, -117.6086855750632765, -26.24286718912224003 ) ) ;
#29651 = AXIS2_PLACEMENT_3D ( 'NONE', #15218, #38073, #21768 ) ;
#29652 = EDGE_CURVE ( 'NONE', #8193, #18529, #3299, .T. ) ;
#29653 = ORIENTED_EDGE ( 'NONE', *, *, #3740, .T. ) ;
#29654 = CIRCLE ( 'NONE', #331, 120.5010000000000048 ) ;
#29655 = AXIS2_PLACEMENT_3D ( 'NONE', #8507, #42077, #41671 ) ;
#29656 = EDGE_CURVE ( 'NONE', #36478, #6009, #27552, .T. ) ;
#29657 = AXIS2_PLACEMENT_3D ( 'NONE', #18407, #1768, #18631 ) ;
#29658 = ORIENTED_EDGE ( 'NONE', *, *, #43155, .F. ) ;
#29659 = DIRECTION ( 'NONE',  ( 0.000000000000000000, -1.000000000000000000, 1.287488025362403787E-15 ) ) ;
#29660 = EDGE_LOOP ( 'NONE', ( #22158, #31327, #21057, #30189 ) ) ;
#29661 = AXIS2_PLACEMENT_3D ( 'NONE', #7711, #13865, #26934 ) ;
#29662 = CYLINDRICAL_SURFACE ( 'NONE', #22391, 51.99999999999999289 ) ;
#29663 = CARTESIAN_POINT ( 'NONE',  ( 18.00000000000000355, -5.667686777402029641, 46.64153600743603789 ) ) ;
#29664 = EDGE_CURVE ( 'NONE', #36583, #40692, #35375, .T. ) ;
#29665 = AXIS2_PLACEMENT_3D ( 'NONE', #34337, #14520, #11887 ) ;
#29666 = CARTESIAN_POINT ( 'NONE',  ( 150.5000000000000284, 1.576403824487674918E-12, 6.999999999999998224 ) ) ;
#29667 = FACE_OUTER_BOUND ( 'NONE', #21047, .T. ) ;
#29668 = ORIENTED_EDGE ( 'NONE', *, *, #21562, .T. ) ;
#29669 = FACE_OUTER_BOUND ( 'NONE', #35897, .T. ) ;
#29671 = VERTEX_POINT ( 'NONE', #19952 ) ;
#29670 = AXIS2_PLACEMENT_3D ( 'NONE', #34998, #12536, #9238 ) ;
#29672 = DIRECTION ( 'NONE',  ( -1.000000000000000000, 0.000000000000000000, 0.000000000000000000 ) ) ;
#29673 = ORIENTED_EDGE ( 'NONE', *, *, #15315, .T. ) ;
#29674 = CARTESIAN_POINT ( 'NONE',  ( 17.99999999999999645, 109.4038418350910433, -50.51029986767441926 ) ) ;
#29675 = DIRECTION ( 'NONE',  ( -1.000000000000000000, 0.000000000000000000, 0.000000000000000000 ) ) ;
#29676 = ITEM_DEFINED_TRANSFORMATION ( 'NONE', 'NONE', #10727,  #13552 ) ;
#29677 = CARTESIAN_POINT ( 'NONE',  ( 0.000000000000000000, 87.92975456462995965, -69.68953103478068556 ) ) ;
#29678 = CARTESIAN_POINT ( 'NONE',  ( -29.22812062908682051, 31.00000000000000355, 50.62729764625685647 ) ) ;
#29679 = EDGE_CURVE ( 'NONE', #27833, #14651, #17338, .T. ) ;
#29681 = VERTEX_POINT ( 'NONE', #20174 ) ;
#29680 = AXIS2_PLACEMENT_3D ( 'NONE', #26072, #19982, #9694 ) ;
#29682 = CARTESIAN_POINT ( 'NONE',  ( -2.659806967433831382, 31.00000000000000355, 39.59793253467758944 ) ) ;
#29683 = CARTESIAN_POINT ( 'NONE',  ( -4.745113895469965648, 40.00000000000000000, -72.39583333427917466 ) ) ;
#29684 = AXIS2_PLACEMENT_3D ( 'NONE', #17676, #10656, #18123 ) ;
#29685 = AXIS2_PLACEMENT_3D ( 'NONE', #20921, #41579, #35035 ) ;
#29686 = VECTOR ( 'NONE', #31721, 1000.000000000000000 ) ;
#29687 = DIRECTION ( 'NONE',  ( 0.000000000000000000, 0.000000000000000000, 1.000000000000000000 ) ) ;
#29688 = CARTESIAN_POINT ( 'NONE',  ( 17.99999999999999645, 103.1672962317657323, -44.09967643725766351 ) ) ;
#29689 = VECTOR ( 'NONE', #39923, 1000.000000000000000 ) ;
#29690 = CYLINDRICAL_SURFACE ( 'NONE', #11425, 120.5010000000000190 ) ;
#29691 = DIRECTION ( 'NONE',  ( -0.000000000000000000, -0.000000000000000000, 1.000000000000000000 ) ) ;
#29692 = AXIS2_PLACEMENT_3D ( 'NONE', #37995, #24744, #8119 ) ;
#29694 = ORIENTED_EDGE ( 'NONE', *, *, #38804, .F. ) ;
#29693 = ADVANCED_BREP_SHAPE_REPRESENTATION ( '', ( #112, #13552 ), #2321 ) ;
#29695 = CARTESIAN_POINT ( 'NONE',  ( -18.51709390187839688, 40.00000000000000000, -37.54239277154294996 ) ) ;
#29696 = DIRECTION ( 'NONE',  ( -1.000000000000000000, 0.000000000000000000, 0.000000000000000000 ) ) ;
#29697 = DIRECTION ( 'NONE',  ( 1.000000000000000000, 0.000000000000000000, 0.000000000000000000 ) ) ;
#29698 = ORIENTED_EDGE ( 'NONE', *, *, #28401, .F. ) ;
#29699 = DIRECTION ( 'NONE',  ( 1.000000000000000000, 0.000000000000000000, 0.000000000000000000 ) ) ;
#29700 = CARTESIAN_POINT ( 'NONE',  ( -6.199999999999997513, 4.693303851024319376E-15, 0.000000000000000000 ) ) ;
#29701 = ORIENTED_EDGE ( 'NONE', *, *, #7894, .F. ) ;
#29702 = CARTESIAN_POINT ( 'NONE',  ( 18.00000000000000355, -11.90021268425522827, -45.45261810511227907 ) ) ;
#29703 = ORIENTED_EDGE ( 'NONE', *, *, #27929, .F. ) ;
#29704 = ADVANCED_FACE ( 'NONE', ( #7465 ), #24082, .F. ) ;
#29705 = ORIENTED_EDGE ( 'NONE', *, *, #32051, .F. ) ;
#29706 = DIRECTION ( 'NONE',  ( -0.000000000000000000, 0.8660254037844392627, 0.4999999999999990008 ) ) ;
#29707 = CARTESIAN_POINT ( 'NONE',  ( -68.52217190868857699, 31.00000000000000711, 59.94826526066079708 ) ) ;
#29708 = VERTEX_POINT ( 'NONE', #21 ) ;
#29709 = DIRECTION ( 'NONE',  ( -1.000000000000000000, -0.000000000000000000, 0.000000000000000000 ) ) ;
#29710 = AXIS2_PLACEMENT_3D ( 'NONE', #5308, #14942, #15164 ) ;
#29711 = CYLINDRICAL_SURFACE ( 'NONE', #21314, 2.649999999999985700 ) ;
#29712 = VECTOR ( 'NONE', #21709, 1000.000000000000000 ) ;
#29714 = FACE_OUTER_BOUND ( 'NONE', #39880, .T. ) ;
#29713 = AXIS2_PLACEMENT_3D ( 'NONE', #3388, #3162, #29611 ) ;
#29715 = ORIENTED_EDGE ( 'NONE', *, *, #16874, .F. ) ;
#29716 = VECTOR ( 'NONE', #36959, 1000.000000000000000 ) ;
#29717 = CARTESIAN_POINT ( 'NONE',  ( 17.99999999999999645, -2.418575551221673336, 120.4767259403368911 ) ) ;
#29718 = VECTOR ( 'NONE', #19295, 1000.000000000000000 ) ;
#29719 = FACE_OUTER_BOUND ( 'NONE', #9126, .T. ) ;
#29720 = CIRCLE ( 'NONE', #1830, 116.0000000000000000 ) ;
#29722 = CARTESIAN_POINT ( 'NONE',  ( 17.99999999999999645, 0.000000000000000000, 0.000000000000000000 ) ) ;
#29721 = CARTESIAN_POINT ( 'NONE',  ( 17.99999999999999645, 88.00363688980546328, 82.31555682352686176 ) ) ;
#29723 = VECTOR ( 'NONE', #4544, 1000.000000000000000 ) ;
#29724 = CARTESIAN_POINT ( 'NONE',  ( -10.00000000000000000, 0.000000000000000000, 0.000000000000000000 ) ) ;
#29725 = ORIENTED_EDGE ( 'NONE', *, *, #12637, .T. ) ;
#29726 =( NAMED_UNIT ( * ) PLANE_ANGLE_UNIT ( ) SI_UNIT ( $, .RADIAN. ) );
#29727 = AXIS2_PLACEMENT_3D ( 'NONE', #21155, #15258, #11304 ) ;
#29728 = CARTESIAN_POINT ( 'NONE',  ( -1.799870782497340782, 31.00000000000000355, 27.60416666422008802 ) ) ;
#29729 = EDGE_CURVE ( 'NONE', #4036, #27564, #37738, .T. ) ;
#29730 = ORIENTED_EDGE ( 'NONE', *, *, #37959, .T. ) ;
#29731 = CARTESIAN_POINT ( 'NONE',  ( 17.99999999999999645, 114.8812324315177023, -16.07179003769037351 ) ) ;
#29732 = ADVANCED_FACE ( 'NONE', ( #26901 ), #16895, .T. ) ;
#29733 = CARTESIAN_POINT ( 'NONE',  ( -132.0000507999999968, 1.347111479062088405E-15, 11.00000000000000000 ) ) ;
#29734 = ORIENTED_EDGE ( 'NONE', *, *, #16759, .F. ) ;
#29735 = AXIS2_PLACEMENT_3D ( 'NONE', #36951, #26718, #30006 ) ;
#29736 = CARTESIAN_POINT ( 'NONE',  ( 17.99999999999999645, -113.8630351447207119, 22.16324045874372572 ) ) ;
#29737 = CARTESIAN_POINT ( 'NONE',  ( -10.91816144241376563, 40.00000000000000000, -40.73603723627661566 ) ) ;
#29738 = CARTESIAN_POINT ( 'NONE',  ( 45.06603723658675875, 40.00000000000000000, 15.38899812202754624 ) ) ;
#29739 = ORIENTED_EDGE ( 'NONE', *, *, #17193, .F. ) ;
#29740 = ORIENTED_EDGE ( 'NONE', *, *, #25288, .T. ) ;
#29741 = DIRECTION ( 'NONE',  ( 0.000000000000000000, -0.05322217484218559613, 0.9985826956767616114 ) ) ;
#29742 = CYLINDRICAL_SURFACE ( 'NONE', #21475, 116.0000000000000000 ) ;
#29743 = AXIS2_PLACEMENT_3D ( 'NONE', #37460, #3625, #30509 ) ;
#29744 = DIRECTION ( 'NONE',  ( 1.000000000000000000, -3.469446951953614189E-17, 0.000000000000000000 ) ) ;
#29745 = AXIS2_PLACEMENT_3D ( 'NONE', #23941, #16967, #316 ) ;
#29746 = DIRECTION ( 'NONE',  ( -1.000000000000000000, -0.000000000000000000, -0.000000000000000000 ) ) ;
#29747 = VECTOR ( 'NONE', #39527, 1000.000000000000000 ) ;
#29748 = DIRECTION ( 'NONE',  ( 0.000000000000000000, 0.8993121301712202476, -0.4373073204588531770 ) ) ;
#29749 = VERTEX_POINT ( 'NONE', #17107 ) ;
#29750 = LINE ( 'NONE', #29318, #36109 ) ;
#29751 = VERTEX_POINT ( 'NONE', #24524 ) ;
#29752 = DIRECTION ( 'NONE',  ( 0.000000000000000000, -1.000000000000000000, 5.297542245118643184E-16 ) ) ;
#29753 = CARTESIAN_POINT ( 'NONE',  ( 17.99999999999999645, -79.18387647320706435, -84.76976882518842160 ) ) ;
#29754 = CIRCLE ( 'NONE', #28403, 36.00000000000000000 ) ;
#29755 = ORIENTED_EDGE ( 'NONE', *, *, #10282, .F. ) ;
#29756 = VECTOR ( 'NONE', #30919, 1000.000000000000000 ) ;
#29757 = DIRECTION ( 'NONE',  ( -1.000000000000000000, 0.000000000000000000, -0.000000000000000000 ) ) ;
#29758 = CARTESIAN_POINT ( 'NONE',  ( 17.99999999999999645, 95.38615066514064722, -59.07414607872728141 ) ) ;
#29759 = ORIENTED_EDGE ( 'NONE', *, *, #8968, .T. ) ;
#29760 = FACE_OUTER_BOUND ( 'NONE', #37484, .T. ) ;
#29761 = ORIENTED_EDGE ( 'NONE', *, *, #34293, .T. ) ;
#29762 = DIRECTION ( 'NONE',  ( -1.000000000000000000, 0.000000000000000000, -0.000000000000000000 ) ) ;
#29763 = AXIS2_PLACEMENT_3D ( 'NONE', #12451, #28394, #22497 ) ;
#29764 = ADVANCED_FACE ( 'NONE', ( #31901 ), #8115, .T. ) ;
#29765 = ORIENTED_EDGE ( 'NONE', *, *, #8356, .T. ) ;
#29767 = ORIENTED_EDGE ( 'NONE', *, *, #39782, .F. ) ;
#29766 = DIRECTION ( 'NONE',  ( 0.000000000000000000, 0.000000000000000000, 1.000000000000000000 ) ) ;
#29768 = CARTESIAN_POINT ( 'NONE',  ( 66.90003082756123831, 31.00000000000000000, -4.275635516647131595 ) ) ;
#29769 = EDGE_CURVE ( 'NONE', #1690, #13634, #40937, .T. ) ;
#29770 = ORIENTED_EDGE ( 'NONE', *, *, #1546, .F. ) ;
#29771 = CARTESIAN_POINT ( 'NONE',  ( -4.000000000000000000, 2.309401076758498483, -5.000000000000000000 ) ) ;
#29772 = ADVANCED_FACE ( 'NONE', ( #7893 ), #16587, .F. ) ;
#29773 = ORIENTED_EDGE ( 'NONE', *, *, #6483, .F. ) ;
#29774 = DIRECTION ( 'NONE',  ( 0.000000000000000000, 0.7980172272802363853, 0.6026346363792605132 ) ) ;
#29775 = PRODUCT_DEFINITION_SHAPE ( 'NONE', 'NONE',  #43203 ) ;
#29776 = ORIENTED_EDGE ( 'NONE', *, *, #10844, .F. ) ;
#29777 = CARTESIAN_POINT ( 'NONE',  ( 76.16439905403352384, 39.99999999999999289, 44.11546174421767574 ) ) ;
#29779 = DIRECTION ( 'NONE',  ( -1.000000000000000000, -0.000000000000000000, -0.000000000000000000 ) ) ;
#29778 = DIRECTION ( 'NONE',  ( -1.000000000000000000, -0.000000000000000000, -0.000000000000000000 ) ) ;
#29780 = CARTESIAN_POINT ( 'NONE',  ( -2.841217984690893843E-16, 1.478917074864463474E-14, 1.999999999999980904 ) ) ;
#29781 = ORIENTED_EDGE ( 'NONE', *, *, #3078, .F. ) ;
#29782 = DIRECTION ( 'NONE',  ( 0.000000000000000000, 0.000000000000000000, 1.000000000000000000 ) ) ;
#29783 = CIRCLE ( 'NONE', #39518, 2.500000000000000444 ) ;
#29784 = ORIENTED_EDGE ( 'NONE', *, *, #104, .T. ) ;
#29785 = AXIS2_PLACEMENT_3D ( 'NONE', #10750, #30399, #1350 ) ;
#29786 = SURFACE_STYLE_USAGE ( .BOTH. , #53 ) ;
#29787 = CIRCLE ( 'NONE', #15215, 116.0000000000000000 ) ;
#29788 = CARTESIAN_POINT ( 'NONE',  ( 17.99999999999999645, 0.000000000000000000, 0.000000000000000000 ) ) ;
#29789 = LINE ( 'NONE', #13209, #31695 ) ;
#29790 = CIRCLE ( 'NONE', #25634, 58.99999999999999289 ) ;
#29791 = EDGE_CURVE ( 'NONE', #16, #31395, #1121, .T. ) ;
#29792 = CARTESIAN_POINT ( 'NONE',  ( -61.13902149641835138, 31.00000000000000355, -53.61851653479526902 ) ) ;
#29793 = ADVANCED_FACE ( 'NONE', ( #1986 ), #24735, .T. ) ;
#29795 = DIRECTION ( 'NONE',  ( -1.000000000000000000, -0.000000000000000000, -0.000000000000000000 ) ) ;
#29794 = DIRECTION ( 'NONE',  ( 0.000000000000000000, -0.8951632913550571224, -0.4457383557765488002 ) ) ;
#29797 = VERTEX_POINT ( 'NONE', #21255 ) ;
#29796 = AXIS2_PLACEMENT_3D ( 'NONE', #21535, #28491, #4441 ) ;
#29798 = ADVANCED_FACE ( 'NONE', ( #10977 ), #18637, .F. ) ;
#29799 = ADVANCED_FACE ( 'NONE', ( #27999 ), #5054, .T. ) ;
#29800 = VECTOR ( 'NONE', #10723, 1000.000000000000000 ) ;
#29801 = CARTESIAN_POINT ( 'NONE',  ( 17.99999999999999645, 0.000000000000000000, 0.000000000000000000 ) ) ;
#29802 = CIRCLE ( 'NONE', #42286, 59.00000000000000000 ) ;
#29803 = ORIENTED_EDGE ( 'NONE', *, *, #10997, .T. ) ;
#29804 = DIRECTION ( 'NONE',  ( -1.000000000000000000, 0.000000000000000000, 0.000000000000000000 ) ) ;
#29805 = DIRECTION ( 'NONE',  ( -1.000000000000000000, 0.000000000000000000, 0.000000000000000000 ) ) ;
#29806 = CARTESIAN_POINT ( 'NONE',  ( -61.59955500562279695, 31.00000000000000711, -70.40623950599746195 ) ) ;
#29807 = DIRECTION ( 'NONE',  ( 1.000000000000000000, 0.000000000000000000, 0.000000000000000000 ) ) ;
#29808 = CARTESIAN_POINT ( 'NONE',  ( 2.500000000000000000, -1.178949249685214307, 2.042000000000001592 ) ) ;
#29809 = ORIENTED_EDGE ( 'NONE', *, *, #15966, .F. ) ;
#29810 = DIRECTION ( 'NONE',  ( 0.000000000000000000, 0.000000000000000000, 1.000000000000000000 ) ) ;
#29811 = ORIENTED_EDGE ( 'NONE', *, *, #24118, .T. ) ;
#29812 = CARTESIAN_POINT ( 'NONE',  ( -9.000000000000005329, 1.832071611524440088E-15, -14.91999999999999815 ) ) ;
#29813 = AXIS2_PLACEMENT_3D ( 'NONE', #33229, #29757, #472 ) ;
#29814 = DIRECTION ( 'NONE',  ( 0.000000000000000000, -0.9618256431728160472, -0.2736629900720938813 ) ) ;
#29815 = LINE ( 'NONE', #17164, #2397 ) ;
#29816 = ORIENTED_EDGE ( 'NONE', *, *, #3282, .F. ) ;
#29817 = DIRECTION ( 'NONE',  ( -1.000000000000000000, 0.000000000000000000, 0.000000000000000000 ) ) ;
#29818 = AXIS2_PLACEMENT_3D ( 'NONE', #16837, #29916, #23367 ) ;
#29819 = CARTESIAN_POINT ( 'NONE',  ( 0.000000000000000000, 0.000000000000000000, 0.000000000000000000 ) ) ;
#29820 = VECTOR ( 'NONE', #41657, 1000.000000000000000 ) ;
#29821 = EDGE_CURVE ( 'NONE', #36216, #18546, #8200, .T. ) ;
#29822 = DIRECTION ( 'NONE',  ( 1.000000000000000000, 0.000000000000000000, 0.000000000000000000 ) ) ;
#29823 = CIRCLE ( 'NONE', #41665, 20.00000000000000355 ) ;
#29825 = ORIENTED_EDGE ( 'NONE', *, *, #40986, .F. ) ;
#29824 = DIRECTION ( 'NONE',  ( 0.000000000000000000, 0.000000000000000000, 1.000000000000000000 ) ) ;
#29826 = CARTESIAN_POINT ( 'NONE',  ( -14.91913624998189469, 31.00000000000000355, -30.37684071746364012 ) ) ;
#29827 = EDGE_CURVE ( 'NONE', #33572, #27194, #29140, .T. ) ;
#29828 = DIRECTION ( 'NONE',  ( -1.000000000000000000, -0.000000000000000000, -0.000000000000000000 ) ) ;
#29829 = CIRCLE ( 'NONE', #1236, 120.5010000000000474 ) ;
#29830 = EDGE_CURVE ( 'NONE', #16376, #36189, #22908, .T. ) ;
#29832 = ORIENTED_EDGE ( 'NONE', *, *, #17576, .F. ) ;
#29831 = DIRECTION ( 'NONE',  ( 1.000000000000000000, 0.000000000000000000, -0.000000000000000000 ) ) ;
#29833 = ORIENTED_EDGE ( 'NONE', *, *, #9150, .T. ) ;
#29834 = CARTESIAN_POINT ( 'NONE',  ( 17.99999999999999645, -114.1529630473452386, 38.59523323561398200 ) ) ;
#29835 = DIRECTION ( 'NONE',  ( 0.000000000000000000, 0.6736956436465532105, 0.7390089172206629753 ) ) ;
#29836 = CARTESIAN_POINT ( 'NONE',  ( 7.251580242022520828, 40.00000000000000000, -54.34182998362662431 ) ) ;
#29837 = DIRECTION ( 'NONE',  ( 0.000000000000000000, -0.1253332335643113082, 0.9921147013144769877 ) ) ;
#29838 = CIRCLE ( 'NONE', #1244, 12.50000000000000000 ) ;
#29839 = CARTESIAN_POINT ( 'NONE',  ( 0.000000000000000000, 0.000000000000000000, 0.000000000000000000 ) ) ;
#29840 = DIRECTION ( 'NONE',  ( 0.000000000000000000, 1.599473849036242511E-14, -1.000000000000000000 ) ) ;
#29841 = EDGE_LOOP ( 'NONE', ( #10508, #36235, #31526, #30383 ) ) ;
#29842 = DIRECTION ( 'NONE',  ( 0.000000000000000000, 0.1253332335642974860, 0.9921147013144787641 ) ) ;
#29843 = ORIENTED_EDGE ( 'NONE', *, *, #18626, .T. ) ;
#29844 = DIRECTION ( 'NONE',  ( 0.000000000000000000, 0.8477344278896686847, 0.5304209081197462927 ) ) ;
#29845 = CARTESIAN_POINT ( 'NONE',  ( 0.000000000000000000, -13.85708833599999323, 45.43276465116659324 ) ) ;
#29846 = CARTESIAN_POINT ( 'NONE',  ( 6.892732713553924917, 31.00000000000000355, -52.36990085009771434 ) ) ;
#29848 = ADVANCED_FACE ( 'NONE', ( #24313 ), #1775, .F. ) ;
#29847 = AXIS2_PLACEMENT_3D ( 'NONE', #34944, #18205, #17996 ) ;
#29849 = DIRECTION ( 'NONE',  ( 1.000000000000000000, 0.000000000000000000, 0.000000000000000000 ) ) ;
#29850 = ORIENTED_EDGE ( 'NONE', *, *, #22395, .T. ) ;
#29851 = EDGE_CURVE ( 'NONE', #13195, #8854, #3335, .T. ) ;
#29852 = EDGE_CURVE ( 'NONE', #36282, #17321, #22532, .T. ) ;
#29853 = AXIS2_PLACEMENT_3D ( 'NONE', #41852, #6479, #3188 ) ;
#29854 = AXIS2_PLACEMENT_3D ( 'NONE', #37014, #1221, #13920 ) ;
#29855 = ADVANCED_FACE ( 'NONE', ( #16181 ), #25796, .T. ) ;
#29856 = DIRECTION ( 'NONE',  ( 1.000000000000000000, 1.836909530733573776E-16, 0.000000000000000000 ) ) ;
#29857 = ORIENTED_EDGE ( 'NONE', *, *, #27733, .F. ) ;
#29858 = CARTESIAN_POINT ( 'NONE',  ( 86.04713929520032423, 31.00000000000000000, 42.41619695850760507 ) ) ;
#29859 = AXIS2_PLACEMENT_3D ( 'NONE', #23663, #42806, #3314 ) ;
#29860 = VERTEX_POINT ( 'NONE', #39255 ) ;
#29861 = CARTESIAN_POINT ( 'NONE',  ( 109.0695705685741075, 106.4195705685767166, 6.999999999999998224 ) ) ;
#29862 = VERTEX_POINT ( 'NONE', #19471 ) ;
#29864 = CARTESIAN_POINT ( 'NONE',  ( -48.52617905695110068, 31.00000000000000355, 37.10499320822106029 ) ) ;
#29863 = AXIS2_PLACEMENT_3D ( 'NONE', #15128, #41704, #21897 ) ;
#29865 = CARTESIAN_POINT ( 'NONE',  ( 4.329677741076332964, 40.00000000000000000, -64.59417075179260337 ) ) ;
#29866 = CARTESIAN_POINT ( 'NONE',  ( -60.10374203099167545, 40.00000000000000711, 78.35501831527777483 ) ) ;
#29867 = ORIENTED_EDGE ( 'NONE', *, *, #25834, .T. ) ;
#29868 = VERTEX_POINT ( 'NONE', #42743 ) ;
#29869 = CARTESIAN_POINT ( 'NONE',  ( -2.756197834950067094, -3.027510591568735254, -3.223146290109809797 ) ) ;
#29870 = ADVANCED_FACE ( 'NONE', ( #42334 ), #12900, .T. ) ;
#29871 = CARTESIAN_POINT ( 'NONE',  ( -15.99999999999997691, 31.00000000000000355, 5.571627607371296764E-15 ) ) ;
#29872 = DIRECTION ( 'NONE',  ( 0.000000000000000000, 0.000000000000000000, 1.000000000000000000 ) ) ;
#29874 = ORIENTED_EDGE ( 'NONE', *, *, #43160, .T. ) ;
#29873 = CYLINDRICAL_SURFACE ( 'NONE', #40137, 116.0000000000000000 ) ;
#29875 = CYLINDRICAL_SURFACE ( 'NONE', #35158, 13.59999999999999964 ) ;
#29876 = ORIENTED_EDGE ( 'NONE', *, *, #28334, .T. ) ;
#29877 = CARTESIAN_POINT ( 'NONE',  ( 3.355112389629172576, -2.681727112203168950, -0.2256878752776777242 ) ) ;
#29878 = CARTESIAN_POINT ( 'NONE',  ( -5.726861599740728614, 40.00000000000000000, 87.60416666588449175 ) ) ;
#29879 = DIRECTION ( 'NONE',  ( 0.000000000000000000, 0.000000000000000000, 1.000000000000000000 ) ) ;
#29880 = EDGE_LOOP ( 'NONE', ( #18475, #11248, #13280, #26353, #38069, #30195, #12609, #34906, #8436, #33719, #34949, #122, #19781, #42149, #33106, #21910, #11094, #14063, #6779, #12844, #4460, #24397, #11021, #38923, #3626, #34820, #37533, #12818, #3036, #18045, #4439, #40236, #35699, #37410, #4516, #11443, #10379, #25698, #20908, #36489, #9706, #9992, #21693, #16791, #24885, #11540, #41710, #9451, #2366, #7539, #1726, #35228, #19322, #26906, #33501, #37731, #26475, #16070, #7468, #5085, #18925, #7915, #12872, #10265, #6337, #23891, #12595, #28031, #39481, #6215, #40874, #15508, #29511, #34320, #32898, #8336, #40211, #23066, #31684, #3079, #16881, #37386, #17044, #29390, #3975, #10660, #25465, #10650, #4398, #29998, #24314, #6400, #26902, #12302, #10042, #20202, #2659, #8357, #42124, #9493, #18834, #12754, #37563, #36875, #33645, #20326, #36675, #14722, #5663, #29929, #41228, #25957, #38722, #23709, #21533, #15767, #21993, #10815, #3392, #28558, #10206, #20503, #30980, #28158, #21685, #25620, #13733, #28911, #15584, #15491, #35301, #582, #18704, #17934, #24606, #38148, #11639, #15912, #35840, #37706, #20887, #34402, #37408, #25602, #12643, #15706, #31045, #30747, #16193, #37949, #39436, #5003, #13478, #15295, #19252, #15788, #36986, #33926, #20122, #4578, #36197, #16111, #12413, #19508, #39841, #36114, #7334, #7211, #32368, #5190, #41547, #29930, #12480, #13811, #12870, #32372, #35119, #16438, #12596, #12245, #34677, #23238, #15697, #34709, #16980, #16885, #25116, #28538, #6171, #26128, #29310, #2789, #4479, #9678, #36325, #6825, #25445, #20134, #6591, #19422, #17648, #40472, #30732, #11255, #34333, #40260, #30510, #2281, #37178, #11440, #10633, #30687, #11363, #30899, #13890, #3134, #32399, #8797, #29279, #13397, #37398, #34156, #5155, #37662, #23257, #40452, #31795, #20195, #14484, #5354, #39308, #19597, #3086, #25097, #21946, #30254, #18222, #18118, #177, #12863, #16783, #28504, #33743, #13355, #20614, #15763, #1841, #12520, #29154, #19983, #32425, #27881, #8018, #19338, #14122, #10830, #41779, #24787, #19809, #30121, #1232, #21214, #16689, #78, #39794, #24086, #29989, #27689, #13736, #26688, #20488, #39028, #20533, #4193, #23965, #748, #34544, #13655, #2674, #37238, #13626, #35967, #23615, #41059, #24525, #13240, #8369, #31952, #20706, #32113, #3315, #15598, #2017, #11239, #39145, #36136, #678, #30710, #40173, #23034, #6162, #24975, #21540, #27203, #18306, #30430, #23520, #7757, #22219, #20358, #5052, #7721, #30646, #36659, #41363, #6827, #18161, #8978, #21512, #29734, #38221, #25390, #34838, #16864, #32696, #21646, #6857, #6099, #34214, #10435, #29367, #39568, #17136, #40022, #12860, #22556, #3640, #18372, #20290, #29113, #29301, #21517, #3252, #21492, #2152, #14738, #20381, #22061, #14420, #27355, #20809, #23329, #19239, #24110, #30134, #18445, #3903, #9069, #15308, #38824, #20519, #5475, #17103, #30541, #14901, #35674, #23670, #3442, #37990, #39385, #5314, #25864, #2802, #28746, #26567, #864, #11802, #14665, #24889, #39251, #29280, #21602, #24584, #11191, #18014, #36265, #38249, #4500, #10091, #38466, #25413, #11946, #39565, #12351, #32153, #10749, #41319, #40568, #36341, #26171, #1002, #34303, #37850, #42838, #13959, #12141, #4751, #26839, #30075, #26491, #40392, #5325, #14532, #14585, #38264, #20293, #26762, #20483, #32382, #37602, #11485, #32618, #30664, #7545, #5614, #3063, #1420, #8598, #39169, #36364, #18923, #13949, #17766, #37872, #33497, #22331, #35672, #13101, #39698, #23822, #16700, #25704, #13440, #4174, #35409, #30143, #22972, #37821, #15562, #26108, #26165, #24478, #37522, #14071, #28253, #7815, #38727, #210, #19915, #21898, #36840, #43040, #4355, #34236, #19881, #39093, #42156, #20505, #31672, #6225, #23695, #40159, #39233, #15159, #1884, #20841, #37785 ) ) ;
#29881 = FACE_OUTER_BOUND ( 'NONE', #27924, .T. ) ;
#29882 = CIRCLE ( 'NONE', #11066, 120.5010000000000190 ) ;
#29883 = DIRECTION ( 'NONE',  ( 0.000000000000000000, 0.000000000000000000, -1.000000000000000000 ) ) ;
#29884 = ORIENTED_EDGE ( 'NONE', *, *, #30498, .T. ) ;
#29885 = EDGE_CURVE ( 'NONE', #31507, #20227, #26366, .T. ) ;
#29886 = AXIS2_PLACEMENT_3D ( 'NONE', #25021, #38049, #41307 ) ;
#29887 = ORIENTED_EDGE ( 'NONE', *, *, #18135, .F. ) ;
#29888 = DIRECTION ( 'NONE',  ( 3.009274222672345096E-17, 1.000000000000000000, -2.455023325076454960E-18 ) ) ;
#29889 = ORIENTED_EDGE ( 'NONE', *, *, #8813, .F. ) ;
#29890 = CARTESIAN_POINT ( 'NONE',  ( 0.000000000000000000, -15.21076497709635156, -119.5371223922156503 ) ) ;
#29891 = CARTESIAN_POINT ( 'NONE',  ( 21.00000000000000355, 2.789133085058097101E-16, -2.055000000000000160 ) ) ;
#29892 = CARTESIAN_POINT ( 'NONE',  ( 0.000000000000000000, 72.00556975657703163, 86.04342158279412445 ) ) ;
#29893 = DIRECTION ( 'NONE',  ( -1.000000000000000000, 0.000000000000000000, 0.000000000000000000 ) ) ;
#29894 = DIRECTION ( 'NONE',  ( -1.000000000000000000, 0.000000000000000000, -0.000000000000000000 ) ) ;
#29895 = ORIENTED_EDGE ( 'NONE', *, *, #14790, .T. ) ;
#29896 = DIRECTION ( 'NONE',  ( -1.000000000000000000, -0.000000000000000000, 0.000000000000000000 ) ) ;
#29897 = EDGE_LOOP ( 'NONE', ( #2183, #27942, #18790, #29770 ) ) ;
#29898 = DIRECTION ( 'NONE',  ( 0.000000000000000000, 0.000000000000000000, 1.000000000000000000 ) ) ;
#29899 = ADVANCED_FACE ( 'NONE', ( #19255 ), #32108, .T. ) ;
#29900 = DIRECTION ( 'NONE',  ( 0.000000000000000000, -0.1590634960190788760, 0.9872683547213435551 ) ) ;
#29901 = ORIENTED_EDGE ( 'NONE', *, *, #36202, .F. ) ;
#29902 = CARTESIAN_POINT ( 'NONE',  ( 9.000000000000001776, -109.3506818544107659, -38.70953859161123489 ) ) ;
#29903 = EDGE_CURVE ( 'NONE', #21574, #21438, #4024, .T. ) ;
#29904 = CARTESIAN_POINT ( 'NONE',  ( -45.51113419504475388, -2.055254544495720648, 56.57887602028989704 ) ) ;
#29905 = CONTEXT_DEPENDENT_SHAPE_REPRESENTATION ( #20638, #39130 ) ;
#29906 = CARTESIAN_POINT ( 'NONE',  ( 17.99999999999999645, 52.19040376560566585, -99.31985817764127944 ) ) ;
#29907 = CARTESIAN_POINT ( 'NONE',  ( -53.27196957865878346, 31.00000000000000711, 26.27224001321920355 ) ) ;
#29908 = AXIS2_PLACEMENT_3D ( 'NONE', #13669, #23499, #36978 ) ;
#29909 = ORIENTED_EDGE ( 'NONE', *, *, #41352, .T. ) ;
#29910 = CARTESIAN_POINT ( 'NONE',  ( 28.62564328229763788, 31.00000000000000355, -21.88780996306212501 ) ) ;
#29911 = CARTESIAN_POINT ( 'NONE',  ( -60.02123122004734768, 40.00000000000000711, 34.66859033927303813 ) ) ;
#29912 = AXIS2_PLACEMENT_3D ( 'NONE', #39253, #19254, #2613 ) ;
#29913 = EDGE_CURVE ( 'NONE', #26002, #18694, #1274, .T. ) ;
#29914 = FILL_AREA_STYLE ('',( #12525 ) ) ;
#29915 = EDGE_CURVE ( 'NONE', #25913, #28841, #32945, .T. ) ;
#29916 = DIRECTION ( 'NONE',  ( -3.996523416598930318E-16, 2.658563593772947863E-15, 1.000000000000000000 ) ) ;
#29917 = ORIENTED_EDGE ( 'NONE', *, *, #26835, .T. ) ;
#29918 = DIRECTION ( 'NONE',  ( 1.000000000000000000, 0.000000000000000000, 0.000000000000000000 ) ) ;
#29919 = CARTESIAN_POINT ( 'NONE',  ( 0.000000000000000000, 0.000000000000000000, 0.000000000000000000 ) ) ;
#29920 = ORIENTED_EDGE ( 'NONE', *, *, #743, .T. ) ;
#29921 = CARTESIAN_POINT ( 'NONE',  ( -36.80126402429788612, 40.00000000000000000, 32.28896105221774349 ) ) ;
#29922 = CARTESIAN_POINT ( 'NONE',  ( 17.99999999999999645, 114.6488492393079781, 37.09625815500054102 ) ) ;
#29923 = LINE ( 'NONE', #6973, #25005 ) ;
#29924 = ORIENTED_EDGE ( 'NONE', *, *, #13645, .T. ) ;
#29925 = DIRECTION ( 'NONE',  ( 0.000000000000000000, -0.7705132427757815927, -0.6374239897486989603 ) ) ;
#29926 = DIRECTION ( 'NONE',  ( -1.000000000000000000, -0.000000000000000000, 0.000000000000000000 ) ) ;
#29927 = ORIENTED_EDGE ( 'NONE', *, *, #24790, .T. ) ;
#29928 = FACE_OUTER_BOUND ( 'NONE', #39325, .T. ) ;
#29929 = ORIENTED_EDGE ( 'NONE', *, *, #36981, .T. ) ;
#29930 = ORIENTED_EDGE ( 'NONE', *, *, #25691, .T. ) ;
#29931 = CARTESIAN_POINT ( 'NONE',  ( -19.85879968743109458, -12.05525454449572109, 67.01652747270929922 ) ) ;
#29932 = CARTESIAN_POINT ( 'NONE',  ( -55.31949386280458469, 31.00000000000000711, 71.91600076666669850 ) ) ;
#29933 = ORIENTED_EDGE ( 'NONE', *, *, #19657, .T. ) ;
#29934 = CARTESIAN_POINT ( 'NONE',  ( 9.000000000000001776, 11.65176648921033298, 115.4133282497342918 ) ) ;
#29935 = AXIS2_PLACEMENT_3D ( 'NONE', #39754, #40405, #23445 ) ;
#29936 = VECTOR ( 'NONE', #9855, 1000.000000000000000 ) ;
#29937 = CARTESIAN_POINT ( 'NONE',  ( -10.00000000000000000, 0.000000000000000000, 0.000000000000000000 ) ) ;
#29938 = DIRECTION ( 'NONE',  ( 0.000000000000000000, 0.000000000000000000, 1.000000000000000000 ) ) ;
#29939 = EDGE_LOOP ( 'NONE', ( #12674, #28608, #6653, #38396 ) ) ;
#29940 = DIRECTION ( 'NONE',  ( 1.000000000000000000, 0.000000000000000000, 0.000000000000000000 ) ) ;
#29941 = CARTESIAN_POINT ( 'NONE',  ( 3.413765605486547727, -14.29811891091961229, -1.199999999999999956 ) ) ;
#29943 = LINE ( 'NONE', #36441, #20586 ) ;
#29942 = CARTESIAN_POINT ( 'NONE',  ( 18.00000000000000355, 0.000000000000000000, 0.000000000000000000 ) ) ;
#29944 = EDGE_CURVE ( 'NONE', #27398, #22603, #25702, .T. ) ;
#29945 = DIRECTION ( 'NONE',  ( 0.000000000000000000, -0.7705132427757950264, 0.6374239897486826401 ) ) ;
#29946 = EDGE_CURVE ( 'NONE', #4177, #39762, #37496, .T. ) ;
#29947 = EDGE_LOOP ( 'NONE', ( #10861, #41432, #18708, #40841 ) ) ;
#29948 = CARTESIAN_POINT ( 'NONE',  ( -19.19493090124598922, 31.00000000000000355, -25.00897302100653263 ) ) ;
#29949 = ORIENTED_EDGE ( 'NONE', *, *, #26579, .T. ) ;
#29950 = FACE_OUTER_BOUND ( 'NONE', #24767, .T. ) ;
#29951 = FACE_OUTER_BOUND ( 'NONE', #39826, .T. ) ;
#29952 = VERTEX_POINT ( 'NONE', #29270 ) ;
#29953 = DIRECTION ( 'NONE',  ( -1.000000000000000000, 0.000000000000000000, 0.000000000000000000 ) ) ;
#29954 = CARTESIAN_POINT ( 'NONE',  ( -38.45388554590046937, 40.00000000000000000, -13.05014827191142679 ) ) ;
#29955 = CARTESIAN_POINT ( 'NONE',  ( -21.81649963859176822, 40.00000000000000000, -37.93159502954524243 ) ) ;
#29956 = EDGE_CURVE ( 'NONE', #37810, #2041, #12452, .T. ) ;
#29957 = CIRCLE ( 'NONE', #25110, 59.00000000000000711 ) ;
#29958 = ORIENTED_EDGE ( 'NONE', *, *, #7879, .T. ) ;
#29959 = AXIS2_PLACEMENT_3D ( 'NONE', #35250, #28534, #7780 ) ;
#29960 = ORIENTED_EDGE ( 'NONE', *, *, #14876, .F. ) ;
#29961 = CARTESIAN_POINT ( 'NONE',  ( 17.99999999999999645, 0.000000000000000000, 0.000000000000000000 ) ) ;
#29962 = EDGE_CURVE ( 'NONE', #3796, #38173, #34013, .T. ) ;
#29963 = CARTESIAN_POINT ( 'NONE',  ( -10.00000000000000000, 0.000000000000000000, 0.000000000000000000 ) ) ;
#29964 = AXIS2_PLACEMENT_3D ( 'NONE', #16405, #29706, #3686 ) ;
#29965 = DIRECTION ( 'NONE',  ( 1.000000000000000000, 0.000000000000000000, -6.546126324440850663E-16 ) ) ;
#29966 = CARTESIAN_POINT ( 'NONE',  ( 17.99999999999999645, 91.51415974874592507, 64.91094698989330425 ) ) ;
#29967 = VERTEX_POINT ( 'NONE', #25375 ) ;
#29968 = LINE ( 'NONE', #43024, #23608 ) ;
#29969 = ORIENTED_EDGE ( 'NONE', *, *, #18974, .T. ) ;
#29970 = DIRECTION ( 'NONE',  ( 0.000000000000000000, 0.000000000000000000, -1.000000000000000000 ) ) ;
#29971 = CARTESIAN_POINT ( 'NONE',  ( 0.000000000000000000, -46.90537658765328644, -2.727856614654796452 ) ) ;
#29972 = ORIENTED_EDGE ( 'NONE', *, *, #38768, .T. ) ;
#29973 = CARTESIAN_POINT ( 'NONE',  ( 17.99999999999999645, 0.000000000000000000, 0.000000000000000000 ) ) ;
#29974 = CARTESIAN_POINT ( 'NONE',  ( 52.26814377733353467, -12.05525454449572464, -19.42827587850796434 ) ) ;
#29975 = ORIENTED_EDGE ( 'NONE', *, *, #16824, .F. ) ;
#29976 = CARTESIAN_POINT ( 'NONE',  ( 17.99999999999999645, -98.69720329640912837, -60.94966826380012037 ) ) ;
#29977 = ORIENTED_EDGE ( 'NONE', *, *, #18541, .T. ) ;
#29978 = DIRECTION ( 'NONE',  ( -0.000000000000000000, -0.000000000000000000, 1.000000000000000000 ) ) ;
#29979 = EDGE_CURVE ( 'NONE', #2427, #18000, #21521, .T. ) ;
#29980 = EDGE_LOOP ( 'NONE', ( #39852, #33330, #30298, #4136 ) ) ;
#29982 = VERTEX_POINT ( 'NONE', #35372 ) ;
#29981 = DIRECTION ( 'NONE',  ( 0.000000000000000000, 0.000000000000000000, 1.000000000000000000 ) ) ;
#29983 = CARTESIAN_POINT ( 'NONE',  ( -61.40313508884858607, 31.00000000000000711, 7.989450542815522027 ) ) ;
#29985 = EDGE_CURVE ( 'NONE', #28114, #28849, #9180, .T. ) ;
#29984 = ORIENTED_EDGE ( 'NONE', *, *, #16930, .T. ) ;
#29986 = CARTESIAN_POINT ( 'NONE',  ( 42.80287614962790599, -40.05525454449572464, 69.29271901957253021 ) ) ;
#29987 = ORIENTED_EDGE ( 'NONE', *, *, #39892, .F. ) ;
#29988 = CYLINDRICAL_SURFACE ( 'NONE', #32859, 59.00000000000000000 ) ;
#29989 = ORIENTED_EDGE ( 'NONE', *, *, #6924, .F. ) ;
#29990 = CARTESIAN_POINT ( 'NONE',  ( 68.41293481152064260, 39.99999999999999289, -52.34142988144959219 ) ) ;
#29991 = AXIS2_PLACEMENT_3D ( 'NONE', #16678, #43022, #14191 ) ;
#29992 = CIRCLE ( 'NONE', #13270, 116.0000000000000000 ) ;
#29993 = CIRCLE ( 'NONE', #17495, 120.5010000000000332 ) ;
#29995 = CARTESIAN_POINT ( 'NONE',  ( 17.99999999999999645, -54.09091620264790379, 102.6166301549515936 ) ) ;
#29994 = DIRECTION ( 'NONE',  ( -1.000000000000000000, -0.000000000000000000, -0.000000000000000000 ) ) ;
#29996 = AXIS2_PLACEMENT_3D ( 'NONE', #6328, #39683, #19673 ) ;
#29997 = DIRECTION ( 'NONE',  ( 0.000000000000000000, 0.000000000000000000, 1.000000000000000000 ) ) ;
#29998 = ORIENTED_EDGE ( 'NONE', *, *, #35311, .T. ) ;
#29999 = LINE ( 'NONE', #33254, #5640 ) ;
#30000 = EDGE_CURVE ( 'NONE', #17019, #10305, #12421, .T. ) ;
#30001 = ORIENTED_EDGE ( 'NONE', *, *, #41455, .T. ) ;
#30002 = SURFACE_STYLE_FILL_AREA ( #3112 ) ;
#30003 = DIRECTION ( 'NONE',  ( 0.000000000000000000, -0.05322217484216511946, -0.9985826956767627216 ) ) ;
#30004 = CARTESIAN_POINT ( 'NONE',  ( 70.67261647610648367, 31.00000000000000000, -24.00465245562410743 ) ) ;
#30006 = DIRECTION ( 'NONE',  ( 0.000000000000000000, 0.000000000000000000, 1.000000000000000000 ) ) ;
#30005 = FACE_OUTER_BOUND ( 'NONE', #42910, .T. ) ;
#30007 = ORIENTED_EDGE ( 'NONE', *, *, #42325, .F. ) ;
#30008 = CARTESIAN_POINT ( 'NONE',  ( 17.99999999999999645, 111.1352304691227744, 15.40237066878635730 ) ) ;
#30009 = EDGE_CURVE ( 'NONE', #28297, #23529, #34695, .T. ) ;
#30010 = CIRCLE ( 'NONE', #23054, 59.00000000000000000 ) ;
#30011 = ORIENTED_EDGE ( 'NONE', *, *, #36812, .T. ) ;
#30012 = CARTESIAN_POINT ( 'NONE',  ( 9.000000000000001776, 25.61928775981044382, 45.25098998563486674 ) ) ;
#30013 = EDGE_CURVE ( 'NONE', #15607, #22119, #36767, .T. ) ;
#30014 = CARTESIAN_POINT ( 'NONE',  ( 17.99999999999999645, 0.000000000000000000, 0.000000000000000000 ) ) ;
#30015 = CARTESIAN_POINT ( 'NONE',  ( -101.1468392227577340, 31.00000000000000711, 13.20405500233197671 ) ) ;
#30016 = EDGE_CURVE ( 'NONE', #29982, #25474, #24274, .T. ) ;
#30017 = CARTESIAN_POINT ( 'NONE',  ( 17.99999999999999645, 26.29521155129848964, 17.34211205339357065 ) ) ;
#30018 = AXIS2_PLACEMENT_3D ( 'NONE', #9949, #40033, #23299 ) ;
#30019 = ORIENTED_EDGE ( 'NONE', *, *, #3598, .T. ) ;
#30020 = DIRECTION ( 'NONE',  ( -1.000000000000000000, -0.000000000000000000, -0.000000000000000000 ) ) ;
#30021 = EDGE_LOOP ( 'NONE', ( #30841, #26705, #20850, #19950 ) ) ;
#30022 = VECTOR ( 'NONE', #34632, 1000.000000000000000 ) ;
#30023 = DIRECTION ( 'NONE',  ( -1.000000000000000000, -0.000000000000000000, -0.000000000000000000 ) ) ;
#30024 = CIRCLE ( 'NONE', #7733, 120.5010000000000474 ) ;
#30025 = AXIS2_PLACEMENT_3D ( 'NONE', #37900, #21607, #21390 ) ;
#30026 = CARTESIAN_POINT ( 'NONE',  ( 106.4195705685741302, 106.4195705685767166, 6.999999999999998224 ) ) ;
#30027 = DIRECTION ( 'NONE',  ( 1.000000000000000000, -0.000000000000000000, -0.000000000000000000 ) ) ;
#30028 = EDGE_LOOP ( 'NONE', ( #23531, #38597, #36610, #34410 ) ) ;
#30029 = ORIENTED_EDGE ( 'NONE', *, *, #1960, .T. ) ;
#30030 = DIRECTION ( 'NONE',  ( 0.000000000000000000, 0.000000000000000000, 1.000000000000000000 ) ) ;
#30031 = CYLINDRICAL_SURFACE ( 'NONE', #13757, 13.59999999999999964 ) ;
#30032 = CYLINDRICAL_SURFACE ( 'NONE', #4845, 1.000000000000000444 ) ;
#30034 = VERTEX_POINT ( 'NONE', #629 ) ;
#30033 = DIRECTION ( 'NONE',  ( 0.000000000000000000, 0.000000000000000000, 1.000000000000000000 ) ) ;
#30035 = CARTESIAN_POINT ( 'NONE',  ( -22.00208165626505519, 31.00000000000000355, -25.16137218361809502 ) ) ;
#30036 = EDGE_CURVE ( 'NONE', #33918, #35878, #34035, .T. ) ;
#30037 = CARTESIAN_POINT ( 'NONE',  ( 18.00000000000000355, 36.05989434073656952, -30.12041790338580682 ) ) ;
#30038 = EDGE_CURVE ( 'NONE', #15861, #18124, #20332, .T. ) ;
#30040 = ORIENTED_EDGE ( 'NONE', *, *, #18295, .F. ) ;
#30039 = DIRECTION ( 'NONE',  ( -0.000000000000000000, -0.000000000000000000, 1.000000000000000000 ) ) ;
#30041 = VERTEX_POINT ( 'NONE', #17053 ) ;
#30042 = LINE ( 'NONE', #32435, #19864 ) ;
#30043 = CARTESIAN_POINT ( 'NONE',  ( -10.00000000000000000, 0.000000000000000000, 0.000000000000000000 ) ) ;
#30044 = CARTESIAN_POINT ( 'NONE',  ( -3.469229457552012619, 40.00000000000000000, -54.39987425098301799 ) ) ;
#30045 = LINE ( 'NONE', #36775, #7636 ) ;
#30046 = LINE ( 'NONE', #27407, #4031 ) ;
#30047 = DIRECTION ( 'NONE',  ( 0.000000000000000000, 0.000000000000000000, 1.000000000000000000 ) ) ;
#30048 = ORIENTED_EDGE ( 'NONE', *, *, #30498, .F. ) ;
#30049 = CARTESIAN_POINT ( 'NONE',  ( 8.919999999999998153, 1.352010066258677905E-15, -11.00000000000000000 ) ) ;
#30050 = VERTEX_POINT ( 'NONE', #24029 ) ;
#30051 = DIRECTION ( 'NONE',  ( -1.000000000000000000, 0.000000000000000000, 0.000000000000000000 ) ) ;
#30052 = DIRECTION ( 'NONE',  ( 0.000000000000000000, 0.5264321628773507289, 0.8502171357296173237 ) ) ;
#30053 = AXIS2_PLACEMENT_3D ( 'NONE', #24753, #14705, #24983 ) ;
#30054 = CARTESIAN_POINT ( 'NONE',  ( 28.83751338862256119, 31.00000000000000355, -32.88701605462710376 ) ) ;
#30055 = DIRECTION ( 'NONE',  ( 0.000000000000000000, 0.000000000000000000, 1.000000000000000000 ) ) ;
#30056 = VERTEX_POINT ( 'NONE', #16633 ) ;
#30057 = VECTOR ( 'NONE', #16948, 1000.000000000000000 ) ;
#30058 = CARTESIAN_POINT ( 'NONE',  ( 17.99999999999999645, 0.000000000000000000, 0.000000000000000000 ) ) ;
#30059 = ORIENTED_EDGE ( 'NONE', *, *, #10617, .T. ) ;
#30060 = EDGE_CURVE ( 'NONE', #3503, #13758, #2618, .T. ) ;
#30061 = CARTESIAN_POINT ( 'NONE',  ( -20.07939870814534089, 40.00000000000000000, -2.638545259751242877 ) ) ;
#30062 = AXIS2_PLACEMENT_3D ( 'NONE', #5662, #12456, #8948 ) ;
#30063 = ORIENTED_EDGE ( 'NONE', *, *, #10507, .T. ) ;
#30064 = ADVANCED_FACE ( 'NONE', ( #4123 ), #10256, .F. ) ;
#30065 = CARTESIAN_POINT ( 'NONE',  ( 17.99999999999999645, -75.03166794516862126, 94.29071961951481740 ) ) ;
#30066 = CARTESIAN_POINT ( 'NONE',  ( 47.76959191294547225, 31.00000000000000355, 62.44753968350421047 ) ) ;
#30067 = CARTESIAN_POINT ( 'NONE',  ( -49.21613380539481142, 40.00000000000000000, 63.96793098899348706 ) ) ;
#30068 = CYLINDRICAL_SURFACE ( 'NONE', #34144, 59.00000000000000000 ) ;
#30069 = ORIENTED_EDGE ( 'NONE', *, *, #26066, .T. ) ;
#30070 = ORIENTED_EDGE ( 'NONE', *, *, #42019, .F. ) ;
#30071 = CARTESIAN_POINT ( 'NONE',  ( 17.99999999999999645, 0.000000000000000000, 0.000000000000000000 ) ) ;
#30072 = DIRECTION ( 'NONE',  ( 0.000000000000000000, 0.000000000000000000, 1.000000000000000000 ) ) ;
#30073 = CARTESIAN_POINT ( 'NONE',  ( -4.101948962585906244, 2.368261337751074169, -3.681124513963621503 ) ) ;
#30075 = ORIENTED_EDGE ( 'NONE', *, *, #17174, .T. ) ;
#30074 = DIRECTION ( 'NONE',  ( -1.000000000000000000, 0.000000000000000000, 0.000000000000000000 ) ) ;
#30076 = LINE ( 'NONE', #10196, #39993 ) ;
#30077 = VERTEX_POINT ( 'NONE', #185 ) ;
#30078 = DIRECTION ( 'NONE',  ( 0.000000000000000000, 0.000000000000000000, 1.000000000000000000 ) ) ;
#30079 = CARTESIAN_POINT ( 'NONE',  ( -64.44063486737354651, 40.00000000000000711, -49.42892067282641477 ) ) ;
#30080 = CARTESIAN_POINT ( 'NONE',  ( 0.000000000000000000, -17.50309955389642269, 43.60271849949357659 ) ) ;
#30081 = AXIS2_PLACEMENT_3D ( 'NONE', #16860, #26434, #9835 ) ;
#30082 = ORIENTED_EDGE ( 'NONE', *, *, #30198, .F. ) ;
#30083 = EDGE_CURVE ( 'NONE', #21051, #39595, #9623, .T. ) ;
#30084 = DIRECTION ( 'NONE',  ( 1.000000000000000000, 0.000000000000000000, 0.000000000000000000 ) ) ;
#30085 = EDGE_CURVE ( 'NONE', #38633, #29515, #15913, .T. ) ;
#30086 = DIRECTION ( 'NONE',  ( 0.000000000000000000, 0.000000000000000000, 1.000000000000000000 ) ) ;
#30087 = EDGE_CURVE ( 'NONE', #42455, #42118, #41669, .T. ) ;
#30088 = EDGE_CURVE ( 'NONE', #15352, #30905, #29923, .T. ) ;
#30089 = AXIS2_PLACEMENT_3D ( 'NONE', #32527, #6535, #23379 ) ;
#30090 = ORIENTED_EDGE ( 'NONE', *, *, #926, .F. ) ;
#30091 = EDGE_LOOP ( 'NONE', ( #27518, #3499, #10995, #18470 ) ) ;
#30092 = CARTESIAN_POINT ( 'NONE',  ( 17.99999999999999645, 5.919241748380035695, -31.39643714728450163 ) ) ;
#30093 = EDGE_LOOP ( 'NONE', ( #198, #1022, #11692, #25489 ) ) ;
#30095 = CARTESIAN_POINT ( 'NONE',  ( 27.02985023942251885, 40.00000000000000000, 3.586895573513070090 ) ) ;
#30094 = AXIS2_PLACEMENT_3D ( 'NONE', #39133, #22826, #40850 ) ;
#30096 = DIRECTION ( 'NONE',  ( 0.000000000000000000, 0.000000000000000000, 1.000000000000000000 ) ) ;
#30097 = CARTESIAN_POINT ( 'NONE',  ( 0.000000000000000000, -112.5220807139882311, -28.19186676675956704 ) ) ;
#30098 = DIRECTION ( 'NONE',  ( -1.000000000000000000, -0.000000000000000000, -0.000000000000000000 ) ) ;
#30099 = DIRECTION ( 'NONE',  ( 0.1305261922200512403, -0.9914448613738104932, 0.000000000000000000 ) ) ;
#30100 = ORIENTED_EDGE ( 'NONE', *, *, #1053, .F. ) ;
#30102 = CARTESIAN_POINT ( 'NONE',  ( 0.000000000000000000, -92.25992191227339845, -77.51514567967485902 ) ) ;
#30101 = CARTESIAN_POINT ( 'NONE',  ( 18.00000000000000355, -44.61570720899106846, 14.73072383765551940 ) ) ;
#30103 = VERTEX_POINT ( 'NONE', #39904 ) ;
#30104 = FACE_OUTER_BOUND ( 'NONE', #16702, .T. ) ;
#30105 = CARTESIAN_POINT ( 'NONE',  ( 0.000000000000000000, 0.000000000000000000, 0.000000000000000000 ) ) ;
#30106 = ORIENTED_EDGE ( 'NONE', *, *, #14735, .F. ) ;
#30107 = CARTESIAN_POINT ( 'NONE',  ( 0.000000000000000000, 12.30077720129096264, 50.52416135122086871 ) ) ;
#30108 = CYLINDRICAL_SURFACE ( 'NONE', #19592, 12.55910585664918422 ) ;
#30109 = DIRECTION ( 'NONE',  ( -3.996523416598930318E-16, 2.658563593772947863E-15, 1.000000000000000000 ) ) ;
#30110 = CARTESIAN_POINT ( 'NONE',  ( -62.26029918285335896, 31.00000000000000711, 30.70375207684418228 ) ) ;
#30111 =( REPRESENTATION_RELATIONSHIP ('NONE','NONE', #330, #39082 ) REPRESENTATION_RELATIONSHIP_WITH_TRANSFORMATION ( #10235 )SHAPE_REPRESENTATION_RELATIONSHIP( ) );
#30112 = CIRCLE ( 'NONE', #28008, 130.0000000000000000 ) ;
#30113 = EDGE_CURVE ( 'NONE', #14112, #17801, #18748, .T. ) ;
#30114 = ORIENTED_EDGE ( 'NONE', *, *, #26875, .T. ) ;
#30115 = CARTESIAN_POINT ( 'NONE',  ( 32.62694724487210607, 31.00000000000000355, -16.02036196159510339 ) ) ;
#30116 = AXIS2_PLACEMENT_3D ( 'NONE', #22928, #19637, #26163 ) ;
#30117 = CARTESIAN_POINT ( 'NONE',  ( -79.27599250299880396, 40.00000000000000711, 10.45126230984107707 ) ) ;
#30118 = AXIS2_PLACEMENT_3D ( 'NONE', #34967, #1798, #4642 ) ;
#30119 = CARTESIAN_POINT ( 'NONE',  ( 17.99999999999999645, -64.58410930313458209, -101.7319213743688664 ) ) ;
#30120 = CARTESIAN_POINT ( 'NONE',  ( 17.99999999999999645, 72.00556975657821113, -86.04342158279314390 ) ) ;
#30121 = ORIENTED_EDGE ( 'NONE', *, *, #5831, .F. ) ;
#30122 = DIRECTION ( 'NONE',  ( -1.000000000000000000, -0.000000000000000000, 0.000000000000000000 ) ) ;
#30123 = DIRECTION ( 'NONE',  ( 0.000000000000000000, 0.000000000000000000, 1.000000000000000000 ) ) ;
#30124 = PRODUCT_DEFINITION_SHAPE ( 'NONE', 'NONE',  #32055 ) ;
#30125 = ORIENTED_EDGE ( 'NONE', *, *, #10792, .F. ) ;
#30126 = CARTESIAN_POINT ( 'NONE',  ( 54.89583333452979730, 40.00000000000000000, -3.599741573803383332 ) ) ;
#30127 = DIRECTION ( 'NONE',  ( 0.000000000000000000, 0.000000000000000000, 1.000000000000000000 ) ) ;
#30128 = CARTESIAN_POINT ( 'NONE',  ( 4.000000000000000000, 2.309401076758515803, -0.4999999999999995559 ) ) ;
#30129 = VERTEX_POINT ( 'NONE', #20774 ) ;
#30130 = CARTESIAN_POINT ( 'NONE',  ( 18.00000000000000355, -49.65209126885773827, 15.44894276735532657 ) ) ;
#30131 = DIRECTION ( 'NONE',  ( -1.000000000000000000, 0.000000000000000000, 0.000000000000000000 ) ) ;
#30132 = EDGE_CURVE ( 'NONE', #40692, #5278, #7537, .T. ) ;
#30133 = EDGE_CURVE ( 'NONE', #25132, #5730, #38180, .T. ) ;
#30134 = ORIENTED_EDGE ( 'NONE', *, *, #2354, .F. ) ;
#30135 = CYLINDRICAL_SURFACE ( 'NONE', #26296, 20.00000000000000000 ) ;
#30136 = ORIENTED_EDGE ( 'NONE', *, *, #3851, .F. ) ;
#30137 = ADVANCED_FACE ( 'NONE', ( #20126 ), #11745, .T. ) ;
#30138 = AXIS2_PLACEMENT_3D ( 'NONE', #10895, #23577, #24226 ) ;
#30139 = VERTEX_POINT ( 'NONE', #23814 ) ;
#30140 = CARTESIAN_POINT ( 'NONE',  ( 158.4999999999992042, -1.991533622299105221E-13, 6.999999999999939604 ) ) ;
#30141 = VECTOR ( 'NONE', #36465, 1000.000000000000000 ) ;
#30142 = CARTESIAN_POINT ( 'NONE',  ( -56.91377077966711084, 31.00000000000000355, -74.37798324515208037 ) ) ;
#30143 = ORIENTED_EDGE ( 'NONE', *, *, #6317, .T. ) ;
#30144 = DIRECTION ( 'NONE',  ( -1.000000000000000000, 0.000000000000000000, -0.000000000000000000 ) ) ;
#30145 = AXIS2_PLACEMENT_3D ( 'NONE', #11962, #8446, #18317 ) ;
#30146 = CARTESIAN_POINT ( 'NONE',  ( 17.99999999999999645, 0.000000000000000000, 0.000000000000000000 ) ) ;
#30147 = EDGE_CURVE ( 'NONE', #28016, #22117, #31939, .T. ) ;
#30148 = CARTESIAN_POINT ( 'NONE',  ( 9.000000000000001776, 31.17727234463848163, -111.7317219465816862 ) ) ;
#30149 = ORIENTED_EDGE ( 'NONE', *, *, #8640, .T. ) ;
#30150 = EDGE_CURVE ( 'NONE', #34172, #8500, #16638, .T. ) ;
#30151 = LINE ( 'NONE', #29717, #14804 ) ;
#30152 = DIRECTION ( 'NONE',  ( -1.000000000000000000, 0.000000000000000000, 0.000000000000000000 ) ) ;
#30153 = ADVANCED_FACE ( 'NONE', ( #33811 ), #26847, .F. ) ;
#30155 = DIRECTION ( 'NONE',  ( -1.000000000000000000, 0.000000000000000000, 0.000000000000000000 ) ) ;
#30154 = CARTESIAN_POINT ( 'NONE',  ( 17.99999999999999645, -117.9424311864590891, 24.69967462998996766 ) ) ;
#30156 = FACE_OUTER_BOUND ( 'NONE', #19153, .T. ) ;
#30157 = ORIENTED_EDGE ( 'NONE', *, *, #10535, .T. ) ;
#30158 = CARTESIAN_POINT ( 'NONE',  ( 22.24487986055951083, 31.00000000000000355, 28.98451114863597766 ) ) ;
#30159 = ORIENTED_EDGE ( 'NONE', *, *, #43094, .F. ) ;
#30160 = DIRECTION ( 'NONE',  ( -3.996523416598930318E-16, 2.658563593772947863E-15, 1.000000000000000000 ) ) ;
#30161 = DIRECTION ( 'NONE',  ( 0.000000000000000000, 0.000000000000000000, 1.000000000000000000 ) ) ;
#30162 = EDGE_LOOP ( 'NONE', ( #22856, #974, #3540, #18241 ) ) ;
#30163 = DIRECTION ( 'NONE',  ( 0.000000000000000000, -0.4999999999999993339, 0.8660254037844390407 ) ) ;
#30164 = EDGE_CURVE ( 'NONE', #10716, #19787, #36694, .T. ) ;
#30165 = CARTESIAN_POINT ( 'NONE',  ( 21.71086051706764763, 40.00000000000000000, -37.60982366119799991 ) ) ;
#30166 = CARTESIAN_POINT ( 'NONE',  ( 38.14553738578516828, 40.00000000000000000, 29.36968266378342207 ) ) ;
#30167 = ORIENTED_EDGE ( 'NONE', *, *, #7583, .T. ) ;
#30168 = CARTESIAN_POINT ( 'NONE',  ( 17.99999999999999645, -48.55277268144396174, 105.3500273609078306 ) ) ;
#30169 = DIRECTION ( 'NONE',  ( 0.000000000000000000, -0.1590634960190595026, -0.9872683547213466637 ) ) ;
#30170 = DIRECTION ( 'NONE',  ( 0.000000000000000000, 0.000000000000000000, 1.000000000000000000 ) ) ;
#30171 = VERTEX_POINT ( 'NONE', #8874 ) ;
#30172 = CARTESIAN_POINT ( 'NONE',  ( 11.86982580658625075, 40.00000000000000000, 24.05989836594520526 ) ) ;
#30173 = VERTEX_POINT ( 'NONE', #14642 ) ;
#30174 = LINE ( 'NONE', #13831, #32017 ) ;
#30175 = VECTOR ( 'NONE', #39881, 1000.000000000000000 ) ;
#30176 = DIRECTION ( 'NONE',  ( -1.000000000000000000, 0.000000000000000000, -0.000000000000000000 ) ) ;
#30177 = ORIENTED_EDGE ( 'NONE', *, *, #34904, .T. ) ;
#30178 = CARTESIAN_POINT ( 'NONE',  ( 17.99999999999999645, 0.000000000000000000, 0.000000000000000000 ) ) ;
#30179 = EDGE_CURVE ( 'NONE', #69, #2881, #34625, .T. ) ;
#30180 = CYLINDRICAL_SURFACE ( 'NONE', #15056, 20.00000000000000711 ) ;
#30181 = ORIENTED_EDGE ( 'NONE', *, *, #18112, .T. ) ;
#30182 = CARTESIAN_POINT ( 'NONE',  ( -10.00000000000000000, 0.000000000000000000, 0.000000000000000000 ) ) ;
#30183 = ORIENTED_EDGE ( 'NONE', *, *, #37504, .F. ) ;
#30184 = DIRECTION ( 'NONE',  ( 0.000000000000000000, 0.9911528310040067513, 0.1327255272837256084 ) ) ;
#30185 = VERTEX_POINT ( 'NONE', #42011 ) ;
#30187 = ORIENTED_EDGE ( 'NONE', *, *, #34982, .T. ) ;
#30186 = DIRECTION ( 'NONE',  ( 0.000000000000000000, 0.000000000000000000, 1.000000000000000000 ) ) ;
#30188 = CARTESIAN_POINT ( 'NONE',  ( -28.16914340538000161, 31.00000000000000355, -57.36152490105312296 ) ) ;
#30189 = ORIENTED_EDGE ( 'NONE', *, *, #39490, .F. ) ;
#30190 = CARTESIAN_POINT ( 'NONE',  ( 0.000000000000000000, 0.000000000000000000, 0.000000000000000000 ) ) ;
#30191 = EDGE_CURVE ( 'NONE', #2577, #6385, #470, .T. ) ;
#30192 = EDGE_LOOP ( 'NONE', ( #21267, #8931, #42706, #18187 ) ) ;
#30193 = EDGE_CURVE ( 'NONE', #6244, #29643, #35682, .T. ) ;
#30194 = CARTESIAN_POINT ( 'NONE',  ( 6.075999999999997847, 0.000000000000000000, 0.000000000000000000 ) ) ;
#30195 = ORIENTED_EDGE ( 'NONE', *, *, #22304, .F. ) ;
#30196 = VECTOR ( 'NONE', #41336, 1000.000000000000000 ) ;
#30197 = CARTESIAN_POINT ( 'NONE',  ( -74.30604906370724905, 40.00000000000000711, -36.76128443489604791 ) ) ;
#30198 = EDGE_CURVE ( 'NONE', #24613, #30077, #12357, .T. ) ;
#30200 = CARTESIAN_POINT ( 'NONE',  ( 0.000000000000000000, -27.24480646643596415, -15.80846360676612505 ) ) ;
#30199 = CARTESIAN_POINT ( 'NONE',  ( 0.000000000000000000, 0.000000000000000000, -6.000000000000000000 ) ) ;
#30201 = DIRECTION ( 'NONE',  ( -1.000000000000000000, -0.000000000000000000, -0.000000000000000000 ) ) ;
#30202 = ORIENTED_EDGE ( 'NONE', *, *, #33507, .T. ) ;
#30203 = CARTESIAN_POINT ( 'NONE',  ( 0.000000000000000000, -101.8011932243944386, -55.61040422519432980 ) ) ;
#30204 = EDGE_LOOP ( 'NONE', ( #13744, #24582 ) ) ;
#30205 =( NAMED_UNIT ( * ) PLANE_ANGLE_UNIT ( ) SI_UNIT ( $, .RADIAN. ) );
#30206 = COLOUR_RGB ( '', 0.08235294, 0.09019608, 0.10196078) ;
#30207 = ORIENTED_EDGE ( 'NONE', *, *, #41973, .F. ) ;
#30208 = CYLINDRICAL_SURFACE ( 'NONE', #284, 59.00000000000000000 ) ;
#30209 = CARTESIAN_POINT ( 'NONE',  ( -54.00384411200708712, 31.00000000000000711, 70.40394205939183792 ) ) ;
#30210 = DIRECTION ( 'NONE',  ( -1.000000000000000000, -0.000000000000000000, -0.000000000000000000 ) ) ;
#30211 = ORIENTED_EDGE ( 'NONE', *, *, #6788, .T. ) ;
#30212 = DIRECTION ( 'NONE',  ( 0.000000000000000000, -0.3681245526846853022, 0.9297764858882484607 ) ) ;
#30213 = EDGE_CURVE ( 'NONE', #19383, #13115, #21552, .T. ) ;
#30214 = ORIENTED_EDGE ( 'NONE', *, *, #18854, .T. ) ;
#30215 = DIRECTION ( 'NONE',  ( -1.000000000000000000, 0.000000000000000000, -0.000000000000000000 ) ) ;
#30216 = AXIS2_PLACEMENT_3D ( 'NONE', #14281, #31294, #14943 ) ;
#30217 = EDGE_CURVE ( 'NONE', #28134, #33321, #27080, .T. ) ;
#30218 = DIRECTION ( 'NONE',  ( 0.000000000000000000, 0.000000000000000000, 1.000000000000000000 ) ) ;
#30219 = DIRECTION ( 'NONE',  ( 0.000000000000000000, 0.9407002666710320149, 0.3392388661180340548 ) ) ;
#30220 = CIRCLE ( 'NONE', #16277, 47.49900000000000233 ) ;
#30221 = LINE ( 'NONE', #13439, #30959 ) ;
#30222 = ORIENTED_EDGE ( 'NONE', *, *, #39441, .F. ) ;
#30223 = DIRECTION ( 'NONE',  ( -1.000000000000000000, -0.000000000000000000, 0.000000000000000000 ) ) ;
#30224 = ORIENTED_EDGE ( 'NONE', *, *, #30757, .F. ) ;
#30225 = CARTESIAN_POINT ( 'NONE',  ( 9.000000000000001776, 101.8011932243955613, -55.61040422519224791 ) ) ;
#30226 = CARTESIAN_POINT ( 'NONE',  ( 17.99999999999999645, -30.71634675606047793, -8.790889055186887902 ) ) ;
#30227 = DIRECTION ( 'NONE',  ( 0.000000000000000000, 0.000000000000000000, 1.000000000000000000 ) ) ;
#30228 = ORIENTED_EDGE ( 'NONE', *, *, #28898, .F. ) ;
#30229 = EDGE_LOOP ( 'NONE', ( #22753, #21308, #19096, #24251 ) ) ;
#30230 = LINE ( 'NONE', #20018, #7735 ) ;
#30231 = EDGE_CURVE ( 'NONE', #16711, #5593, #17937, .T. ) ;
#30232 = FACE_OUTER_BOUND ( 'NONE', #37586, .T. ) ;
#30233 = CARTESIAN_POINT ( 'NONE',  ( 17.99999999999999645, -110.3490479609630910, 38.71798610214488434 ) ) ;
#30234 = CIRCLE ( 'NONE', #38589, 59.00000000000000000 ) ;
#30236 = VERTEX_POINT ( 'NONE', #28546 ) ;
#30235 = CARTESIAN_POINT ( 'NONE',  ( 18.00000000000000355, 0.000000000000000000, 0.000000000000000000 ) ) ;
#30237 = CARTESIAN_POINT ( 'NONE',  ( 32.80084743084299248, 31.00000000000000355, 19.01436317119123842 ) ) ;
#30238 = CARTESIAN_POINT ( 'NONE',  ( 17.99999999999999645, 57.40245293794667703, 96.40140491896650587 ) ) ;
#30239 = VECTOR ( 'NONE', #36706, 1000.000000000000000 ) ;
#30240 = ADVANCED_FACE ( 'NONE', ( #1066 ), #35263, .T. ) ;
#30242 = VERTEX_POINT ( 'NONE', #28958 ) ;
#30241 = CARTESIAN_POINT ( 'NONE',  ( 0.000000000000000000, 114.1529630473454944, -38.59523323561318620 ) ) ;
#30243 = ORIENTED_EDGE ( 'NONE', *, *, #10320, .F. ) ;
#30244 = DIRECTION ( 'NONE',  ( 0.000000000000000000, -0.7865515558026354714, -0.6175246149462008116 ) ) ;
#30245 = DIRECTION ( 'NONE',  ( 0.000000000000000000, 1.411300455031978640E-14, -1.000000000000000000 ) ) ;
#30246 = CARTESIAN_POINT ( 'NONE',  ( 21.53706125533296500, 40.00000000000000000, 43.87245753945351368 ) ) ;
#30247 = AXIS2_PLACEMENT_3D ( 'NONE', #22216, #29578, #5582 ) ;
#30248 = LINE ( 'NONE', #34367, #34700 ) ;
#30249 = CIRCLE ( 'NONE', #19806, 4.000000000000000000 ) ;
#30250 = ADVANCED_FACE ( 'NONE', ( #847, #24258 ), #32009, .T. ) ;
#30251 = CARTESIAN_POINT ( 'NONE',  ( 17.99999999999999645, 0.000000000000000000, 0.000000000000000000 ) ) ;
#30252 = ORIENTED_EDGE ( 'NONE', *, *, #4189, .F. ) ;
#30253 = DIRECTION ( 'NONE',  ( 0.000000000000000000, 0.000000000000000000, -1.000000000000000000 ) ) ;
#30254 = ORIENTED_EDGE ( 'NONE', *, *, #28816, .F. ) ;
#30255 = AXIS2_PLACEMENT_3D ( 'NONE', #2337, #32472, #35940 ) ;
#30256 = DIRECTION ( 'NONE',  ( 1.000000000000000000, 0.000000000000000000, 0.000000000000000000 ) ) ;
#30257 = CYLINDRICAL_SURFACE ( 'NONE', #28985, 51.99999999999999289 ) ;
#30258 = CARTESIAN_POINT ( 'NONE',  ( -15.46676570949300000, 31.00000000000000355, 45.57083133015776610 ) ) ;
#30259 = CYLINDRICAL_SURFACE ( 'NONE', #19763, 12.59999999999999964 ) ;
#30260 = VERTEX_POINT ( 'NONE', #2091 ) ;
#30261 = AXIS2_PLACEMENT_3D ( 'NONE', #3927, #27759, #4364 ) ;
#30262 = AXIS2_PLACEMENT_3D ( 'NONE', #17741, #27979, #41454 ) ;
#30263 = CARTESIAN_POINT ( 'NONE',  ( 17.99999999999999645, -46.12538073176274622, -111.3235835452215952 ) ) ;
#30264 = VERTEX_POINT ( 'NONE', #12383 ) ;
#30265 = CARTESIAN_POINT ( 'NONE',  ( 17.96659372829068246, 40.00000000000000000, -15.76829228678407624 ) ) ;
#30266 = ADVANCED_FACE ( 'NONE', ( #32211 ), #21201, .F. ) ;
#30267 = ORIENTED_EDGE ( 'NONE', *, *, #20915, .F. ) ;
#30268 = ADVANCED_FACE ( 'NONE', ( #34453 ), #31208, .F. ) ;
#30269 = CARTESIAN_POINT ( 'NONE',  ( -4.943662031389838196E-16, -1.828353205453026285E-14, 6.938893903907228378E-15 ) ) ;
#30270 = CARTESIAN_POINT ( 'NONE',  ( -20.82795069773117547, 31.00000000000000355, 77.32795358076221248 ) ) ;
#30271 = CARTESIAN_POINT ( 'NONE',  ( -77.35014290652780744, 40.00000000000000711, 26.14598721591455899 ) ) ;
#30272 = CARTESIAN_POINT ( 'NONE',  ( 17.99999999999999645, 0.000000000000000000, 0.000000000000000000 ) ) ;
#30273 = AXIS2_PLACEMENT_3D ( 'NONE', #14863, #41431, #5654 ) ;
#30274 = TOROIDAL_SURFACE ( 'NONE', #39296, 5.384454397937118664, 0.5155456020628804703 ) ;
#30275 = ORIENTED_EDGE ( 'NONE', *, *, #5423, .F. ) ;
#30276 = ORIENTED_EDGE ( 'NONE', *, *, #14908, .T. ) ;
#30277 = CARTESIAN_POINT ( 'NONE',  ( 18.00000000000000355, -30.93515269692088765, -36.04401931830283701 ) ) ;
#30278 = CIRCLE ( 'NONE', #19835, 116.0000000000000000 ) ;
#30279 = DIRECTION ( 'NONE',  ( 1.000000000000000000, 0.000000000000000000, 0.000000000000000000 ) ) ;
#30280 = AXIS2_PLACEMENT_3D ( 'NONE', #38356, #11781, #1276 ) ;
#30282 = ORIENTED_EDGE ( 'NONE', *, *, #19414, .T. ) ;
#30281 = DIRECTION ( 'NONE',  ( 0.000000000000000000, 0.000000000000000000, 1.000000000000000000 ) ) ;
#30283 = DIRECTION ( 'NONE',  ( -1.000000000000000000, 0.000000000000000000, 0.000000000000000000 ) ) ;
#30284 = ORIENTED_EDGE ( 'NONE', *, *, #18639, .F. ) ;
#30285 = DIRECTION ( 'NONE',  ( -1.000000000000000000, -0.000000000000000000, -0.000000000000000000 ) ) ;
#30286 = EDGE_CURVE ( 'NONE', #7115, #4217, #25486, .T. ) ;
#30287 = CIRCLE ( 'NONE', #1707, 120.5010000000000332 ) ;
#30288 = CARTESIAN_POINT ( 'NONE',  ( -76.41092972884307244, 40.00000000000000711, -25.93877460596726436 ) ) ;
#30289 = FACE_OUTER_BOUND ( 'NONE', #3099, .T. ) ;
#30290 = ORIENTED_EDGE ( 'NONE', *, *, #8473, .F. ) ;
#30291 = FACE_OUTER_BOUND ( 'NONE', #20007, .T. ) ;
#30292 = DIRECTION ( 'NONE',  ( -1.000000000000000000, 0.000000000000000000, 0.000000000000000000 ) ) ;
#30293 = ORIENTED_EDGE ( 'NONE', *, *, #4431, .T. ) ;
#30294 = AXIS2_PLACEMENT_3D ( 'NONE', #34540, #24556, #7926 ) ;
#30295 = ADVANCED_FACE ( 'NONE', ( #35475 ), #15651, .F. ) ;
#30296 = VERTEX_POINT ( 'NONE', #10924 ) ;
#30297 = DIRECTION ( 'NONE',  ( 0.000000000000000000, 0.000000000000000000, 1.000000000000000000 ) ) ;
#30298 = ORIENTED_EDGE ( 'NONE', *, *, #7651, .T. ) ;
#30299 = CARTESIAN_POINT ( 'NONE',  ( -1.587008504153756938, 40.00000000000000000, -24.39691638390478090 ) ) ;
#30300 = DIRECTION ( 'NONE',  ( -1.000000000000000000, -0.000000000000000000, -0.000000000000000000 ) ) ;
#30301 = DIRECTION ( 'NONE',  ( -1.000000000000000000, -0.000000000000000000, -0.000000000000000000 ) ) ;
#30302 = ADVANCED_FACE ( 'NONE', ( #34242 ), #30031, .T. ) ;
#30303 = DIRECTION ( 'NONE',  ( 0.000000000000000000, 0.6382441836448211614, -0.7698339834299053885 ) ) ;
#30304 = DIRECTION ( 'NONE',  ( 0.000000000000000000, 0.000000000000000000, 1.000000000000000000 ) ) ;
#30306 = VERTEX_POINT ( 'NONE', #33288 ) ;
#30305 = VECTOR ( 'NONE', #37681, 1000.000000000000000 ) ;
#30308 = CARTESIAN_POINT ( 'NONE',  ( -6.896599878636567205, -12.98179148322719101, -1.199999999999999956 ) ) ;
#30307 = CARTESIAN_POINT ( 'NONE',  ( 0.000000000000000000, 13.00789606333472470, 115.2683592318615382 ) ) ;
#30309 = CIRCLE ( 'NONE', #24069, 47.49900000000000233 ) ;
#30310 = ORIENTED_EDGE ( 'NONE', *, *, #18023, .T. ) ;
#30311 = VECTOR ( 'NONE', #42794, 1000.000000000000000 ) ;
#30312 = DIRECTION ( 'NONE',  ( -1.000000000000000000, 0.000000000000000000, 0.000000000000000000 ) ) ;
#30313 = DIRECTION ( 'NONE',  ( 0.000000000000000000, -0.9911528310040085277, 0.1327255272837126188 ) ) ;
#30314 = VERTEX_POINT ( 'NONE', #3370 ) ;
#30315 = FACE_OUTER_BOUND ( 'NONE', #26649, .T. ) ;
#30316 = VECTOR ( 'NONE', #18502, 1000.000000000000000 ) ;
#30317 = DIRECTION ( 'NONE',  ( 1.000000000000000000, 0.000000000000000000, -0.000000000000000000 ) ) ;
#30319 = CIRCLE ( 'NONE', #41443, 47.49899999999999523 ) ;
#30318 = FACE_OUTER_BOUND ( 'NONE', #13947, .T. ) ;
#30320 = CARTESIAN_POINT ( 'NONE',  ( -31.81163009274181519, 31.00000000000000355, -64.50738158386226928 ) ) ;
#30321 = EDGE_CURVE ( 'NONE', #19359, #9181, #17265, .T. ) ;
#30322 = ADVANCED_FACE ( 'NONE', ( #6439 ), #9727, .F. ) ;
#30323 = ORIENTED_EDGE ( 'NONE', *, *, #26088, .T. ) ;
#30324 = CARTESIAN_POINT ( 'NONE',  ( -2.829072032612243159, 31.00000000000000355, -44.39959014221899025 ) ) ;
#30325 = EDGE_CURVE ( 'NONE', #10324, #28580, #10146, .T. ) ;
#30326 = EDGE_CURVE ( 'NONE', #5730, #34051, #29592, .T. ) ;
#30327 = CARTESIAN_POINT ( 'NONE',  ( 41.75688748258168914, 40.00000000000000000, -72.32308762158416471 ) ) ;
#30328 = DIRECTION ( 'NONE',  ( 0.000000000000000000, 0.000000000000000000, 1.000000000000000000 ) ) ;
#30329 = CARTESIAN_POINT ( 'NONE',  ( 17.99999999999999645, 73.51007459736430860, 89.73443560133387109 ) ) ;
#30330 = EDGE_LOOP ( 'NONE', ( #8205, #37306, #10975, #15162 ) ) ;
#30331 = CIRCLE ( 'NONE', #37287, 59.00000000000000711 ) ;
#30332 = CARTESIAN_POINT ( 'NONE',  ( -26.14979319748359643, 5.944745455504278020, 2.972870684497277427 ) ) ;
#30333 = AXIS2_PLACEMENT_3D ( 'NONE', #23086, #12809, #36332 ) ;
#30334 = CARTESIAN_POINT ( 'NONE',  ( -1.391697335622809950, -4.043246145443391448, -3.503898532754372575 ) ) ;
#30335 = ORIENTED_EDGE ( 'NONE', *, *, #41954, .F. ) ;
#30336 = CARTESIAN_POINT ( 'NONE',  ( -38.53741714288415210, 40.00000000000000000, -33.79371401777069650 ) ) ;
#30337 = CARTESIAN_POINT ( 'NONE',  ( 0.000000000000000000, 27.43636312076376527, -38.14186064215121519 ) ) ;
#30338 = CARTESIAN_POINT ( 'NONE',  ( 4.000000000000000000, 0.000000000000000000, 0.000000000000000000 ) ) ;
#30339 = CIRCLE ( 'NONE', #20583, 52.00000000000000000 ) ;
#30340 = ORIENTED_EDGE ( 'NONE', *, *, #13562, .T. ) ;
#30341 = DIRECTION ( 'NONE',  ( -1.000000000000000000, 0.000000000000000000, 0.000000000000000000 ) ) ;
#30342 = FACE_OUTER_BOUND ( 'NONE', #38392, .T. ) ;
#30343 = CIRCLE ( 'NONE', #38669, 22.99999999999987921 ) ;
#30344 = VERTEX_POINT ( 'NONE', #12589 ) ;
#30345 = CARTESIAN_POINT ( 'NONE',  ( 17.99999999999999645, 30.01658535635262481, 108.1077105353199102 ) ) ;
#30346 = VERTEX_POINT ( 'NONE', #39374 ) ;
#30347 = ADVANCED_FACE ( 'NONE', ( #9513 ), #32422, .F. ) ;
#30348 = ORIENTED_EDGE ( 'NONE', *, *, #13074, .T. ) ;
#30349 = CARTESIAN_POINT ( 'NONE',  ( -126.0000000000000284, 4.615443851143735910E-16, 0.000000000000000000 ) ) ;
#30350 = CARTESIAN_POINT ( 'NONE',  ( -83.29221842953128885, 31.00000000000000711, -41.19657635674187190 ) ) ;
#30351 = ORIENTED_EDGE ( 'NONE', *, *, #24768, .T. ) ;
#30352 = DIRECTION ( 'NONE',  ( -1.000000000000000000, -0.000000000000000000, -0.000000000000000000 ) ) ;
#30353 = EDGE_CURVE ( 'NONE', #37184, #12223, #29073, .T. ) ;
#30354 = DIRECTION ( 'NONE',  ( -0.000000000000000000, 0.000000000000000000, 1.000000000000000000 ) ) ;
#30355 = CARTESIAN_POINT ( 'NONE',  ( 9.000000000000001776, -19.74581912682874929, 48.10512059033386834 ) ) ;
#30356 = EDGE_LOOP ( 'NONE', ( #34999, #3374, #14655, #14095 ) ) ;
#30357 = CARTESIAN_POINT ( 'NONE',  ( 17.99999999999999645, -68.61497464550663494, 99.05794392877579924 ) ) ;
#30358 = CARTESIAN_POINT ( 'NONE',  ( 0.000000000000000000, 24.72041153920788403, -40.55929306992662475 ) ) ;
#30359 = AXIS2_PLACEMENT_3D ( 'NONE', #34318, #24338, #3545 ) ;
#30361 = DIRECTION ( 'NONE',  ( 0.000000000000000000, 0.000000000000000000, 1.000000000000000000 ) ) ;
#30360 = LINE ( 'NONE', #30154, #14096 ) ;
#30362 = CIRCLE ( 'NONE', #42199, 20.00000000000000711 ) ;
#30363 = CYLINDRICAL_SURFACE ( 'NONE', #30502, 116.0000000000000000 ) ;
#30364 = CIRCLE ( 'NONE', #1061, 120.5010000000000190 ) ;
#30365 = VERTEX_POINT ( 'NONE', #19371 ) ;
#30366 = AXIS2_PLACEMENT_3D ( 'NONE', #37334, #7448, #14233 ) ;
#30367 = DIRECTION ( 'NONE',  ( -0.2140725878556641593, 0.000000000000000000, 0.9768177553304296934 ) ) ;
#30368 = CARTESIAN_POINT ( 'NONE',  ( -39.53383601736616271, 31.00000000000000355, 5.215339288884301538 ) ) ;
#30369 = ORIENTED_EDGE ( 'NONE', *, *, #30060, .T. ) ;
#30370 = FACE_OUTER_BOUND ( 'NONE', #12972, .T. ) ;
#30371 = CIRCLE ( 'NONE', #40082, 120.5010000000000474 ) ;
#30372 = LINE ( 'NONE', #29733, #23115 ) ;
#30373 = ORIENTED_EDGE ( 'NONE', *, *, #17576, .T. ) ;
#30374 = CIRCLE ( 'NONE', #8065, 20.00000000000000355 ) ;
#30375 = EDGE_CURVE ( 'NONE', #6807, #27591, #32537, .T. ) ;
#30376 = EDGE_CURVE ( 'NONE', #1326, #9666, #3144, .T. ) ;
#30377 = CIRCLE ( 'NONE', #12364, 36.00000000000000000 ) ;
#30378 = CARTESIAN_POINT ( 'NONE',  ( 47.90854556226721428, -2.055254544495724645, -74.83297477053847047 ) ) ;
#30379 = CARTESIAN_POINT ( 'NONE',  ( 43.15607885788778475, 40.00000000000000000, -11.56636786368396486 ) ) ;
#30380 = CARTESIAN_POINT ( 'NONE',  ( -16.19793102918200134, 40.00000000000000000, 47.43702525406639836 ) ) ;
#30381 = EDGE_CURVE ( 'NONE', #4296, #36528, #38114, .T. ) ;
#30382 = AXIS2_PLACEMENT_3D ( 'NONE', #2981, #39438, #23131 ) ;
#30383 = ORIENTED_EDGE ( 'NONE', *, *, #32193, .T. ) ;
#30384 = DIRECTION ( 'NONE',  ( -1.000000000000000000, -0.000000000000000000, 0.000000000000000000 ) ) ;
#30385 = LINE ( 'NONE', #23855, #29747 ) ;
#30386 = ADVANCED_FACE ( 'NONE', ( #6017 ), #26532, .T. ) ;
#30387 = FACE_OUTER_BOUND ( 'NONE', #28468, .T. ) ;
#30388 = EDGE_LOOP ( 'NONE', ( #13885, #31584, #12299, #16178 ) ) ;
#30389 = CARTESIAN_POINT ( 'NONE',  ( 21.81281596512078025, 40.00000000000000000, -10.76194779073239083 ) ) ;
#30390 = EDGE_LOOP ( 'NONE', ( #11984, #9233, #27089, #41048, #36719 ) ) ;
#30391 = DIRECTION ( 'NONE',  ( -1.000000000000000000, 0.000000000000000000, 0.000000000000000000 ) ) ;
#30392 = CARTESIAN_POINT ( 'NONE',  ( 1.654252653721905331, 3.663718938583014229, -0.01223254789873410957 ) ) ;
#30393 = EDGE_CURVE ( 'NONE', #9420, #29484, #19343, .T. ) ;
#30394 = ORIENTED_EDGE ( 'NONE', *, *, #9828, .T. ) ;
#30395 = CIRCLE ( 'NONE', #2513, 59.00000000000000000 ) ;
#30396 = FACE_OUTER_BOUND ( 'NONE', #7089, .T. ) ;
#30397 = CARTESIAN_POINT ( 'NONE',  ( 0.000000000000000000, 5.456439917444967591, 112.0647122740742105 ) ) ;
#30398 = VERTEX_POINT ( 'NONE', #9928 ) ;
#30399 = DIRECTION ( 'NONE',  ( 1.000000000000000000, 0.000000000000000000, 0.000000000000000000 ) ) ;
#30400 = AXIS2_PLACEMENT_3D ( 'NONE', #30308, #604, #1031 ) ;
#30401 = ORIENTED_EDGE ( 'NONE', *, *, #29266, .T. ) ;
#30402 = CIRCLE ( 'NONE', #28335, 13.59999999999999964 ) ;
#30403 = DIRECTION ( 'NONE',  ( -3.996523416598930318E-16, 2.658563593772947863E-15, 1.000000000000000000 ) ) ;
#30404 = VECTOR ( 'NONE', #26776, 1000.000000000000000 ) ;
#30405 = ORIENTED_EDGE ( 'NONE', *, *, #10848, .T. ) ;
#30406 = AXIS2_PLACEMENT_3D ( 'NONE', #15161, #41936, #31500 ) ;
#30408 = VERTEX_POINT ( 'NONE', #29178 ) ;
#30407 = CARTESIAN_POINT ( 'NONE',  ( 17.99999999999999645, 95.38615066513983720, 59.07414607872858170 ) ) ;
#30409 = CARTESIAN_POINT ( 'NONE',  ( 7.664524495375376389, 31.00000000000000355, 58.91906827746952757 ) ) ;
#30410 = ORIENTED_EDGE ( 'NONE', *, *, #39039, .T. ) ;
#30411 = CARTESIAN_POINT ( 'NONE',  ( 17.99999999999999645, 76.48293397876373945, -82.08917884620232996 ) ) ;
#30412 = VECTOR ( 'NONE', #11340, 999.9999999999997726 ) ;
#30413 = CIRCLE ( 'NONE', #25548, 120.5010000000000190 ) ;
#30414 = ORIENTED_EDGE ( 'NONE', *, *, #29729, .T. ) ;
#30415 = DIRECTION ( 'NONE',  ( -1.000000000000000000, 0.000000000000000000, 0.000000000000000000 ) ) ;
#30416 = VECTOR ( 'NONE', #142, 1000.000000000000000 ) ;
#30417 = EDGE_LOOP ( 'NONE', ( #39813, #12468, #14812, #21643 ) ) ;
#30418 = CARTESIAN_POINT ( 'NONE',  ( -81.66074000183850501, 40.00000000000000711, -10.87165890510346777 ) ) ;
#30420 = LINE ( 'NONE', #494, #37433 ) ;
#30419 = DIRECTION ( 'NONE',  ( -0.000000000000000000, -0.000000000000000000, 1.000000000000000000 ) ) ;
#30421 = CARTESIAN_POINT ( 'NONE',  ( 0.000000000000000000, 43.55304910509446614, -28.41006711799937889 ) ) ;
#30422 = ORIENTED_EDGE ( 'NONE', *, *, #26647, .T. ) ;
#30423 = CARTESIAN_POINT ( 'NONE',  ( 17.99999999999999645, 80.74349901498510462, -77.90224541347200216 ) ) ;
#30424 = EDGE_LOOP ( 'NONE', ( #34389, #19111, #5948, #12748 ) ) ;
#30425 = DIRECTION ( 'NONE',  ( 1.000000000000000000, 0.000000000000000000, 0.000000000000000000 ) ) ;
#30426 = CARTESIAN_POINT ( 'NONE',  ( 18.00000000000000355, 42.60732521687572927, 19.80331771201673519 ) ) ;
#30427 = CARTESIAN_POINT ( 'NONE',  ( 52.74436945453300041, 31.00000000000000355, 68.73989242669851762 ) ) ;
#30428 = FACE_OUTER_BOUND ( 'NONE', #16455, .T. ) ;
#30429 = CIRCLE ( 'NONE', #22755, 47.49900000000000233 ) ;
#30430 = ORIENTED_EDGE ( 'NONE', *, *, #29827, .T. ) ;
#30431 = EDGE_CURVE ( 'NONE', #11045, #2217, #10239, .T. ) ;
#30432 = CIRCLE ( 'NONE', #11633, 2.041999999999999815 ) ;
#30433 = CIRCLE ( 'NONE', #6029, 59.00000000000000711 ) ;
#30434 = CARTESIAN_POINT ( 'NONE',  ( 18.00000000000000355, 0.000000000000000000, 0.000000000000000000 ) ) ;
#30435 = AXIS2_PLACEMENT_3D ( 'NONE', #39945, #36682, #10076 ) ;
#30436 = VERTEX_POINT ( 'NONE', #19577 ) ;
#30437 = CYLINDRICAL_SURFACE ( 'NONE', #9458, 59.00000000000000000 ) ;
#30438 = CYLINDRICAL_SURFACE ( 'NONE', #13004, 20.00000000000000355 ) ;
#30439 = CARTESIAN_POINT ( 'NONE',  ( -66.59699903142619348, 31.00000000000000711, 75.74378954611491110 ) ) ;
#30440 = AXIS2_PLACEMENT_3D ( 'NONE', #37665, #16991, #10190 ) ;
#30441 = DIRECTION ( 'NONE',  ( 0.000000000000000000, -0.8183027759081742403, 0.5747874102143992747 ) ) ;
#30442 = ADVANCED_FACE ( 'NONE', ( #32849 ), #19155, .F. ) ;
#30443 = ORIENTED_EDGE ( 'NONE', *, *, #29054, .F. ) ;
#30444 = CARTESIAN_POINT ( 'NONE',  ( 0.000000000000000000, 0.000000000000000000, 0.000000000000000000 ) ) ;
#30445 = ORIENTED_EDGE ( 'NONE', *, *, #26346, .F. ) ;
#30446 = CARTESIAN_POINT ( 'NONE',  ( -2.650000000000198419, 150.5000000000013642, 10.00000000000041744 ) ) ;
#30447 = CIRCLE ( 'NONE', #22916, 59.00000000000000711 ) ;
#30448 = EDGE_CURVE ( 'NONE', #34314, #6747, #42443, .T. ) ;
#30449 = DIRECTION ( 'NONE',  ( 0.000000000000000000, 0.000000000000000000, 1.000000000000000000 ) ) ;
#30450 = EDGE_CURVE ( 'NONE', #34755, #2151, #26111, .T. ) ;
#30451 = CARTESIAN_POINT ( 'NONE',  ( 17.99999999999999645, 10.40101730206529140, -120.0512800434970018 ) ) ;
#30452 = ORIENTED_EDGE ( 'NONE', *, *, #26095, .F. ) ;
#30453 = ORIENTED_EDGE ( 'NONE', *, *, #8055, .F. ) ;
#30454 = CARTESIAN_POINT ( 'NONE',  ( 0.000000000000000000, 105.7179949885863266, 37.57629584241859533 ) ) ;
#30455 = CARTESIAN_POINT ( 'NONE',  ( 18.00000000000000355, 0.000000000000000000, 0.000000000000000000 ) ) ;
#30456 = DIRECTION ( 'NONE',  ( -1.000000000000000000, 0.000000000000000000, 0.000000000000000000 ) ) ;
#30458 = EDGE_LOOP ( 'NONE', ( #1554, #34523, #39854, #9851 ) ) ;
#30457 = DIRECTION ( 'NONE',  ( -1.000000000000000000, -0.000000000000000000, -0.000000000000000000 ) ) ;
#30459 = CARTESIAN_POINT ( 'NONE',  ( 30.20675218207096790, 31.00000000000000355, 23.25504409023748309 ) ) ;
#30460 = CYLINDRICAL_SURFACE ( 'NONE', #32096, 10.49999999999998934 ) ;
#30461 = VECTOR ( 'NONE', #31569, 1000.000000000000000 ) ;
#30462 = AXIS2_PLACEMENT_3D ( 'NONE', #17590, #25012, #38255 ) ;
#30463 = VECTOR ( 'NONE', #20836, 1000.000000000000000 ) ;
#30465 = ORIENTED_EDGE ( 'NONE', *, *, #19811, .T. ) ;
#30464 = DIRECTION ( 'NONE',  ( 0.000000000000000000, 0.1590634960190723812, -0.9872683547213445543 ) ) ;
#30466 = ORIENTED_EDGE ( 'NONE', *, *, #34780, .F. ) ;
#30467 = CARTESIAN_POINT ( 'NONE',  ( 18.00000000000000355, 11.90021268425617329, -45.45261810511203038 ) ) ;
#30468 = EDGE_CURVE ( 'NONE', #24680, #239, #23611, .T. ) ;
#30469 = CARTESIAN_POINT ( 'NONE',  ( 17.99999999999999645, 0.000000000000000000, 0.000000000000000000 ) ) ;
#30470 = CARTESIAN_POINT ( 'NONE',  ( 38.48770111205618605, 40.00000000000000000, 44.02435964457617956 ) ) ;
#30471 = CIRCLE ( 'NONE', #34624, 13.59999999999999787 ) ;
#30472 = CIRCLE ( 'NONE', #1164, 4.500000000000002665 ) ;
#30473 = VECTOR ( 'NONE', #17812, 1000.000000000000000 ) ;
#30474 = LINE ( 'NONE', #13680, #36777 ) ;
#30475 = DIRECTION ( 'NONE',  ( -0.000000000000000000, -0.000000000000000000, -1.000000000000000000 ) ) ;
#30476 = VERTEX_POINT ( 'NONE', #23920 ) ;
#30477 = DIRECTION ( 'NONE',  ( -1.000000000000000000, -0.000000000000000000, 0.000000000000000000 ) ) ;
#30479 = ORIENTED_EDGE ( 'NONE', *, *, #9814, .T. ) ;
#30478 = CIRCLE ( 'NONE', #39409, 13.59999999999999787 ) ;
#30480 = DIRECTION ( 'NONE',  ( 0.000000000000000000, 0.000000000000000000, -1.000000000000000000 ) ) ;
#30481 = DIRECTION ( 'NONE',  ( -1.000000000000000000, -0.000000000000000000, 0.000000000000000000 ) ) ;
#30482 = CARTESIAN_POINT ( 'NONE',  ( 32.65420139560029611, 31.00000000000000355, -42.57517516360295673 ) ) ;
#30483 = DIRECTION ( 'NONE',  ( 0.000000000000000000, 0.000000000000000000, 1.000000000000000000 ) ) ;
#30484 = ORIENTED_EDGE ( 'NONE', *, *, #17115, .F. ) ;
#30485 = ADVANCED_FACE ( 'NONE', ( #14307 ), #21101, .F. ) ;
#30486 = PRODUCT ( 'Return Coil Spring', 'Return Coil Spring', '', ( #16612 ) ) ;
#30487 = DIRECTION ( 'NONE',  ( 0.000000000000000000, 0.000000000000000000, 1.000000000000000000 ) ) ;
#30488 = ORIENTED_EDGE ( 'NONE', *, *, #32697, .F. ) ;
#30489 = CARTESIAN_POINT ( 'NONE',  ( -19.76500330823589735, 40.00000000000000000, -5.286999072153966139 ) ) ;
#30490 = ORIENTED_EDGE ( 'NONE', *, *, #3562, .F. ) ;
#30491 = DIRECTION ( 'NONE',  ( 0.000000000000000000, 0.000000000000000000, 1.000000000000000000 ) ) ;
#30492 = FACE_OUTER_BOUND ( 'NONE', #42371, .T. ) ;
#30493 = AXIS2_PLACEMENT_3D ( 'NONE', #22637, #12584, #12377 ) ;
#30494 = CARTESIAN_POINT ( 'NONE',  ( 19.52887458859586545, 31.00000000000000355, -72.48875405280207929 ) ) ;
#30495 = CARTESIAN_POINT ( 'NONE',  ( -4.761419979751499554, 40.00000000000000000, -74.40007767863900767 ) ) ;
#30496 = CARTESIAN_POINT ( 'NONE',  ( 18.00000000000000355, 32.00046193115148441, 34.40241257139697950 ) ) ;
#30497 = AXIS2_PLACEMENT_3D ( 'NONE', #19510, #16887, #30169 ) ;
#30498 = EDGE_CURVE ( 'NONE', #33075, #16446, #30472, .T. ) ;
#30499 = AXIS2_PLACEMENT_3D ( 'NONE', #31629, #25335, #24920 ) ;
#30500 = VERTEX_POINT ( 'NONE', #14103 ) ;
#30501 = FACE_OUTER_BOUND ( 'NONE', #37717, .T. ) ;
#30502 = AXIS2_PLACEMENT_3D ( 'NONE', #23197, #3701, #26661 ) ;
#30503 = ORIENTED_EDGE ( 'NONE', *, *, #29566, .T. ) ;
#30504 = CARTESIAN_POINT ( 'NONE',  ( 9.000000000000001776, 31.08872492059957793, 41.68322423723110148 ) ) ;
#30505 = CIRCLE ( 'NONE', #21484, 2.649999999999987477 ) ;
#30506 = EDGE_CURVE ( 'NONE', #18955, #41139, #11668, .T. ) ;
#30507 = CARTESIAN_POINT ( 'NONE',  ( 8.999999999999998224, 91.65951123222582453, -71.09524597797991419 ) ) ;
#30508 = CIRCLE ( 'NONE', #15216, 65.00000000000000000 ) ;
#30510 = ORIENTED_EDGE ( 'NONE', *, *, #13536, .T. ) ;
#30509 = DIRECTION ( 'NONE',  ( 0.000000000000000000, -0.9826841245925190815, -0.1852887240871243235 ) ) ;
#30511 = DIRECTION ( 'NONE',  ( -1.000000000000000000, 0.000000000000000000, 0.000000000000000000 ) ) ;
#30512 = EDGE_LOOP ( 'NONE', ( #31910, #23722, #26502, #35450 ) ) ;
#30513 = CARTESIAN_POINT ( 'NONE',  ( 0.000000000000000000, 114.1529630473449686, 38.59523323561477781 ) ) ;
#30514 = CARTESIAN_POINT ( 'NONE',  ( 41.75688748258168914, 40.00000000000000000, -72.32308762158416471 ) ) ;
#30515 = FACE_OUTER_BOUND ( 'NONE', #25926, .T. ) ;
#30516 = AXIS2_PLACEMENT_3D ( 'NONE', #28348, #6671, #19390 ) ;
#30517 = ORIENTED_EDGE ( 'NONE', *, *, #29461, .F. ) ;
#30518 = CARTESIAN_POINT ( 'NONE',  ( -31.74999999999999289, -19.99999999999999645, 2.449293598294706119E-15 ) ) ;
#30519 = DIRECTION ( 'NONE',  ( 1.000000000000000000, 0.000000000000000000, 0.000000000000000000 ) ) ;
#30520 = ORIENTED_EDGE ( 'NONE', *, *, #12503, .T. ) ;
#30521 = VERTEX_POINT ( 'NONE', #40660 ) ;
#30522 = CARTESIAN_POINT ( 'NONE',  ( 18.00000000000000355, -15.49408907645141653, -44.90087086784608061 ) ) ;
#30524 = ORIENTED_EDGE ( 'NONE', *, *, #19041, .F. ) ;
#30523 = EDGE_CURVE ( 'NONE', #23479, #3549, #14536, .T. ) ;
#30525 = CARTESIAN_POINT ( 'NONE',  ( 17.33436897218374639, 40.00000000000000000, 22.64673195036553111 ) ) ;
#30526 = CARTESIAN_POINT ( 'NONE',  ( 42.80287614962723808, -34.05525454449571754, 69.29271901957299917 ) ) ;
#30527 = DIRECTION ( 'NONE',  ( -1.000000000000000000, 0.000000000000000000, 0.000000000000000000 ) ) ;
#30528 = EDGE_CURVE ( 'NONE', #27215, #5690, #20438, .T. ) ;
#30529 = VECTOR ( 'NONE', #17109, 1000.000000000000000 ) ;
#30530 = CARTESIAN_POINT ( 'NONE',  ( -19.99999999999999645, 40.00000000000000000, 0.000000000000000000 ) ) ;
#30531 = CARTESIAN_POINT ( 'NONE',  ( 17.99999999999999645, 0.000000000000000000, 0.000000000000000000 ) ) ;
#30532 = VERTEX_POINT ( 'NONE', #41095 ) ;
#30533 = CIRCLE ( 'NONE', #3290, 116.0000000000000000 ) ;
#30535 = CARTESIAN_POINT ( 'NONE',  ( 0.000000000000000000, 0.000000000000000000, 0.000000000000000000 ) ) ;
#30534 = CARTESIAN_POINT ( 'NONE',  ( 17.99999999999999645, 11.49545354908936545, 29.80986809967263085 ) ) ;
#30536 = VERTEX_POINT ( 'NONE', #17392 ) ;
#30537 = VECTOR ( 'NONE', #6409, 1000.000000000000000 ) ;
#30538 = VECTOR ( 'NONE', #2709, 1000.000000000000000 ) ;
#30539 = DIRECTION ( 'NONE',  ( 0.000000000000000000, 0.000000000000000000, 1.000000000000000000 ) ) ;
#30540 = CARTESIAN_POINT ( 'NONE',  ( 13.36968668718156295, 31.00000000000000355, 23.13838826010315941 ) ) ;
#30541 = ORIENTED_EDGE ( 'NONE', *, *, #19036, .F. ) ;
#30542 = FACE_OUTER_BOUND ( 'NONE', #40463, .T. ) ;
#30543 = AXIS2_PLACEMENT_3D ( 'NONE', #13986, #13130, #19894 ) ;
#30544 = FACE_BOUND ( 'NONE', #39865, .T. ) ;
#30545 = CARTESIAN_POINT ( 'NONE',  ( -100.0000000000000568, 31.00000000000000355, 2.687086664288074189E-12 ) ) ;
#30546 = CARTESIAN_POINT ( 'NONE',  ( 64.89583333437747115, 31.00000000000000000, -4.254240043327834009 ) ) ;
#30547 = ORIENTED_EDGE ( 'NONE', *, *, #31955, .F. ) ;
#30548 = CIRCLE ( 'NONE', #6047, 116.0000000000000000 ) ;
#30549 = CARTESIAN_POINT ( 'NONE',  ( -3.331996295684063192, 31.00000000000000355, 49.59602437330212865 ) ) ;
#30550 = CARTESIAN_POINT ( 'NONE',  ( 36.87680687886029318, 40.00000000000000000, -74.81172728975037955 ) ) ;
#30551 = EDGE_CURVE ( 'NONE', #20249, #38954, #40216, .T. ) ;
#30552 = DIRECTION ( 'NONE',  ( 0.000000000000000000, 0.000000000000000000, 1.000000000000000000 ) ) ;
#30553 = CARTESIAN_POINT ( 'NONE',  ( 17.99999999999999645, -120.3696465864705800, -5.624871700597302571 ) ) ;
#30554 = ADVANCED_FACE ( 'NONE', ( #11251 ), #37406, .T. ) ;
#30555 = DIRECTION ( 'NONE',  ( 0.000000000000000000, 0.000000000000000000, 1.000000000000000000 ) ) ;
#30556 = AXIS2_PLACEMENT_3D ( 'NONE', #11406, #4175, #37572 ) ;
#30557 = VECTOR ( 'NONE', #32901, 1000.000000000000000 ) ;
#30558 = ORIENTED_EDGE ( 'NONE', *, *, #42508, .T. ) ;
#30559 = EDGE_CURVE ( 'NONE', #42037, #24522, #36731, .T. ) ;
#30560 = DIRECTION ( 'NONE',  ( -1.000000000000000000, -0.000000000000000000, 0.000000000000000000 ) ) ;
#30561 = FACE_OUTER_BOUND ( 'NONE', #4883, .T. ) ;
#30562 = VECTOR ( 'NONE', #22476, 1000.000000000000000 ) ;
#30563 = EDGE_LOOP ( 'NONE', ( #37650, #31553, #40608, #42121 ) ) ;
#30564 = CARTESIAN_POINT ( 'NONE',  ( 44.56294422764113250, 40.00000000000000000, 34.17917587534974189 ) ) ;
#30565 = CARTESIAN_POINT ( 'NONE',  ( 0.000000000000000000, 0.000000000000000000, 0.000000000000000000 ) ) ;
#30566 = CARTESIAN_POINT ( 'NONE',  ( 4.000000000000000000, 0.7924765000094659007, -0.05906175389889852662 ) ) ;
#30567 = AXIS2_PLACEMENT_3D ( 'NONE', #32784, #36257, #12737 ) ;
#30568 = ORIENTED_EDGE ( 'NONE', *, *, #39324, .T. ) ;
#30569 = DIRECTION ( 'NONE',  ( -1.000000000000000000, 0.000000000000000000, -0.000000000000000000 ) ) ;
#30570 = DIRECTION ( 'NONE',  ( -1.000000000000000000, -0.000000000000000000, -0.000000000000000000 ) ) ;
#30571 = EDGE_LOOP ( 'NONE', ( #42798, #19432, #23657, #40291 ) ) ;
#30572 = DIRECTION ( 'NONE',  ( 0.000000000000000000, 0.000000000000000000, 1.000000000000000000 ) ) ;
#30573 = ORIENTED_EDGE ( 'NONE', *, *, #39319, .F. ) ;
#30574 = FACE_OUTER_BOUND ( 'NONE', #34674, .T. ) ;
#30575 = EDGE_LOOP ( 'NONE', ( #14081, #25275 ) ) ;
#30576 = LINE ( 'NONE', #30140, #36213 ) ;
#30577 = EDGE_CURVE ( 'NONE', #2440, #21485, #12388, .T. ) ;
#30578 = CARTESIAN_POINT ( 'NONE',  ( 0.000000000000000000, 0.2227391519116599106, 46.98410307550730636 ) ) ;
#30579 = ORIENTED_EDGE ( 'NONE', *, *, #31903, .T. ) ;
#30580 = EDGE_CURVE ( 'NONE', #36912, #26654, #11709, .T. ) ;
#30581 = EDGE_CURVE ( 'NONE', #8080, #21257, #3991, .T. ) ;
#30582 = EDGE_CURVE ( 'NONE', #16031, #24063, #30667, .T. ) ;
#30583 = CARTESIAN_POINT ( 'NONE',  ( 0.000000000000000000, 0.000000000000000000, 0.000000000000000000 ) ) ;
#30584 = DIRECTION ( 'NONE',  ( 1.000000000000000000, 0.000000000000000000, 0.000000000000000000 ) ) ;
#30585 = VERTEX_POINT ( 'NONE', #742 ) ;
#30586 = DIRECTION ( 'NONE',  ( -1.000000000000000000, -0.000000000000000000, -0.000000000000000000 ) ) ;
#30587 = DIRECTION ( 'NONE',  ( -1.000000000000000000, -0.000000000000000000, 0.000000000000000000 ) ) ;
#30588 = AXIS2_PLACEMENT_3D ( 'NONE', #27952, #850, #30983 ) ;
#30589 = DIRECTION ( 'NONE',  ( -1.000000000000000000, 0.000000000000000000, -0.000000000000000000 ) ) ;
#30590 = LINE ( 'NONE', #21226, #28431 ) ;
#30591 = CIRCLE ( 'NONE', #29195, 36.00000000000000000 ) ;
#30592 = ORIENTED_EDGE ( 'NONE', *, *, #37248, .T. ) ;
#30593 = CARTESIAN_POINT ( 'NONE',  ( 47.33767018637038859, 8.999999999999985789, 69.39124571101469030 ) ) ;
#30594 = CARTESIAN_POINT ( 'NONE',  ( 9.000000000000001776, -25.18647942089817349, 113.2326863338526977 ) ) ;
#30595 = CARTESIAN_POINT ( 'NONE',  ( -4.929261580875707871, 31.00000000000000355, 37.46659216873931797 ) ) ;
#30596 = ORIENTED_EDGE ( 'NONE', *, *, #36356, .F. ) ;
#30597 = DIRECTION ( 'NONE',  ( -1.000000000000000000, 0.000000000000000000, 0.000000000000000000 ) ) ;
#30598 = CYLINDRICAL_SURFACE ( 'NONE', #4055, 59.00000000000000000 ) ;
#30599 = EDGE_LOOP ( 'NONE', ( #14205, #18584 ) ) ;
#30600 = CYLINDRICAL_SURFACE ( 'NONE', #8056, 51.99999999999999289 ) ;
#30601 = CARTESIAN_POINT ( 'NONE',  ( 45.10416666515585860, 40.00000000000000000, 2.945243104263102651 ) ) ;
#30602 = CARTESIAN_POINT ( 'NONE',  ( -19.32876798325328949, 40.00000000000000000, -39.37500834187648735 ) ) ;
#30603 = EDGE_CURVE ( 'NONE', #21160, #5342, #534, .T. ) ;
#30604 = VERTEX_POINT ( 'NONE', #295 ) ;
#30605 = DIRECTION ( 'NONE',  ( 0.000000000000000000, 0.000000000000000000, 1.000000000000000000 ) ) ;
#30606 = CARTESIAN_POINT ( 'NONE',  ( 17.99999999999999645, 0.000000000000000000, 0.000000000000000000 ) ) ;
#30607 = CARTESIAN_POINT ( 'NONE',  ( 2.500000000000000444, 0.000000000000000000, -5.000000000000000888 ) ) ;
#30608 = LINE ( 'NONE', #40169, #9217 ) ;
#30609 = VERTEX_POINT ( 'NONE', #33494 ) ;
#30610 = CARTESIAN_POINT ( 'NONE',  ( 5.935205493550105516, 40.00000000000000000, -22.18504493031268865 ) ) ;
#30611 = ORIENTED_EDGE ( 'NONE', *, *, #1485, .F. ) ;
#30612 = CARTESIAN_POINT ( 'NONE',  ( 0.000000000000000000, 0.000000000000000000, 0.000000000000000000 ) ) ;
#30613 = CARTESIAN_POINT ( 'NONE',  ( 0.000000000000000000, 88.00363688980654331, -82.31555682352568226 ) ) ;
#30614 = EDGE_LOOP ( 'NONE', ( #19517, #14192 ) ) ;
#30615 = AXIS2_PLACEMENT_3D ( 'NONE', #41866, #1941, #35892 ) ;
#30616 = AXIS2_PLACEMENT_3D ( 'NONE', #9080, #2292, #15653 ) ;
#30617 = CARTESIAN_POINT ( 'NONE',  ( 0.000000000000000000, 30.74337109795219547, -8.695908345466218492 ) ) ;
#30618 = DIRECTION ( 'NONE',  ( -3.892440008040322386E-16, 2.658563593772947863E-15, 1.000000000000000000 ) ) ;
#30619 = VERTEX_POINT ( 'NONE', #16949 ) ;
#30620 = FACE_OUTER_BOUND ( 'NONE', #38707, .T. ) ;
#30621 = ORIENTED_EDGE ( 'NONE', *, *, #43051, .F. ) ;
#30622 = AXIS2_PLACEMENT_3D ( 'NONE', #31675, #14473, #24080 ) ;
#30623 = LINE ( 'NONE', #3732, #8614 ) ;
#30624 = EDGE_LOOP ( 'NONE', ( #29539, #17822, #33711, #26996 ) ) ;
#30626 = ORIENTED_EDGE ( 'NONE', *, *, #12464, .T. ) ;
#30625 = DIRECTION ( 'NONE',  ( 1.000000000000000000, 0.000000000000000000, 0.000000000000000000 ) ) ;
#30627 = ADVANCED_FACE ( 'NONE', ( #30232 ), #10375, .F. ) ;
#30628 = CARTESIAN_POINT ( 'NONE',  ( -9.616483412539254871, 31.00000000000000355, -73.82325415884287168 ) ) ;
#30629 = VERTEX_POINT ( 'NONE', #3785 ) ;
#30630 = CYLINDRICAL_SURFACE ( 'NONE', #21025, 58.99999999999998579 ) ;
#30631 = EDGE_CURVE ( 'NONE', #23227, #10688, #17168, .T. ) ;
#30632 = EDGE_CURVE ( 'NONE', #40062, #38171, #33259, .T. ) ;
#30633 = ADVANCED_FACE ( 'NONE', ( #18703 ), #31965, .T. ) ;
#30634 = ORIENTED_EDGE ( 'NONE', *, *, #12072, .F. ) ;
#30635 = DIRECTION ( 'NONE',  ( 0.000000000000000000, 0.000000000000000000, 1.000000000000000000 ) ) ;
#30636 = EDGE_CURVE ( 'NONE', #214, #33572, #35003, .T. ) ;
#30637 = VERTEX_POINT ( 'NONE', #2043 ) ;
#30638 = CARTESIAN_POINT ( 'NONE',  ( -41.44813913998980581, 40.00000000000000000, -84.33308812960441969 ) ) ;
#30640 = DIRECTION ( 'NONE',  ( -1.000000000000000000, 0.000000000000000000, 0.000000000000000000 ) ) ;
#30639 = FACE_OUTER_BOUND ( 'NONE', #20516, .T. ) ;
#30641 = LINE ( 'NONE', #10344, #32468 ) ;
#30642 = CARTESIAN_POINT ( 'NONE',  ( 0.000000000000000000, 67.32409792376626001, -89.75376489259298296 ) ) ;
#30643 = VERTEX_POINT ( 'NONE', #8594 ) ;
#30644 = CARTESIAN_POINT ( 'NONE',  ( 17.99999999999999645, -111.9370513079672520, 44.61600100275137493 ) ) ;
#30645 = VECTOR ( 'NONE', #20035, 1000.000000000000000 ) ;
#30646 = ORIENTED_EDGE ( 'NONE', *, *, #4094, .T. ) ;
#30647 = DIRECTION ( 'NONE',  ( -1.000000000000000000, -0.000000000000000000, -0.000000000000000000 ) ) ;
#30648 = CARTESIAN_POINT ( 'NONE',  ( -11.47416535668642723, 31.00000000000000355, 87.14428777381637303 ) ) ;
#30649 = AXIS2_PLACEMENT_3D ( 'NONE', #6828, #10327, #29981 ) ;
#30650 = DIRECTION ( 'NONE',  ( -1.000000000000000000, -0.000000000000000000, -0.000000000000000000 ) ) ;
#30651 = ORIENTED_EDGE ( 'NONE', *, *, #19092, .T. ) ;
#30652 = DIRECTION ( 'NONE',  ( -1.000000000000000000, -0.000000000000000000, 0.000000000000000000 ) ) ;
#30653 = VERTEX_POINT ( 'NONE', #14968 ) ;
#30654 = VERTEX_POINT ( 'NONE', #32162 ) ;
#30655 = CARTESIAN_POINT ( 'NONE',  ( 17.99999999999999645, 110.3490479609632615, 38.71798610214565173 ) ) ;
#30656 = DIRECTION ( 'NONE',  ( 0.000000000000000000, 0.000000000000000000, 1.000000000000000000 ) ) ;
#30657 = CARTESIAN_POINT ( 'NONE',  ( 0.000000000000000000, 39.64889472655779201, -33.64468972902464117 ) ) ;
#30658 = ORIENTED_EDGE ( 'NONE', *, *, #31466, .T. ) ;
#30659 = CARTESIAN_POINT ( 'NONE',  ( 5.657435538624008755E-15, 4.615443851143735910E-16, 367.6955262170047263 ) ) ;
#30660 = ORIENTED_EDGE ( 'NONE', *, *, #1705, .F. ) ;
#30661 = CARTESIAN_POINT ( 'NONE',  ( 17.99999999999999645, 31.80866420683990725, 16.59709355804141495 ) ) ;
#30662 = CARTESIAN_POINT ( 'NONE',  ( 0.000000000000000000, 46.19362259308845609, -8.585149169757988474 ) ) ;
#30663 = CARTESIAN_POINT ( 'NONE',  ( 0.000000000000000000, 0.000000000000000000, 3.469446951953614189E-15 ) ) ;
#30664 = ORIENTED_EDGE ( 'NONE', *, *, #16536, .F. ) ;
#30665 = ORIENTED_EDGE ( 'NONE', *, *, #10294, .T. ) ;
#30666 = CARTESIAN_POINT ( 'NONE',  ( 31.80287614962791665, -35.35525454449572180, 69.29271901957253021 ) ) ;
#30667 = LINE ( 'NONE', #40887, #510 ) ;
#30668 = LINE ( 'NONE', #7528, #16018 ) ;
#30669 = AXIS2_PLACEMENT_3D ( 'NONE', #28554, #4747, #18114 ) ;
#30670 = VERTEX_POINT ( 'NONE', #2243 ) ;
#30672 = ORIENTED_EDGE ( 'NONE', *, *, #22081, .T. ) ;
#30671 = FACE_OUTER_BOUND ( 'NONE', #26455, .T. ) ;
#30673 = CIRCLE ( 'NONE', #36905, 58.99999999999999289 ) ;
#30674 = CARTESIAN_POINT ( 'NONE',  ( -20.36888183406315278, 31.00000000000000355, -26.63352584488936614 ) ) ;
#30675 = AXIS2_PLACEMENT_3D ( 'NONE', #39493, #6133, #15557 ) ;
#30676 = DIRECTION ( 'NONE',  ( -1.000000000000000000, -0.000000000000000000, -0.000000000000000000 ) ) ;
#30677 = EDGE_CURVE ( 'NONE', #22222, #8344, #23542, .T. ) ;
#30678 = ADVANCED_FACE ( 'NONE', ( #18053, #34570 ), #1399, .F. ) ;
#30680 = ORIENTED_EDGE ( 'NONE', *, *, #31645, .F. ) ;
#30679 = DIRECTION ( 'NONE',  ( 0.000000000000000000, 0.6736956436465582065, -0.7390089172206580903 ) ) ;
#30681 = EDGE_CURVE ( 'NONE', #30034, #42828, #38693, .T. ) ;
#30682 = ORIENTED_EDGE ( 'NONE', *, *, #19762, .T. ) ;
#30683 = CARTESIAN_POINT ( 'NONE',  ( 18.00000000000000355, -46.87740477351720614, 3.172455868805039270 ) ) ;
#30684 = CARTESIAN_POINT ( 'NONE',  ( -26.81486728383016072, 40.00000000000000000, -46.61672233255473685 ) ) ;
#30685 = DIRECTION ( 'NONE',  ( -1.000000000000000000, -0.000000000000000000, -0.000000000000000000 ) ) ;
#30686 = LINE ( 'NONE', #41112, #10942 ) ;
#30687 = ORIENTED_EDGE ( 'NONE', *, *, #38571, .T. ) ;
#30688 = CARTESIAN_POINT ( 'NONE',  ( 8.999999999999998224, 0.000000000000000000, 0.000000000000000000 ) ) ;
#30689 = EDGE_CURVE ( 'NONE', #4034, #15674, #38147, .T. ) ;
#30690 = VERTEX_POINT ( 'NONE', #11464 ) ;
#30691 = CYLINDRICAL_SURFACE ( 'NONE', #2956, 14.70000000000000107 ) ;
#30692 = DIRECTION ( 'NONE',  ( -1.000000000000000000, -0.000000000000000000, 0.000000000000000000 ) ) ;
#30693 = EDGE_CURVE ( 'NONE', #15576, #9420, #8198, .T. ) ;
#30694 = AXIS2_PLACEMENT_3D ( 'NONE', #41016, #17516, #24706 ) ;
#30695 = CARTESIAN_POINT ( 'NONE',  ( -59.40491426035100631, 31.00000000000000711, 7.833300799371349932 ) ) ;
#30696 = CARTESIAN_POINT ( 'NONE',  ( 6.999999999999995559, 18.77999999999999758, 0.000000000000000000 ) ) ;
#30697 = ORIENTED_EDGE ( 'NONE', *, *, #33140, .T. ) ;
#30698 = CARTESIAN_POINT ( 'NONE',  ( 0.000000000000000000, 0.000000000000000000, 0.000000000000000000 ) ) ;
#30699 = ORIENTED_EDGE ( 'NONE', *, *, #40112, .F. ) ;
#30700 = CARTESIAN_POINT ( 'NONE',  ( -99.14707074559267141, 31.00000000000000711, 13.06922382031732610 ) ) ;
#30701 = VECTOR ( 'NONE', #21636, 1000.000000000000000 ) ;
#30702 = ORIENTED_EDGE ( 'NONE', *, *, #17048, .F. ) ;
#30703 = DIRECTION ( 'NONE',  ( -1.000000000000000000, 0.000000000000000000, -0.000000000000000000 ) ) ;
#30704 = CIRCLE ( 'NONE', #2117, 51.99999999999999289 ) ;
#30705 = DIRECTION ( 'NONE',  ( -1.000000000000000000, -0.000000000000000000, 0.000000000000000000 ) ) ;
#30706 = CARTESIAN_POINT ( 'NONE',  ( 66.15140951848846385, 31.00000000000000000, -38.07406969931856366 ) ) ;
#30707 = CARTESIAN_POINT ( 'NONE',  ( -10.54315780146311532, 40.00000000000000000, 79.17709703063971460 ) ) ;
#30708 = AXIS2_PLACEMENT_3D ( 'NONE', #24023, #13547, #6759 ) ;
#30709 = DIRECTION ( 'NONE',  ( -1.000000000000000000, -0.000000000000000000, -0.000000000000000000 ) ) ;
#30710 = ORIENTED_EDGE ( 'NONE', *, *, #42319, .T. ) ;
#30711 = FACE_OUTER_BOUND ( 'NONE', #28140, .T. ) ;
#30712 = ORIENTED_EDGE ( 'NONE', *, *, #35668, .F. ) ;
#30713 = DIRECTION ( 'NONE',  ( 0.000000000000000000, 0.9714298932647090767, 0.2373266998711185127 ) ) ;
#30714 = CARTESIAN_POINT ( 'NONE',  ( 18.00000000000000355, 0.000000000000000000, 0.000000000000000000 ) ) ;
#30716 = ORIENTED_EDGE ( 'NONE', *, *, #28715, .F. ) ;
#30715 = CARTESIAN_POINT ( 'NONE',  ( 0.000000000000000000, 94.52951811191651643, -67.23221107124801676 ) ) ;
#30717 = CARTESIAN_POINT ( 'NONE',  ( -105.9879088449591933, 31.00000000000000355, -0.3807199291576673361 ) ) ;
#30718 = ORIENTED_EDGE ( 'NONE', *, *, #28300, .F. ) ;
#30719 = DIRECTION ( 'NONE',  ( -0.000000000000000000, -0.000000000000000000, 1.000000000000000000 ) ) ;
#30720 = CARTESIAN_POINT ( 'NONE',  ( 10.81967497908702214, 40.00000000000000000, -82.17651821321413763 ) ) ;
#30721 = DIRECTION ( 'NONE',  ( 0.000000000000000000, 0.000000000000000000, 1.000000000000000000 ) ) ;
#30722 = EDGE_LOOP ( 'NONE', ( #15590, #24869, #22338, #17469 ) ) ;
#30723 = DIRECTION ( 'NONE',  ( 0.000000000000000000, -0.9957341762950354669, 0.09226835946329130234 ) ) ;
#30724 = DIRECTION ( 'NONE',  ( -1.000000000000000000, -0.000000000000000000, -0.000000000000000000 ) ) ;
#30725 = ADVANCED_FACE ( 'NONE', ( #14752 ), #25231, .F. ) ;
#30726 = EDGE_LOOP ( 'NONE', ( #2059, #7284, #24555, #34027 ) ) ;
#30727 = AXIS2_PLACEMENT_3D ( 'NONE', #35287, #4764, #35070 ) ;
#30728 = DIRECTION ( 'NONE',  ( 1.000000000000000000, 0.000000000000000000, 0.000000000000000000 ) ) ;
#30729 = ORIENTED_EDGE ( 'NONE', *, *, #9591, .T. ) ;
#30730 = DIRECTION ( 'NONE',  ( 0.000000000000000000, 0.5877852522924742473, -0.8090169943749465631 ) ) ;
#30732 = ORIENTED_EDGE ( 'NONE', *, *, #22259, .T. ) ;
#30731 = CIRCLE ( 'NONE', #14712, 120.5010000000000190 ) ;
#30733 = PLANE ( 'NONE',  #11596 ) ;
#30734 = AXIS2_PLACEMENT_3D ( 'NONE', #30190, #3739, #3973 ) ;
#30735 = CARTESIAN_POINT ( 'NONE',  ( -8.749793197483594298, -2.055254544495723756, 2.972870684497274762 ) ) ;
#30736 = AXIS2_PLACEMENT_3D ( 'NONE', #12216, #36165, #6279 ) ;
#30737 = CARTESIAN_POINT ( 'NONE',  ( -22.00000000000000000, 31.00000000000000355, 1.283214542831021765 ) ) ;
#30738 = EDGE_LOOP ( 'NONE', ( #5999, #4671, #18871, #15310 ) ) ;
#30740 = LINE ( 'NONE', #7379, #15101 ) ;
#30739 = DIRECTION ( 'NONE',  ( 1.000000000000000000, 0.000000000000000000, 0.000000000000000000 ) ) ;
#30741 = EDGE_CURVE ( 'NONE', #14757, #37436, #25434, .T. ) ;
#30742 = ORIENTED_EDGE ( 'NONE', *, *, #25641, .T. ) ;
#30743 = CIRCLE ( 'NONE', #41174, 20.00000000000000711 ) ;
#30744 = DIRECTION ( 'NONE',  ( -1.807003620809174878E-16, 1.000000000000000000, 0.000000000000000000 ) ) ;
#30745 = EDGE_CURVE ( 'NONE', #13758, #18148, #38477, .T. ) ;
#30746 = CARTESIAN_POINT ( 'NONE',  ( 4.274771203358150196, 31.00000000000000355, -32.49882260841580006 ) ) ;
#30747 = ORIENTED_EDGE ( 'NONE', *, *, #22349, .T. ) ;
#30748 = CARTESIAN_POINT ( 'NONE',  ( -91.96080130434580724, -14.05525454449571043, 14.45886780445738218 ) ) ;
#30749 = CARTESIAN_POINT ( 'NONE',  ( 18.00000000000000355, -25.61928775981012762, -45.25098998563503727 ) ) ;
#30750 = CONTEXT_DEPENDENT_SHAPE_REPRESENTATION ( #38998, #25932 ) ;
#30751 = DIRECTION ( 'NONE',  ( -1.000000000000000000, 0.000000000000000000, 0.000000000000000000 ) ) ;
#30752 = CARTESIAN_POINT ( 'NONE',  ( -65.92798595308768483, 31.00000000000000711, 22.39357416381200849 ) ) ;
#30753 = ORIENTED_EDGE ( 'NONE', *, *, #15773, .F. ) ;
#30754 = CARTESIAN_POINT ( 'NONE',  ( -5.720710522141557952, 31.00000000000000355, -44.01410879003383059 ) ) ;
#30755 = CARTESIAN_POINT ( 'NONE',  ( 65.81435062899562638, 39.99999999999999289, 37.99825742656441463 ) ) ;
#30756 = TOROIDAL_SURFACE ( 'NONE', #27270, 14.91999999999999815, 0.08000000000000020983 ) ;
#30757 = EDGE_CURVE ( 'NONE', #23352, #38293, #30505, .T. ) ;
#30758 = LINE ( 'NONE', #14628, #30412 ) ;
#30759 = CIRCLE ( 'NONE', #2172, 23.00000000000000000 ) ;
#30760 = B_SPLINE_CURVE_WITH_KNOTS ( 'NONE', 3,
 ( #39002, #19839, #32894, #36370, #2970, #19623 ),
 .UNSPECIFIED., .F., .F.,
 ( 4, 2, 4 ),
 ( 0.000000000000000000, 0.0002095117440854730670, 0.0004190234881709461339 ),
 .UNSPECIFIED. ) ;
#30761 = DIRECTION ( 'NONE',  ( 0.000000000000000000, 0.000000000000000000, 1.000000000000000000 ) ) ;
#30762 = ADVANCED_FACE ( 'NONE', ( #21954 ), #5550, .F. ) ;
#30763 = DIRECTION ( 'NONE',  ( 1.000000000000000000, 0.000000000000000000, -0.000000000000000000 ) ) ;
#30765 = VERTEX_POINT ( 'NONE', #42170 ) ;
#30764 = CYLINDRICAL_SURFACE ( 'NONE', #33454, 13.60000000000000142 ) ;
#30766 = CARTESIAN_POINT ( 'NONE',  ( 109.0695705685741075, 106.4195705685767166, 9.999999999999998224 ) ) ;
#30767 = CARTESIAN_POINT ( 'NONE',  ( -3.861362476283256129, -2.629030857716004199, -3.671615880910374941 ) ) ;
#30768 = ORIENTED_EDGE ( 'NONE', *, *, #13677, .F. ) ;
#30769 = CARTESIAN_POINT ( 'NONE',  ( 14.80739997004469366, 40.00000000000000000, 55.25628696611591550 ) ) ;
#30770 = CARTESIAN_POINT ( 'NONE',  ( 9.000000000000001776, 112.8457601792519256, -26.86697618949260402 ) ) ;
#30771 = CARTESIAN_POINT ( 'NONE',  ( 17.99999999999999645, 41.33768078145502756, 104.3046912715542902 ) ) ;
#30772 = VECTOR ( 'NONE', #10106, 1000.000000000000114 ) ;
#30773 = ORIENTED_EDGE ( 'NONE', *, *, #38772, .F. ) ;
#30774 = CARTESIAN_POINT ( 'NONE',  ( 0.000000000000000000, -29.02167576844032482, -108.3790330702172611 ) ) ;
#30775 = CARTESIAN_POINT ( 'NONE',  ( 0.000000000000000000, -105.7179949885865256, -37.57629584241794163 ) ) ;
#30776 = ORIENTED_EDGE ( 'NONE', *, *, #6214, .T. ) ;
#30777 = LINE ( 'NONE', #13781, #535 ) ;
#30778 = EDGE_LOOP ( 'NONE', ( #35219, #21011, #24703, #18127 ) ) ;
#30779 = DIRECTION ( 'NONE',  ( 1.000000000000000000, 0.000000000000000000, 0.000000000000000000 ) ) ;
#30780 = ORIENTED_EDGE ( 'NONE', *, *, #19578, .F. ) ;
#30781 = CARTESIAN_POINT ( 'NONE',  ( 17.99999999999999645, -111.8797445107945236, 8.437727291342365987 ) ) ;
#30782 = CARTESIAN_POINT ( 'NONE',  ( -91.07534658258107640, 31.00000000000000711, 44.76935032132903558 ) ) ;
#30783 = ORIENTED_EDGE ( 'NONE', *, *, #19467, .F. ) ;
#30784 = CYLINDRICAL_SURFACE ( 'NONE', #7267, 59.00000000000000000 ) ;
#30785 = CARTESIAN_POINT ( 'NONE',  ( 18.00000000000001421, 0.000000000000000000, 0.000000000000000000 ) ) ;
#30786 = ORIENTED_EDGE ( 'NONE', *, *, #38400, .F. ) ;
#30787 = FACE_OUTER_BOUND ( 'NONE', #25936, .T. ) ;
#30788 = EDGE_CURVE ( 'NONE', #41859, #8713, #18264, .T. ) ;
#30789 = AXIS2_PLACEMENT_3D ( 'NONE', #24542, #7914, #21274 ) ;
#30790 = AXIS2_PLACEMENT_3D ( 'NONE', #7541, #756, #3590 ) ;
#30791 = CARTESIAN_POINT ( 'NONE',  ( 4.000000000000000000, 2.309401076758497151, -5.000000000000000000 ) ) ;
#30792 = ADVANCED_FACE ( 'NONE', ( #37831 ), #41544, .F. ) ;
#30793 = DIRECTION ( 'NONE',  ( -1.000000000000000000, -0.000000000000000000, -0.000000000000000000 ) ) ;
#30794 = DIRECTION ( 'NONE',  ( 0.000000000000000000, 0.000000000000000000, 1.000000000000000000 ) ) ;
#30795 = ORIENTED_EDGE ( 'NONE', *, *, #20754, .F. ) ;
#30796 = CARTESIAN_POINT ( 'NONE',  ( 36.42574649280170007, -1.000000000000001332, -75.69124779287336935 ) ) ;
#30797 = LINE ( 'NONE', #1095, #32969 ) ;
#30798 = CARTESIAN_POINT ( 'NONE',  ( 38.32544124395173668, 31.00000000000000355, -22.13982348525413002 ) ) ;
#30799 = CIRCLE ( 'NONE', #26622, 36.00000000000000000 ) ;
#30800 = ORIENTED_EDGE ( 'NONE', *, *, #33676, .T. ) ;
#30802 = DIRECTION ( 'NONE',  ( 0.000000000000000000, 0.000000000000000000, 1.000000000000000000 ) ) ;
#30801 = FACE_OUTER_BOUND ( 'NONE', #29137, .T. ) ;
#30803 = CARTESIAN_POINT ( 'NONE',  ( 17.99999999999999645, -19.12429268481792732, 114.4126803693778669 ) ) ;
#30804 = ORIENTED_EDGE ( 'NONE', *, *, #23524, .T. ) ;
#30805 = CYLINDRICAL_SURFACE ( 'NONE', #24100, 2.649999999999985700 ) ;
#30806 = CARTESIAN_POINT ( 'NONE',  ( -45.59965607524345899, 40.00000000000000000, -22.47439267160796916 ) ) ;
#30807 = CARTESIAN_POINT ( 'NONE',  ( 54.79583221321230724, 40.00000000000000000, -14.58025558542526490 ) ) ;
#30808 = DIRECTION ( 'NONE',  ( -1.000000000000000000, 0.000000000000000000, 0.000000000000000000 ) ) ;
#30809 = DIRECTION ( 'NONE',  ( 0.000000000000000000, 0.05322217484217209305, 0.9985826956767622775 ) ) ;
#30810 = EDGE_CURVE ( 'NONE', #12305, #26006, #27710, .T. ) ;
#30811 = EDGE_CURVE ( 'NONE', #34548, #27883, #19740, .T. ) ;
#30812 = DIRECTION ( 'NONE',  ( -1.000000000000000000, -0.000000000000000000, 0.000000000000000000 ) ) ;
#30813 = CARTESIAN_POINT ( 'NONE',  ( 0.000000000000000000, 0.000000000000000000, 0.000000000000000000 ) ) ;
#30814 = AXIS2_PLACEMENT_3D ( 'NONE', #39029, #25563, #22717 ) ;
#30815 = ORIENTED_EDGE ( 'NONE', *, *, #42735, .T. ) ;
#30816 = CARTESIAN_POINT ( 'NONE',  ( -25.30796725786148826, 40.00000000000000000, 14.62256337265529815 ) ) ;
#30817 = ORIENTED_EDGE ( 'NONE', *, *, #28442, .T. ) ;
#30818 = CARTESIAN_POINT ( 'NONE',  ( 17.99999999999999645, -5.822172717930031993, -31.41458249383147106 ) ) ;
#30819 = AXIS2_PLACEMENT_3D ( 'NONE', #15096, #28400, #11589 ) ;
#30820 = LINE ( 'NONE', #3954, #33975 ) ;
#30821 = AXIS2_PLACEMENT_3D ( 'NONE', #25588, #32102, #8531 ) ;
#30822 = EDGE_LOOP ( 'NONE', ( #17248, #31820, #19891, #1515 ) ) ;
#30823 = ADVANCED_FACE ( 'NONE', ( #32369 ), #42599, .T. ) ;
#30824 = DIRECTION ( 'NONE',  ( 1.000000000000000000, -0.000000000000000000, -0.000000000000000000 ) ) ;
#30825 = CARTESIAN_POINT ( 'NONE',  ( 18.00000000000000355, -35.11945359308083425, -38.34871548466050939 ) ) ;
#30826 = ORIENTED_EDGE ( 'NONE', *, *, #38162, .F. ) ;
#30827 = DIRECTION ( 'NONE',  ( 0.000000000000000000, -0.9957341762950334685, -0.09226835946331299332 ) ) ;
#30828 = ORIENTED_EDGE ( 'NONE', *, *, #41735, .F. ) ;
#30829 = CARTESIAN_POINT ( 'NONE',  ( 0.000000000000000000, 11.58753559615485251, 29.77419532459266449 ) ) ;
#30830 = ADVANCED_FACE ( 'NONE', ( #9242 ), #26481, .F. ) ;
#30831 = AXIS2_PLACEMENT_3D ( 'NONE', #27969, #16156, #25775 ) ;
#30832 = ORIENTED_EDGE ( 'NONE', *, *, #38643, .T. ) ;
#30834 = ORIENTED_EDGE ( 'NONE', *, *, #1644, .T. ) ;
#30833 = CYLINDRICAL_SURFACE ( 'NONE', #38317, 36.00000000000000000 ) ;
#30835 = CARTESIAN_POINT ( 'NONE',  ( 61.98103557012429121, 31.00000000000000000, 47.69015029125303329 ) ) ;
#30836 = VERTEX_POINT ( 'NONE', #42809 ) ;
#30837 = CARTESIAN_POINT ( 'NONE',  ( 8.999999999999998224, 78.18175027177430536, 85.69488855493025881 ) ) ;
#30838 = ORIENTED_EDGE ( 'NONE', *, *, #18112, .F. ) ;
#30839 = DIRECTION ( 'NONE',  ( 0.000000000000000000, -0.8443279255020201823, 0.5358267949789886631 ) ) ;
#30840 = EDGE_CURVE ( 'NONE', #9027, #15861, #29790, .T. ) ;
#30841 = ORIENTED_EDGE ( 'NONE', *, *, #12039, .F. ) ;
#30842 = CARTESIAN_POINT ( 'NONE',  ( -70.09526419943651376, 40.00000000000000711, -61.63891210109846241 ) ) ;
#30843 = ADVANCED_FACE ( 'NONE', ( #2454 ), #33002, .F. ) ;
#30845 = CARTESIAN_POINT ( 'NONE',  ( 0.000000000000000000, -5.822172717930484964, 31.41458249383138934 ) ) ;
#30844 = LINE ( 'NONE', #26707, #777 ) ;
#30846 = CARTESIAN_POINT ( 'NONE',  ( 17.99999999999999645, -111.7974656912329436, -9.465682155096647676 ) ) ;
#30847 = CYLINDRICAL_SURFACE ( 'NONE', #22904, 20.00000000000000355 ) ;
#30848 = ORIENTED_EDGE ( 'NONE', *, *, #31497, .T. ) ;
#30849 = AXIS2_PLACEMENT_3D ( 'NONE', #9102, #22457, #5824 ) ;
#30850 = DIRECTION ( 'NONE',  ( -1.000000000000000000, -0.000000000000000000, -0.000000000000000000 ) ) ;
#30851 = DIRECTION ( 'NONE',  ( -1.000000000000000000, 0.000000000000000000, 0.000000000000000000 ) ) ;
#30852 = CARTESIAN_POINT ( 'NONE',  ( -22.78857244739539212, 31.00000000000000355, 85.10612709700112077 ) ) ;
#30853 = EDGE_CURVE ( 'NONE', #40305, #31476, #37883, .T. ) ;
#30854 = LINE ( 'NONE', #28471, #14220 ) ;
#30855 = ORIENTED_EDGE ( 'NONE', *, *, #7928, .F. ) ;
#30856 = CARTESIAN_POINT ( 'NONE',  ( -24.64063138600937464, 40.00000000000000000, 18.85097431370326859 ) ) ;
#30857 = AXIS2_PLACEMENT_3D ( 'NONE', #4313, #21621, #37495 ) ;
#30858 = ORIENTED_EDGE ( 'NONE', *, *, #12608, .F. ) ;
#30859 = EDGE_CURVE ( 'NONE', #8016, #12374, #12805, .T. ) ;
#30860 = VERTEX_POINT ( 'NONE', #25856 ) ;
#30861 = CARTESIAN_POINT ( 'NONE',  ( 0.000000000000000000, 16.86122981692017930, 27.13802899033298388 ) ) ;
#30862 = EDGE_CURVE ( 'NONE', #16394, #17179, #3003, .T. ) ;
#30863 = CARTESIAN_POINT ( 'NONE',  ( 2.500000000000000000, 2.500728763858895382E-16, -2.041999999999999815 ) ) ;
#30864 = EDGE_CURVE ( 'NONE', #28489, #34791, #33234, .T. ) ;
#30865 = ADVANCED_FACE ( 'NONE', ( #22384 ), #5959, .T. ) ;
#30866 = CARTESIAN_POINT ( 'NONE',  ( 18.00000000000000355, 0.000000000000000000, 0.000000000000000000 ) ) ;
#30867 = ORIENTED_EDGE ( 'NONE', *, *, #22492, .T. ) ;
#30868 = DIRECTION ( 'NONE',  ( -3.996523416598930318E-16, 2.658563593772947863E-15, 1.000000000000000000 ) ) ;
#30869 = ORIENTED_EDGE ( 'NONE', *, *, #10568, .T. ) ;
#30870 = DIRECTION ( 'NONE',  ( 1.000000000000000000, -0.000000000000000000, -0.000000000000000000 ) ) ;
#30871 = DIRECTION ( 'NONE',  ( -1.000000000000000000, -0.000000000000000000, -0.000000000000000000 ) ) ;
#30872 = CARTESIAN_POINT ( 'NONE',  ( 18.00000000000000355, -26.17370628620627571, -39.63700417846190049 ) ) ;
#30873 = CARTESIAN_POINT ( 'NONE',  ( 17.99999999999999645, 111.2721026680460596, -14.38025178762657852 ) ) ;
#30874 = EDGE_LOOP ( 'NONE', ( #7902, #11585, #6601, #1129 ) ) ;
#30875 = EDGE_LOOP ( 'NONE', ( #8421, #26844, #36564, #11997 ) ) ;
#30876 = DIRECTION ( 'NONE',  ( 0.000000000000000000, -0.1837495178165570453, -0.9829730996839042279 ) ) ;
#30877 = DIRECTION ( 'NONE',  ( 1.000000000000000000, 0.000000000000000000, 0.000000000000000000 ) ) ;
#30878 = VECTOR ( 'NONE', #11063, 1000.000000000000000 ) ;
#30879 = CARTESIAN_POINT ( 'NONE',  ( 18.00000000000000355, 0.000000000000000000, 0.000000000000000000 ) ) ;
#30880 = EDGE_LOOP ( 'NONE', ( #11840, #32906, #42897, #31290 ) ) ;
#30882 = VERTEX_POINT ( 'NONE', #25655 ) ;
#30881 = CARTESIAN_POINT ( 'NONE',  ( 0.000000000000000000, 0.000000000000000000, 0.000000000000000000 ) ) ;
#30883 = CARTESIAN_POINT ( 'NONE',  ( -28.59133019391535768, 31.00000000000000355, -32.71076623427349261 ) ) ;
#30884 = DIRECTION ( 'NONE',  ( -1.000000000000000000, -0.000000000000000000, 0.000000000000000000 ) ) ;
#30886 = ORIENTED_EDGE ( 'NONE', *, *, #11544, .F. ) ;
#30885 = CARTESIAN_POINT ( 'NONE',  ( 9.000000000000000000, 6.007673836298004666, 35.49518073029998533 ) ) ;
#30887 = VERTEX_POINT ( 'NONE', #38915 ) ;
#30889 = CARTESIAN_POINT ( 'NONE',  ( -61.79211991639481028, 40.00000000000000711, -8.240724169186190551 ) ) ;
#30888 = CIRCLE ( 'NONE', #39912, 13.59999999999999787 ) ;
#30890 = FACE_OUTER_BOUND ( 'NONE', #101, .T. ) ;
#30891 = DIRECTION ( 'NONE',  ( 0.000000000000000000, 0.000000000000000000, 1.000000000000000000 ) ) ;
#30892 = EDGE_LOOP ( 'NONE', ( #38274, #25744, #38140, #32088 ) ) ;
#30893 = CARTESIAN_POINT ( 'NONE',  ( -15.99999999999997691, 40.00000000000000000, 2.500000000000006217 ) ) ;
#30894 = ORIENTED_EDGE ( 'NONE', *, *, #31113, .T. ) ;
#30895 = DIRECTION ( 'NONE',  ( 1.000000000000000000, 0.000000000000000000, 0.000000000000000000 ) ) ;
#30896 = CARTESIAN_POINT ( 'NONE',  ( 17.99999999999999645, 8.827181066047508295, -120.1772519049558667 ) ) ;
#30897 = CARTESIAN_POINT ( 'NONE',  ( 51.69409438402072965, 31.00000000000000355, -17.56033928829605273 ) ) ;
#30898 = CARTESIAN_POINT ( 'NONE',  ( 0.000000000000000000, 23.85344185397347161, -113.5209818126988779 ) ) ;
#30899 = ORIENTED_EDGE ( 'NONE', *, *, #16508, .F. ) ;
#30900 = AXIS2_PLACEMENT_3D ( 'NONE', #28724, #25457, #22199 ) ;
#30901 = DIRECTION ( 'NONE',  ( 1.000000000000000000, 0.000000000000000000, 0.000000000000000000 ) ) ;
#30902 = ORIENTED_EDGE ( 'NONE', *, *, #37737, .F. ) ;
#30903 = CIRCLE ( 'NONE', #9991, 59.00000000000000711 ) ;
#30904 = CARTESIAN_POINT ( 'NONE',  ( -10.31048697494744815, 40.00000000000000000, -30.34325702988586215 ) ) ;
#30905 = VERTEX_POINT ( 'NONE', #32796 ) ;
#30906 = DIRECTION ( 'NONE',  ( -1.000000000000000000, 0.000000000000000000, 0.000000000000000000 ) ) ;
#30907 = DIRECTION ( 'NONE',  ( 1.000000000000000000, 0.000000000000000000, 0.000000000000000000 ) ) ;
#30908 = CARTESIAN_POINT ( 'NONE',  ( 46.16409756963976463, 31.00000000000000355, -59.99419878592187416 ) ) ;
#30909 = CARTESIAN_POINT ( 'NONE',  ( 5.085823974618865151, 40.00000000000000000, 79.40009828669005287 ) ) ;
#30910 = EDGE_CURVE ( 'NONE', #2973, #38690, #14215, .T. ) ;
#30911 = ADVANCED_FACE ( 'NONE', ( #5749 ), #29540, .T. ) ;
#30912 = DIRECTION ( 'NONE',  ( 0.000000000000000000, 0.000000000000000000, 1.000000000000000000 ) ) ;
#30913 = PRESENTATION_LAYER_ASSIGNMENT (  '', '', ( #28161 ) ) ;
#30914 = EDGE_CURVE ( 'NONE', #36853, #10288, #36062, .T. ) ;
#30915 = ORIENTED_EDGE ( 'NONE', *, *, #5983, .F. ) ;
#30916 = DIRECTION ( 'NONE',  ( 0.000000000000000000, 0.8993121301712203586, -0.4373073204588531215 ) ) ;
#30917 = VERTEX_POINT ( 'NONE', #35834 ) ;
#30918 = AXIS2_PLACEMENT_3D ( 'NONE', #35234, #5361, #18730 ) ;
#30919 = DIRECTION ( 'NONE',  ( -1.000000000000000000, -0.000000000000000000, 0.000000000000000000 ) ) ;
#30920 = LINE ( 'NONE', #11085, #24834 ) ;
#30922 = EDGE_LOOP ( 'NONE', ( #29067, #40404, #17343, #63 ) ) ;
#30921 = CARTESIAN_POINT ( 'NONE',  ( 8.999999999999998224, -23.79363200506972476, 27.01597816121638829 ) ) ;
#30923 = CARTESIAN_POINT ( 'NONE',  ( 18.00000000000000355, 36.05989434073656952, -30.12041790338580682 ) ) ;
#30924 = ORIENTED_EDGE ( 'NONE', *, *, #9501, .F. ) ;
#30925 = CARTESIAN_POINT ( 'NONE',  ( 0.000000000000000000, 5.051668046482832750E-16, -4.000000000000000000 ) ) ;
#30926 = CARTESIAN_POINT ( 'NONE',  ( 25.17870271038170316, 40.00000000000000000, 93.97695291299892517 ) ) ;
#30927 = CYLINDRICAL_SURFACE ( 'NONE', #29191, 31.49899999999999878 ) ;
#30928 =( REPRESENTATION_RELATIONSHIP ('NONE','NONE', #330, #37437 ) REPRESENTATION_RELATIONSHIP_WITH_TRANSFORMATION ( #15484 )SHAPE_REPRESENTATION_RELATIONSHIP( ) );
#30929 = ORIENTED_EDGE ( 'NONE', *, *, #21356, .T. ) ;
#30930 = EDGE_CURVE ( 'NONE', #18335, #42499, #2670, .T. ) ;
#30931 = DIRECTION ( 'NONE',  ( 0.000000000000000000, -6.538873467836204094E-15, 1.000000000000000000 ) ) ;
#30932 = CARTESIAN_POINT ( 'NONE',  ( 0.000000000000000000, 31.17727234463695041, 111.7317219465820983 ) ) ;
#30933 = AXIS2_PLACEMENT_3D ( 'NONE', #392, #11121, #17474 ) ;
#30934 = ORIENTED_EDGE ( 'NONE', *, *, #7647, .F. ) ;
#30935 = DIRECTION ( 'NONE',  ( 0.000000000000000000, 0.5963673585384969833, 0.8027116379309670036 ) ) ;
#30936 = CIRCLE ( 'NONE', #42058, 2.500000000000002665 ) ;
#30937 = ORIENTED_EDGE ( 'NONE', *, *, #38202, .T. ) ;
#30938 = CARTESIAN_POINT ( 'NONE',  ( 0.000000000000000000, -23.10276247328017263, -118.2656051737072431 ) ) ;
#30939 = ORIENTED_EDGE ( 'NONE', *, *, #36911, .F. ) ;
#30940 = CARTESIAN_POINT ( 'NONE',  ( -13.43146050690766735, 40.00000000000000000, 27.15249184974963015 ) ) ;
#30941 = CARTESIAN_POINT ( 'NONE',  ( 17.99999999999999645, 34.78944633786279184, 9.257128253673748475 ) ) ;
#30942 = PLANE ( 'NONE',  #7297 ) ;
#30943 = EDGE_CURVE ( 'NONE', #19993, #39452, #15619, .T. ) ;
#30944 = DIRECTION ( 'NONE',  ( 0.000000000000000000, 0.3641605752528230266, -0.9313361774523382097 ) ) ;
#30945 = ORIENTED_EDGE ( 'NONE', *, *, #42095, .T. ) ;
#30948 = FACE_OUTER_BOUND ( 'NONE', #7507, .T. ) ;
#30947 = DIRECTION ( 'NONE',  ( -1.000000000000000000, 0.000000000000000000, 0.000000000000000000 ) ) ;
#30946 = AXIS2_PLACEMENT_3D ( 'NONE', #27526, #447, #17518 ) ;
#30949 = ORIENTED_EDGE ( 'NONE', *, *, #4360, .T. ) ;
#30950 = VECTOR ( 'NONE', #1752, 1000.000000000000000 ) ;
#30951 = DIRECTION ( 'NONE',  ( 1.000000000000000000, -1.373900992973641868E-15, -3.273063162220443081E-16 ) ) ;
#30952 = CARTESIAN_POINT ( 'NONE',  ( 10.28773449565296083, 31.00000000000000355, -20.88174966193524895 ) ) ;
#30953 = VERTEX_POINT ( 'NONE', #40401 ) ;
#30954 = DIRECTION ( 'NONE',  ( 1.000000000000000000, 0.000000000000000000, 0.000000000000000000 ) ) ;
#30955 = CARTESIAN_POINT ( 'NONE',  ( -4.000000000000000000, -7.806255641895631925E-15, -3.142992957459232350 ) ) ;
#30956 = CIRCLE ( 'NONE', #10778, 59.00000000000000000 ) ;
#30957 = DIRECTION ( 'NONE',  ( 0.000000000000000000, -0.3641605752528101481, -0.9313361774523430947 ) ) ;
#30958 = CARTESIAN_POINT ( 'NONE',  ( 48.66231590553977071, 31.00000000000000000, -55.48862040801125062 ) ) ;
#30959 = VECTOR ( 'NONE', #26729, 1000.000000000000000 ) ;
#30960 = ORIENTED_EDGE ( 'NONE', *, *, #6023, .T. ) ;
#30961 = CARTESIAN_POINT ( 'NONE',  ( 45.87644943786595064, 31.00000000000000355, 12.37342411884007376 ) ) ;
#30962 = EDGE_CURVE ( 'NONE', #15150, #3093, #5840, .T. ) ;
#30963 = CARTESIAN_POINT ( 'NONE',  ( 10.12401712103624263, 40.00000000000000000, 76.79210772277129138 ) ) ;
#30964 = PRODUCT_RELATED_PRODUCT_CATEGORY ( 'part', '', ( #19330 ) ) ;
#30965 = AXIS2_PLACEMENT_3D ( 'NONE', #37027, #13287, #10640 ) ;
#30966 = CARTESIAN_POINT ( 'NONE',  ( 142.5000000000000284, 0.000000000000000000, 6.999999999999998224 ) ) ;
#30967 = CARTESIAN_POINT ( 'NONE',  ( 8.999999999999998224, 1.356908653455267209E-15, -11.08000000000000007 ) ) ;
#30968 = CARTESIAN_POINT ( 'NONE',  ( 0.000000000000000000, 0.000000000000000000, 0.000000000000000000 ) ) ;
#30969 = EDGE_CURVE ( 'NONE', #33557, #10195, #30623, .T. ) ;
#30971 = EDGE_LOOP ( 'NONE', ( #5628, #34924, #33008, #10447 ) ) ;
#30970 = DIRECTION ( 'NONE',  ( 0.000000000000000000, 0.000000000000000000, 1.000000000000000000 ) ) ;
#30972 = DIRECTION ( 'NONE',  ( -0.000000000000000000, 5.297542245118643184E-16, 1.000000000000000000 ) ) ;
#30973 = DIRECTION ( 'NONE',  ( -1.000000000000000000, -0.000000000000000000, 0.000000000000000000 ) ) ;
#30974 = EDGE_CURVE ( 'NONE', #3514, #13787, #16297, .T. ) ;
#30975 = ORIENTED_EDGE ( 'NONE', *, *, #3508, .F. ) ;
#30976 = CARTESIAN_POINT ( 'NONE',  ( -22.94860596549062848, 40.00000000000000000, -46.53072237555588231 ) ) ;
#30977 = DIRECTION ( 'NONE',  ( 0.000000000000000000, -1.505387152034110654E-14, -1.000000000000000000 ) ) ;
#30978 = STYLED_ITEM ( 'NONE', ( #38023 ), #20853 ) ;
#30979 = CARTESIAN_POINT ( 'NONE',  ( 42.80287614962723808, -35.35525454449572180, 69.29271901957299917 ) ) ;
#30980 = ORIENTED_EDGE ( 'NONE', *, *, #39579, .T. ) ;
#30981 = EDGE_CURVE ( 'NONE', #3101, #17781, #37357, .T. ) ;
#30982 = CYLINDRICAL_SURFACE ( 'NONE', #18973, 31.49899999999999878 ) ;
#30983 = DIRECTION ( 'NONE',  ( -0.000000000000000000, 0.000000000000000000, 1.000000000000000000 ) ) ;
#30984 = ORIENTED_EDGE ( 'NONE', *, *, #34721, .T. ) ;
#30985 = DIRECTION ( 'NONE',  ( -1.000000000000000000, 0.000000000000000000, 0.000000000000000000 ) ) ;
#30986 = ORIENTED_EDGE ( 'NONE', *, *, #21157, .F. ) ;
#30987 = AXIS2_PLACEMENT_3D ( 'NONE', #18323, #38330, #28557 ) ;
#30988 = CARTESIAN_POINT ( 'NONE',  ( 17.99999999999999645, 59.07817985939141181, -105.0250430397503294 ) ) ;
#30989 = ORIENTED_EDGE ( 'NONE', *, *, #30930, .T. ) ;
#30990 = AXIS2_PLACEMENT_3D ( 'NONE', #42584, #35617, #5534 ) ;
#30991 = DIRECTION ( 'NONE',  ( 0.000000000000000000, 0.000000000000000000, 1.000000000000000000 ) ) ;
#30992 = DIRECTION ( 'NONE',  ( 1.000000000000000000, 0.000000000000000000, 0.000000000000000000 ) ) ;
#30993 = ORIENTED_EDGE ( 'NONE', *, *, #3159, .F. ) ;
#30994 = AXIS2_PLACEMENT_3D ( 'NONE', #7116, #20916, #33524 ) ;
#30995 = CYLINDRICAL_SURFACE ( 'NONE', #1698, 59.00000000000000000 ) ;
#30996 = CARTESIAN_POINT ( 'NONE',  ( 17.99999999999999645, -18.25486108452607681, -25.66996392254292658 ) ) ;
#30997 = ORIENTED_EDGE ( 'NONE', *, *, #35530, .F. ) ;
#30998 = CARTESIAN_POINT ( 'NONE',  ( 17.99999999999999645, -109.1131968883996848, -26.12628443612003437 ) ) ;
#30999 = CIRCLE ( 'NONE', #19878, 116.0000000000000000 ) ;
#31000 = ADVANCED_FACE ( 'NONE', ( #27344 ), #6826, .F. ) ;
#31001 = CARTESIAN_POINT ( 'NONE',  ( 18.00000000000000355, 11.90021268425617329, -45.45261810511203038 ) ) ;
#31002 = DIRECTION ( 'NONE',  ( 0.000000000000000000, 0.1062934856473655570, -0.9943348002101372041 ) ) ;
#31003 = DIRECTION ( 'NONE',  ( 0.000000000000000000, 0.000000000000000000, 1.000000000000000000 ) ) ;
#31004 = VERTEX_POINT ( 'NONE', #37136 ) ;
#31006 = AXIS2_PLACEMENT_3D ( 'NONE', #39140, #6625, #16712 ) ;
#31005 = CARTESIAN_POINT ( 'NONE',  ( -6.914608630413351290E-15, 52.99999999999997868, 3.218651493858380453E-14 ) ) ;
#31007 = CARTESIAN_POINT ( 'NONE',  ( 18.00000000000000355, -42.41764978026621691, 20.20639853260276197 ) ) ;
#31008 = CARTESIAN_POINT ( 'NONE',  ( -38.45388554590046937, 31.00000000000000355, -13.05014827191142679 ) ) ;
#31009 = EDGE_LOOP ( 'NONE', ( #21555, #17733, #10028, #28164 ) ) ;
#31011 = CARTESIAN_POINT ( 'NONE',  ( 17.99999999999999645, -23.85344185397275041, 113.5209818126990200 ) ) ;
#31010 = CARTESIAN_POINT ( 'NONE',  ( 8.999999999999998224, 108.8880088604282008, -39.99251838045848473 ) ) ;
#31012 = CARTESIAN_POINT ( 'NONE',  ( 0.000000000000000000, 34.03046037009303149, -33.13733193845768454 ) ) ;
#31013 = ORIENTED_EDGE ( 'NONE', *, *, #22428, .F. ) ;
#31014 = AXIS2_PLACEMENT_3D ( 'NONE', #16409, #9402, #23189 ) ;
#31015 = DIRECTION ( 'NONE',  ( 0.000000000000000000, 0.000000000000000000, 1.000000000000000000 ) ) ;
#31016 = CARTESIAN_POINT ( 'NONE',  ( 23.58227068755204314, 40.00000000000000000, -47.84673847638903510 ) ) ;
#31017 = AXIS2_PLACEMENT_3D ( 'NONE', #18429, #28013, #41273 ) ;
#31018 = EDGE_CURVE ( 'NONE', #15836, #4507, #32315, .T. ) ;
#31019 = CARTESIAN_POINT ( 'NONE',  ( -45.90931453312558119, 40.00000000000000000, 40.13788153756827626 ) ) ;
#31020 = AXIS2_PLACEMENT_3D ( 'NONE', #4997, #8278, #41853 ) ;
#31021 = CARTESIAN_POINT ( 'NONE',  ( 5.991979999999993645, 0.000000000000000000, 0.000000000000000000 ) ) ;
#31022 = AXIS2_PLACEMENT_3D ( 'NONE', #18129, #15679, #25730 ) ;
#31023 = LINE ( 'NONE', #4607, #41628 ) ;
#31024 = CIRCLE ( 'NONE', #25479, 59.00000000000000711 ) ;
#31025 = DIRECTION ( 'NONE',  ( -1.058513553088275437E-16, -1.000000000000000000, 8.813324511995299047E-17 ) ) ;
#31026 = DIRECTION ( 'NONE',  ( -1.000000000000000000, -0.000000000000000000, -0.000000000000000000 ) ) ;
#31027 = EDGE_CURVE ( 'NONE', #40171, #6447, #42723, .T. ) ;
#31028 = AXIS2_PLACEMENT_3D ( 'NONE', #7028, #20384, #13611 ) ;
#31029 = EDGE_LOOP ( 'NONE', ( #38481, #30394 ) ) ;
#31030 = CARTESIAN_POINT ( 'NONE',  ( 14.35450763783260797, 40.00000000000000000, -18.72194639494853874 ) ) ;
#31031 = ORIENTED_EDGE ( 'NONE', *, *, #28891, .F. ) ;
#31032 = DIRECTION ( 'NONE',  ( -1.000000000000000000, -0.000000000000000000, 0.000000000000000000 ) ) ;
#31033 = CARTESIAN_POINT ( 'NONE',  ( 0.1750025118121568690, 4.719839900820621104, -3.469254087858248070 ) ) ;
#31034 = VERTEX_POINT ( 'NONE', #13839 ) ;
#31035 = DIRECTION ( 'NONE',  ( 1.000000000000000000, 0.000000000000000000, 0.000000000000000000 ) ) ;
#31036 = DIRECTION ( 'NONE',  ( 0.000000000000000000, 0.000000000000000000, 1.000000000000000000 ) ) ;
#31037 = EDGE_CURVE ( 'NONE', #18907, #11646, #36923, .T. ) ;
#31038 = ORIENTED_EDGE ( 'NONE', *, *, #36760, .T. ) ;
#31039 = LINE ( 'NONE', #40399, #30463 ) ;
#31040 = ORIENTED_EDGE ( 'NONE', *, *, #5686, .F. ) ;
#31041 = CIRCLE ( 'NONE', #28263, 59.00000000000001421 ) ;
#31042 = ORIENTED_EDGE ( 'NONE', *, *, #11128, .F. ) ;
#31043 = DIRECTION ( 'NONE',  ( 0.000000000000000000, 0.9957341762950341346, 0.09226835946330566585 ) ) ;
#31044 = CARTESIAN_POINT ( 'NONE',  ( -71.33925323112771366, 31.00000000000000711, 9.290813765106920030 ) ) ;
#31045 = ORIENTED_EDGE ( 'NONE', *, *, #4062, .T. ) ;
#31046 = FACE_OUTER_BOUND ( 'NONE', #2677, .T. ) ;
#31047 = CIRCLE ( 'NONE', #42845, 59.00000000000000711 ) ;
#31048 = AXIS2_PLACEMENT_3D ( 'NONE', #5472, #9163, #18833 ) ;
#31049 = AXIS2_PLACEMENT_3D ( 'NONE', #13800, #20143, #33401 ) ;
#31050 = EDGE_LOOP ( 'NONE', ( #14623, #23569, #7559, #33415 ) ) ;
#31051 = VECTOR ( 'NONE', #25738, 1000.000000000000000 ) ;
#31052 = CARTESIAN_POINT ( 'NONE',  ( 6.075999999999998735, 1.847259681127465666E-15, -15.08402000000000065 ) ) ;
#31053 = ORIENTED_EDGE ( 'NONE', *, *, #18992, .F. ) ;
#31054 = CARTESIAN_POINT ( 'NONE',  ( -61.59955500558135100, 40.00000000000000711, -70.40623950603891501 ) ) ;
#31055 = EDGE_CURVE ( 'NONE', #24215, #9004, #13532, .T. ) ;
#31056 = VECTOR ( 'NONE', #21366, 1000.000000000000000 ) ;
#31057 = VECTOR ( 'NONE', #30481, 1000.000000000000000 ) ;
#31058 = EDGE_CURVE ( 'NONE', #16222, #32693, #36464, .T. ) ;
#31060 = DIRECTION ( 'NONE',  ( -1.000000000000000000, -0.000000000000000000, -0.000000000000000000 ) ) ;
#31059 = LINE ( 'NONE', #1147, #31520 ) ;
#31061 = AXIS2_PLACEMENT_3D ( 'NONE', #31947, #2027, #24782 ) ;
#31062 = CYLINDRICAL_SURFACE ( 'NONE', #41490, 120.5010000000000190 ) ;
#31063 = DIRECTION ( 'NONE',  ( 0.000000000000000000, 0.9213119778704113028, 0.3888241754733244848 ) ) ;
#31064 = ORIENTED_EDGE ( 'NONE', *, *, #11806, .T. ) ;
#31065 = CIRCLE ( 'NONE', #33163, 116.0000000000000000 ) ;
#31066 = CARTESIAN_POINT ( 'NONE',  ( 17.99999999999999645, -106.5605152861907072, 56.26142179985788516 ) ) ;
#31067 = CYLINDRICAL_SURFACE ( 'NONE', #13616, 59.00000000000000000 ) ;
#31068 = CARTESIAN_POINT ( 'NONE',  ( 66.75212336275305347, 31.00000000000000000, -51.21939497476837744 ) ) ;
#31069 = DIRECTION ( 'NONE',  ( 0.000000000000000000, -0.9996456111234528485, 0.02662052143776447166 ) ) ;
#31070 = VERTEX_POINT ( 'NONE', #7245 ) ;
#31071 = EDGE_CURVE ( 'NONE', #33465, #36745, #17726, .T. ) ;
#31072 = CARTESIAN_POINT ( 'NONE',  ( 21.18498618631003438, 40.00000000000000000, 18.62224443192851098 ) ) ;
#31073 = ORIENTED_EDGE ( 'NONE', *, *, #1761, .T. ) ;
#31074 = VERTEX_POINT ( 'NONE', #7034 ) ;
#31075 = CARTESIAN_POINT ( 'NONE',  ( 1.391697335622810172, 4.043246145443375461, -3.503898532754365913 ) ) ;
#31076 = FACE_OUTER_BOUND ( 'NONE', #25452, .T. ) ;
#31078 = CARTESIAN_POINT ( 'NONE',  ( 0.000000000000000000, 34.03046037009255542, 33.13733193845817482 ) ) ;
#31077 = CIRCLE ( 'NONE', #7362, 47.49900000000000233 ) ;
#31079 = DIRECTION ( 'NONE',  ( 1.000000000000000000, 0.000000000000000000, 0.000000000000000000 ) ) ;
#31080 = AXIS2_PLACEMENT_3D ( 'NONE', #25291, #21812, #35057 ) ;
#31081 = AXIS2_PLACEMENT_3D ( 'NONE', #25964, #38595, #12656 ) ;
#31082 = AXIS2_PLACEMENT_3D ( 'NONE', #6634, #33269, #3355 ) ;
#31083 = ADVANCED_FACE ( 'NONE', ( #7475 ), #3965, .F. ) ;
#31084 = EDGE_LOOP ( 'NONE', ( #38262, #5369, #25803, #27441 ) ) ;
#31085 = CARTESIAN_POINT ( 'NONE',  ( 18.00000000000000355, 47.00885577955421013, -6.806061952191806874 ) ) ;
#31086 = EDGE_LOOP ( 'NONE', ( #35996, #34686, #13132, #17000 ) ) ;
#31087 = DIRECTION ( 'NONE',  ( 0.000000000000000000, -0.05322217484218558226, 0.9985826956767615004 ) ) ;
#31088 = DIRECTION ( 'NONE',  ( -1.000000000000000000, -0.000000000000000000, -0.000000000000000000 ) ) ;
#31089 = MECHANICAL_DESIGN_GEOMETRIC_PRESENTATION_REPRESENTATION (  '', ( #20652 ), #17892 ) ;
#31090 = EDGE_CURVE ( 'NONE', #29643, #42975, #17031, .T. ) ;
#31091 = CIRCLE ( 'NONE', #17895, 59.00000000000000711 ) ;
#31092 = DIRECTION ( 'NONE',  ( 0.000000000000000000, 0.000000000000000000, 1.000000000000000000 ) ) ;
#31093 = CIRCLE ( 'NONE', #28065, 59.00000000000000000 ) ;
#31094 = CARTESIAN_POINT ( 'NONE',  ( -20.00000000000000000, 0.000000000000000000, -6.000000000000000000 ) ) ;
#31095 = ORIENTED_EDGE ( 'NONE', *, *, #7212, .T. ) ;
#31096 = VERTEX_POINT ( 'NONE', #33651 ) ;
#31097 = DIRECTION ( 'NONE',  ( 1.000000000000000000, 0.000000000000000000, 0.000000000000000000 ) ) ;
#31098 = CARTESIAN_POINT ( 'NONE',  ( -105.9879088449591933, 31.00000000000000355, -0.3807199291576673361 ) ) ;
#31099 = ORIENTED_EDGE ( 'NONE', *, *, #41032, .T. ) ;
#31101 = ORIENTED_EDGE ( 'NONE', *, *, #35137, .F. ) ;
#31100 = CARTESIAN_POINT ( 'NONE',  ( 17.99999999999999645, 100.6739960869717834, 49.52796165323294986 ) ) ;
#31102 = CARTESIAN_POINT ( 'NONE',  ( -26.44890248586417414, 31.00000000000000355, -34.59877114778963403 ) ) ;
#31103 = DIRECTION ( 'NONE',  ( -1.000000000000000000, -0.000000000000000000, 0.000000000000000000 ) ) ;
#31105 = CYLINDRICAL_SURFACE ( 'NONE', #39359, 20.00000000000000355 ) ;
#31104 = CARTESIAN_POINT ( 'NONE',  ( -4.000000000000000888, 1.563622288139195238, -0.2253451193528307472 ) ) ;
#31106 = EDGE_LOOP ( 'NONE', ( #30697, #27252, #21547, #40917 ) ) ;
#31107 = CARTESIAN_POINT ( 'NONE',  ( -61.89998375879795844, 40.00000000000000711, 3.952486745199417673 ) ) ;
#31108 = EDGE_CURVE ( 'NONE', #17574, #29604, #5129, .T. ) ;
#31109 = ADVANCED_FACE ( 'NONE', ( #903 ), #13400, .F. ) ;
#31110 = AXIS2_PLACEMENT_3D ( 'NONE', #29428, #35937, #32469 ) ;
#31111 = CARTESIAN_POINT ( 'NONE',  ( 2.649999999999993694, -150.5000000000000284, 9.999999999999998224 ) ) ;
#31112 = EDGE_CURVE ( 'NONE', #24346, #41108, #14427, .T. ) ;
#31113 = EDGE_CURVE ( 'NONE', #34568, #14255, #14914, .T. ) ;
#31114 = AXIS2_PLACEMENT_3D ( 'NONE', #2205, #35789, #15565 ) ;
#31115 = DIRECTION ( 'NONE',  ( 0.000000000000000000, 0.000000000000000000, 1.000000000000000000 ) ) ;
#31117 = VERTEX_POINT ( 'NONE', #7852 ) ;
#31116 = AXIS2_PLACEMENT_3D ( 'NONE', #15894, #33074, #29193 ) ;
#31118 = DIRECTION ( 'NONE',  ( 0.000000000000000000, -0.3641605752528102591, -0.9313361774523430947 ) ) ;
#31119 = AXIS2_PLACEMENT_3D ( 'NONE', #13437, #23697, #7070 ) ;
#31120 = EDGE_LOOP ( 'NONE', ( #14911, #2787, #18534, #2022, #34951, #13056 ) ) ;
#31121 = PRESENTATION_STYLE_ASSIGNMENT (( #6947 ) ) ;
#31122 = TOROIDAL_SURFACE ( 'NONE', #12322, 11.08000000000000007, 0.07999999999999934941 ) ;
#31123 = CYLINDRICAL_SURFACE ( 'NONE', #35732, 59.00000000000000000 ) ;
#31124 = CARTESIAN_POINT ( 'NONE',  ( 0.000000000000000000, 0.000000000000000000, 0.000000000000000000 ) ) ;
#31125 = CARTESIAN_POINT ( 'NONE',  ( 54.43714469963884284, 31.00000000000000355, -7.178810421751046000 ) ) ;
#31126 = CYLINDRICAL_SURFACE ( 'NONE', #9318, 36.00000000000000000 ) ;
#31128 = ORIENTED_EDGE ( 'NONE', *, *, #21302, .F. ) ;
#31127 = AXIS2_PLACEMENT_3D ( 'NONE', #32636, #16284, #12581 ) ;
#31130 = VECTOR ( 'NONE', #35958, 1000.000000000000000 ) ;
#31129 = CARTESIAN_POINT ( 'NONE',  ( 17.99999999999999645, -29.03409033315573851, -12.21509719675420946 ) ) ;
#31131 = EDGE_LOOP ( 'NONE', ( #29023, #27997, #33253, #42004 ) ) ;
#31132 = CARTESIAN_POINT ( 'NONE',  ( 26.99674208481366833, 40.00000000000000000, -20.71990538090019029 ) ) ;
#31133 = ORIENTED_EDGE ( 'NONE', *, *, #8859, .F. ) ;
#31134 = DIRECTION ( 'NONE',  ( -1.000000000000000000, 0.000000000000000000, 0.000000000000000000 ) ) ;
#31135 = DIRECTION ( 'NONE',  ( 0.000000000000000000, 0.000000000000000000, 1.000000000000000000 ) ) ;
#31136 = CARTESIAN_POINT ( 'NONE',  ( 44.33290732825512492, 31.00000000000000355, 77.00207852755224280 ) ) ;
#31137 = CARTESIAN_POINT ( 'NONE',  ( -62.56443097449947288, 40.00000000000000000, -55.02758207457567607 ) ) ;
#31138 = CIRCLE ( 'NONE', #29053, 59.00000000000000711 ) ;
#31139 = CARTESIAN_POINT ( 'NONE',  ( -10.00000000000000000, 0.000000000000000000, 0.000000000000000000 ) ) ;
#31140 = ADVANCED_FACE ( 'NONE', ( #13996 ), #7192, .F. ) ;
#31141 = VERTEX_POINT ( 'NONE', #30988 ) ;
#31142 = CYLINDRICAL_SURFACE ( 'NONE', #25632, 31.49899999999999878 ) ;
#31143 = ORIENTED_EDGE ( 'NONE', *, *, #32823, .F. ) ;
#31144 = CARTESIAN_POINT ( 'NONE',  ( -8.920000000000003482, 0.000000000000000000, 0.000000000000000000 ) ) ;
#31145 = LINE ( 'NONE', #24624, #25512 ) ;
#31146 = ADVANCED_FACE ( 'NONE', ( #30574 ), #27742, .T. ) ;
#31147 = AXIS2_PLACEMENT_3D ( 'NONE', #40712, #33540, #9976 ) ;
#31149 = ORIENTED_EDGE ( 'NONE', *, *, #16870, .F. ) ;
#31148 = CARTESIAN_POINT ( 'NONE',  ( -10.00000000000000000, 0.000000000000000000, 0.000000000000000000 ) ) ;
#31150 = CARTESIAN_POINT ( 'NONE',  ( 0.000000000000000000, 0.000000000000000000, 0.000000000000000000 ) ) ;
#31151 = ORIENTED_EDGE ( 'NONE', *, *, #42085, .T. ) ;
#31152 = CARTESIAN_POINT ( 'NONE',  ( -3.974344831685191280E-13, 4.796734841935104576, -3.721909803043223608 ) ) ;
#31153 = VECTOR ( 'NONE', #31511, 1000.000000000000000 ) ;
#31154 = CARTESIAN_POINT ( 'NONE',  ( -45.94448050778635917, 40.00000000000000000, -79.54744219826071117 ) ) ;
#31155 = CYLINDRICAL_SURFACE ( 'NONE', #34057, 31.49899999999999878 ) ;
#31156 = AXIS2_PLACEMENT_3D ( 'NONE', #2380, #9376, #12474 ) ;
#31157 = VECTOR ( 'NONE', #7627, 1000.000000000000000 ) ;
#31158 = ORIENTED_EDGE ( 'NONE', *, *, #11753, .T. ) ;
#31159 = CYLINDRICAL_SURFACE ( 'NONE', #34571, 47.49900000000000233 ) ;
#31160 = CARTESIAN_POINT ( 'NONE',  ( 17.99999999999999645, 84.77518783075197462, -73.49448960231268302 ) ) ;
#31161 = VECTOR ( 'NONE', #21037, 1000.000000000000114 ) ;
#31162 = CYLINDRICAL_SURFACE ( 'NONE', #5956, 59.00000000000000000 ) ;
#31163 = VERTEX_POINT ( 'NONE', #4130 ) ;
#31164 = DIRECTION ( 'NONE',  ( 1.000000000000000000, 0.000000000000000000, 0.000000000000000000 ) ) ;
#31165 = ORIENTED_EDGE ( 'NONE', *, *, #29035, .F. ) ;
#31166 = DIRECTION ( 'NONE',  ( -1.000000000000000000, 0.000000000000000000, 0.000000000000000000 ) ) ;
#31167 = CARTESIAN_POINT ( 'NONE',  ( 9.304442065600174061, 40.00000000000000000, 27.50946418541003169 ) ) ;
#31168 = CYLINDRICAL_SURFACE ( 'NONE', #40448, 10.49999999999999112 ) ;
#31169 = VECTOR ( 'NONE', #20405, 1000.000000000000000 ) ;
#31170 = EDGE_CURVE ( 'NONE', #37998, #8193, #40563, .T. ) ;
#31171 = LINE ( 'NONE', #37482, #9382 ) ;
#31172 = EDGE_CURVE ( 'NONE', #33598, #28845, #13786, .T. ) ;
#31173 = EDGE_CURVE ( 'NONE', #19229, #35630, #31218, .T. ) ;
#31174 = DIRECTION ( 'NONE',  ( 0.000000000000000000, 0.6382441836448211614, -0.7698339834299053885 ) ) ;
#31175 = ORIENTED_EDGE ( 'NONE', *, *, #26316, .T. ) ;
#31177 = DIRECTION ( 'NONE',  ( -1.000000000000000000, -0.000000000000000000, 0.000000000000000000 ) ) ;
#31176 = DIRECTION ( 'NONE',  ( 0.000000000000000000, 0.1062934856473655293, -0.9943348002101370930 ) ) ;
#31178 = EDGE_CURVE ( 'NONE', #433, #29621, #28850, .T. ) ;
#31179 = ORIENTED_EDGE ( 'NONE', *, *, #23388, .F. ) ;
#31180 = CARTESIAN_POINT ( 'NONE',  ( 17.99999999999999645, 115.0622509503832589, 14.72000021165183803 ) ) ;
#31181 = CARTESIAN_POINT ( 'NONE',  ( 7.000000000000009770, -19.59999999999998721, 2.424800662311758221E-15 ) ) ;
#31182 = CARTESIAN_POINT ( 'NONE',  ( -27.97094176822542977, 31.00000000000000355, 9.504947828999611659 ) ) ;
#31184 = ORIENTED_EDGE ( 'NONE', *, *, #8055, .T. ) ;
#31183 = AXIS2_PLACEMENT_3D ( 'NONE', #30026, #13882, #1394 ) ;
#31185 = LINE ( 'NONE', #14176, #24634 ) ;
#31186 = FACE_BOUND ( 'NONE', #32594, .T. ) ;
#31187 = CIRCLE ( 'NONE', #36036, 11.08000000000000007 ) ;
#31188 = AXIS2_PLACEMENT_3D ( 'NONE', #24746, #1780, #37997 ) ;
#31189 = CARTESIAN_POINT ( 'NONE',  ( 4.000000000000000000, 0.000000000000000000, 0.000000000000000000 ) ) ;
#31190 = CARTESIAN_POINT ( 'NONE',  ( -53.76583044639610165, 31.00000000000000355, -61.28633540801820345 ) ) ;
#31191 = ORIENTED_EDGE ( 'NONE', *, *, #7534, .F. ) ;
#31193 = CARTESIAN_POINT ( 'NONE',  ( -42.09738266246711191, 31.00000000000000355, -2.828681863544771691 ) ) ;
#31192 = VECTOR ( 'NONE', #39537, 1000.000000000000000 ) ;
#31194 = VECTOR ( 'NONE', #14022, 1000.000000000000000 ) ;
#31195 = CARTESIAN_POINT ( 'NONE',  ( 68.41617299536980568, 39.99999999999999289, 52.47886963225217016 ) ) ;
#31196 = DIRECTION ( 'NONE',  ( 1.000000000000000000, 0.000000000000000000, 0.000000000000000000 ) ) ;
#31197 = AXIS2_PLACEMENT_3D ( 'NONE', #1903, #34641, #2106 ) ;
#31198 = DIRECTION ( 'NONE',  ( 1.000000000000000000, 0.000000000000000000, 0.000000000000000000 ) ) ;
#31199 = DIRECTION ( 'NONE',  ( 1.000000000000000000, 0.000000000000000000, 0.000000000000000000 ) ) ;
#31200 = ADVANCED_FACE ( 'NONE', ( #17717 ), #7635, .T. ) ;
#31202 = ORIENTED_EDGE ( 'NONE', *, *, #5843, .T. ) ;
#31201 = CYLINDRICAL_SURFACE ( 'NONE', #4161, 59.00000000000000000 ) ;
#31203 = CARTESIAN_POINT ( 'NONE',  ( 0.000000000000000000, -21.56073507908662634, 23.57770962728557151 ) ) ;
#31204 = FACE_OUTER_BOUND ( 'NONE', #18670, .T. ) ;
#31205 = ORIENTED_EDGE ( 'NONE', *, *, #26348, .F. ) ;
#31206 = CARTESIAN_POINT ( 'NONE',  ( -27.38011802910879311, 40.00000000000000000, -55.51905197969063011 ) ) ;
#31207 = CARTESIAN_POINT ( 'NONE',  ( -103.7695705685748635, -106.4195705685759776, 6.999999999999998224 ) ) ;
#31208 = CYLINDRICAL_SURFACE ( 'NONE', #38789, 100.0000000000000000 ) ;
#31209 = ORIENTED_EDGE ( 'NONE', *, *, #34658, .T. ) ;
#31210 = CIRCLE ( 'NONE', #36749, 59.00000000000000000 ) ;
#31211 = CARTESIAN_POINT ( 'NONE',  ( 17.99999999999999645, -28.57802095670097131, 14.28532136906662586 ) ) ;
#31212 = DIRECTION ( 'NONE',  ( -1.000000000000000000, -0.000000000000000000, -0.000000000000000000 ) ) ;
#31213 = EDGE_LOOP ( 'NONE', ( #27852, #32068, #7479, #15243 ) ) ;
#31214 = CARTESIAN_POINT ( 'NONE',  ( 18.00000000000000355, -30.93515269692088765, -36.04401931830283701 ) ) ;
#31215 = ORIENTED_EDGE ( 'NONE', *, *, #37793, .F. ) ;
#31216 = AXIS2_PLACEMENT_3D ( 'NONE', #27274, #24018, #8047 ) ;
#31217 = AXIS2_PLACEMENT_3D ( 'NONE', #37945, #8068, #34685 ) ;
#31218 = LINE ( 'NONE', #20785, #9295 ) ;
#31219 = VERTEX_POINT ( 'NONE', #34463 ) ;
#31220 = AXIS2_PLACEMENT_3D ( 'NONE', #19095, #2233, #15393 ) ;
#31221 = DIRECTION ( 'NONE',  ( 1.000000000000000000, -0.000000000000000000, -0.000000000000000000 ) ) ;
#31222 = DIRECTION ( 'NONE',  ( -1.000000000000000000, 0.000000000000000000, 0.000000000000000000 ) ) ;
#31223 = ORIENTED_EDGE ( 'NONE', *, *, #4702, .T. ) ;
#31224 = VECTOR ( 'NONE', #35995, 1000.000000000000000 ) ;
#31225 = CARTESIAN_POINT ( 'NONE',  ( 0.000000000000000000, 31.80866420683990725, 2.997093558041416195 ) ) ;
#31226 = ADVANCED_FACE ( 'NONE', ( #11150 ), #24481, .F. ) ;
#31227 = DIRECTION ( 'NONE',  ( 0.000000000000000000, -0.9714298932647122964, 0.2373266998711055509 ) ) ;
#31228 = ORIENTED_EDGE ( 'NONE', *, *, #19279, .F. ) ;
#31229 = DIRECTION ( 'NONE',  ( -1.000000000000000000, 0.000000000000000000, -0.000000000000000000 ) ) ;
#31230 = CARTESIAN_POINT ( 'NONE',  ( 17.99999999999999645, -59.07817985938929439, -105.0250430397515089 ) ) ;
#31231 = EDGE_LOOP ( 'NONE', ( #32239, #37815, #30665, #1185 ) ) ;
#31232 = CARTESIAN_POINT ( 'NONE',  ( 17.99999999999999645, 53.40478689619876462, -108.0204598100360016 ) ) ;
#31233 = DIRECTION ( 'NONE',  ( 0.000000000000000000, 0.000000000000000000, 1.000000000000000000 ) ) ;
#31234 = EDGE_LOOP ( 'NONE', ( #4021, #19828 ) ) ;
#31235 = EDGE_CURVE ( 'NONE', #34436, #40375, #10012, .T. ) ;
#31236 = DIRECTION ( 'NONE',  ( 3.009274222672401179E-17, 1.000000000000000000, -2.455023325076604027E-18 ) ) ;
#31237 = LINE ( 'NONE', #1324, #14954 ) ;
#31238 = CARTESIAN_POINT ( 'NONE',  ( 6.892732713553924917, 31.00000000000000355, -52.36990085009771434 ) ) ;
#31239 = ORIENTED_EDGE ( 'NONE', *, *, #712, .F. ) ;
#31241 = DIRECTION ( 'NONE',  ( 0.000000000000000000, -0.9980267284282708928, -0.06279051952932436509 ) ) ;
#31240 = CARTESIAN_POINT ( 'NONE',  ( 17.99999999999999645, 29.68570942776472066, 10.53307442156944873 ) ) ;
#31242 = ADVANCED_FACE ( 'NONE', ( #17945 ), #10485, .F. ) ;
#31243 = CARTESIAN_POINT ( 'NONE',  ( 0.000000000000000000, 73.51007459736430860, 89.73443560133387109 ) ) ;
#31244 = ORIENTED_EDGE ( 'NONE', *, *, #41786, .F. ) ;
#31245 = DIRECTION ( 'NONE',  ( 0.000000000000000000, 0.000000000000000000, 1.000000000000000000 ) ) ;
#31246 = CARTESIAN_POINT ( 'NONE',  ( -12.41726970680908515, 40.00000000000000000, 46.38546114896210071 ) ) ;
#31247 = AXIS2_PLACEMENT_3D ( 'NONE', #32681, #10191, #22914 ) ;
#31248 = CARTESIAN_POINT ( 'NONE',  ( -42.11670055800494339, 40.00000000000000000, -32.42481051986320040 ) ) ;
#31249 = AXIS2_PLACEMENT_3D ( 'NONE', #10774, #38241, #21072 ) ;
#31250 = AXIS2_PLACEMENT_3D ( 'NONE', #16232, #29525, #2865 ) ;
#31251 = CARTESIAN_POINT ( 'NONE',  ( 0.000000000000000000, 103.1672962317651496, 44.09967643725903486 ) ) ;
#31252 = CARTESIAN_POINT ( 'NONE',  ( 17.99999999999999645, -118.8387007424472159, 19.94628303336445185 ) ) ;
#31253 = AXIS2_PLACEMENT_3D ( 'NONE', #32734, #22966, #2817 ) ;
#31254 = DIRECTION ( 'NONE',  ( -0.000000000000000000, -0.000000000000000000, 1.000000000000000000 ) ) ;
#31255 = CARTESIAN_POINT ( 'NONE',  ( -14.11622541012940601, 31.00000000000000355, -16.08312669853564358 ) ) ;
#31256 = VERTEX_POINT ( 'NONE', #17503 ) ;
#31257 = CARTESIAN_POINT ( 'NONE',  ( -37.46020281470095625, 40.00000000000000000, 12.72710441276525017 ) ) ;
#31258 = ORIENTED_EDGE ( 'NONE', *, *, #18974, .F. ) ;
#31259 = CARTESIAN_POINT ( 'NONE',  ( 17.99999999999999645, 0.000000000000000000, 0.000000000000000000 ) ) ;
#31260 = CARTESIAN_POINT ( 'NONE',  ( 18.00000000000000355, 0.000000000000000000, 0.000000000000000000 ) ) ;
#31261 = ORIENTED_EDGE ( 'NONE', *, *, #25443, .T. ) ;
#31262 = FACE_OUTER_BOUND ( 'NONE', #25734, .T. ) ;
#31263 = DIRECTION ( 'NONE',  ( 0.000000000000000000, 0.05322217484217209305, 0.9985826956767622775 ) ) ;
#31264 = EDGE_LOOP ( 'NONE', ( #40665, #14249, #13869, #25047 ) ) ;
#31265 = DIRECTION ( 'NONE',  ( 1.836909530733573776E-16, -1.000000000000000000, 0.000000000000000000 ) ) ;
#31266 = VERTEX_POINT ( 'NONE', #14208 ) ;
#31267 = EDGE_LOOP ( 'NONE', ( #17294, #2521, #15340, #17425 ) ) ;
#31268 = DIRECTION ( 'NONE',  ( -1.000000000000000000, 0.000000000000000000, 0.000000000000000000 ) ) ;
#31269 = CARTESIAN_POINT ( 'NONE',  ( 73.52353481979008620, 31.00000000000000000, 25.08131146961490998 ) ) ;
#31270 = ORIENTED_EDGE ( 'NONE', *, *, #30213, .T. ) ;
#31271 = FACE_OUTER_BOUND ( 'NONE', #40619, .T. ) ;
#31272 = CIRCLE ( 'NONE', #7584, 0.7500000000000006661 ) ;
#31273 = VECTOR ( 'NONE', #33111, 1000.000000000000000 ) ;
#31274 = EDGE_CURVE ( 'NONE', #189, #7533, #38596, .T. ) ;
#31275 = CARTESIAN_POINT ( 'NONE',  ( 17.99999999999999645, 68.61497464550593861, 99.05794392877625398 ) ) ;
#31276 = AXIS2_PLACEMENT_3D ( 'NONE', #20880, #24359, #28047 ) ;
#31277 = ADVANCED_FACE ( 'NONE', ( #37089 ), #11359, .F. ) ;
#31278 = ORIENTED_EDGE ( 'NONE', *, *, #6991, .F. ) ;
#31279 = CARTESIAN_POINT ( 'NONE',  ( 0.000000000000000000, 36.05989434073613609, 30.12041790338630776 ) ) ;
#31280 = ORIENTED_EDGE ( 'NONE', *, *, #33797, .T. ) ;
#31281 = CARTESIAN_POINT ( 'NONE',  ( -88.68107738130200346, 40.00000000000000711, 23.63280646693861087 ) ) ;
#31282 = CARTESIAN_POINT ( 'NONE',  ( 22.71825314374493487, 31.00000000000000355, -13.09499307598873585 ) ) ;
#31284 = DIRECTION ( 'NONE',  ( 1.000000000000000000, 0.000000000000000000, 0.000000000000000000 ) ) ;
#31283 = CARTESIAN_POINT ( 'NONE',  ( 5.991979999999993645, 0.000000000000000000, 0.000000000000000000 ) ) ;
#31285 = CARTESIAN_POINT ( 'NONE',  ( 17.99999999999999645, -83.49789599728842404, 86.88263557826738293 ) ) ;
#31286 = CARTESIAN_POINT ( 'NONE',  ( 17.99999999999999645, -79.94368240339368015, -90.16373242487986772 ) ) ;
#31287 = VERTEX_POINT ( 'NONE', #4803 ) ;
#31288 = EDGE_CURVE ( 'NONE', #18067, #32556, #21932, .T. ) ;
#31289 = SURFACE_STYLE_FILL_AREA ( #41068 ) ;
#31290 = ORIENTED_EDGE ( 'NONE', *, *, #13485, .F. ) ;
#31291 = DIRECTION ( 'NONE',  ( -1.000000000000000000, 0.000000000000000000, -0.000000000000000000 ) ) ;
#31292 = EDGE_CURVE ( 'NONE', #2013, #1401, #13560, .T. ) ;
#31293 = CARTESIAN_POINT ( 'NONE',  ( -96.39699453480135105, 31.00000000000000711, 25.82690913164849889 ) ) ;
#31294 = DIRECTION ( 'NONE',  ( 0.000000000000000000, -1.000000000000000000, 0.000000000000000000 ) ) ;
#31295 = ORIENTED_EDGE ( 'NONE', *, *, #1466, .T. ) ;
#31296 = CARTESIAN_POINT ( 'NONE',  ( 11.19416946702162718, 40.00000000000000000, -22.66942529387992522 ) ) ;
#31297 = ORIENTED_EDGE ( 'NONE', *, *, #36826, .T. ) ;
#31298 = VERTEX_POINT ( 'NONE', #31633 ) ;
#31299 = FACE_OUTER_BOUND ( 'NONE', #30356, .T. ) ;
#31300 = DIRECTION ( 'NONE',  ( 0.000000000000000000, -0.9618256431728160472, -0.2736629900720938813 ) ) ;
#31301 = CIRCLE ( 'NONE', #40327, 2.649999999999985700 ) ;
#31302 = FACE_OUTER_BOUND ( 'NONE', #2575, .T. ) ;
#31303 = AXIS2_PLACEMENT_3D ( 'NONE', #38528, #8650, #38112 ) ;
#31304 = LINE ( 'NONE', #11451, #14278 ) ;
#31305 = CIRCLE ( 'NONE', #12498, 116.0000000000000000 ) ;
#31306 = EDGE_LOOP ( 'NONE', ( #26691, #16764, #19823, #36042 ) ) ;
#31307 = DIRECTION ( 'NONE',  ( 1.000000000000000000, 0.000000000000000000, 0.000000000000000000 ) ) ;
#31308 = EDGE_LOOP ( 'NONE', ( #34947, #40825, #26043, #15884 ) ) ;
#31309 = CARTESIAN_POINT ( 'NONE',  ( 0.000000000000000000, -94.83915810436441518, 59.94836581341558457 ) ) ;
#31310 = ADVANCED_FACE ( 'NONE', ( #9141 ), #38383, .T. ) ;
#31311 = DIRECTION ( 'NONE',  ( -0.000000000000000000, 0.000000000000000000, -1.000000000000000000 ) ) ;
#31312 = EDGE_CURVE ( 'NONE', #25961, #9338, #34905, .T. ) ;
#31313 = CARTESIAN_POINT ( 'NONE',  ( 17.99999999999999645, 0.000000000000000000, 0.000000000000000000 ) ) ;
#31314 = LINE ( 'NONE', #31094, #9431 ) ;
#31315 = ORIENTED_EDGE ( 'NONE', *, *, #5961, .F. ) ;
#31316 = ORIENTED_EDGE ( 'NONE', *, *, #27541, .F. ) ;
#31317 = CYLINDRICAL_SURFACE ( 'NONE', #32866, 120.5010000000000190 ) ;
#31318 = CARTESIAN_POINT ( 'NONE',  ( 104.9999999999993321, -2.293336392629658115E-13, -32.00000000000000000 ) ) ;
#31319 = ORIENTED_EDGE ( 'NONE', *, *, #21298, .T. ) ;
#31321 = ORIENTED_EDGE ( 'NONE', *, *, #940, .F. ) ;
#31320 = DIRECTION ( 'NONE',  ( 0.000000000000000000, 0.9618256431728180456, 0.2736629900720866093 ) ) ;
#31322 = CARTESIAN_POINT ( 'NONE',  ( -30.82418422902937039, 31.00000000000000355, 26.94311707098126618 ) ) ;
#31323 = DIRECTION ( 'NONE',  ( -1.000000000000000000, 0.000000000000000000, 0.000000000000000000 ) ) ;
#31324 = EDGE_CURVE ( 'NONE', #4914, #25878, #8647, .T. ) ;
#31326 = CARTESIAN_POINT ( 'NONE',  ( 18.00000000000000355, 0.000000000000000000, 0.000000000000000000 ) ) ;
#31325 = DIRECTION ( 'NONE',  ( -1.000000000000000000, -0.000000000000000000, -0.000000000000000000 ) ) ;
#31327 = ORIENTED_EDGE ( 'NONE', *, *, #10934, .T. ) ;
#31328 = DIRECTION ( 'NONE',  ( 0.000000000000000000, 0.000000000000000000, 1.000000000000000000 ) ) ;
#31329 = CARTESIAN_POINT ( 'NONE',  ( -59.29355402628473826, 40.00000000000000000, -20.23837177251483155 ) ) ;
#31330 = TOROIDAL_SURFACE ( 'NONE', #25863, 19.11697999999999809, 0.08401999999999801294 ) ;
#31331 = CIRCLE ( 'NONE', #29935, 120.5010000000000190 ) ;
#31332 = DIRECTION ( 'NONE',  ( 0.000000000000000000, 0.000000000000000000, 1.000000000000000000 ) ) ;
#31333 = CARTESIAN_POINT ( 'NONE',  ( 0.000000000000000000, -120.3696465864706369, 5.624871700595674540 ) ) ;
#31334 = ORIENTED_EDGE ( 'NONE', *, *, #34598, .F. ) ;
#31335 = CIRCLE ( 'NONE', #6923, 120.5010000000000474 ) ;
#31336 = LINE ( 'NONE', #11927, #36268 ) ;
#31337 = VERTEX_POINT ( 'NONE', #38588 ) ;
#31338 = EDGE_CURVE ( 'NONE', #17494, #19198, #11474, .T. ) ;
#31339 = SURFACE_STYLE_FILL_AREA ( #7975 ) ;
#31340 = CARTESIAN_POINT ( 'NONE',  ( 2.027755760259328333E-13, -150.5000000000013642, 9.999999999999586109 ) ) ;
#31341 = LINE ( 'NONE', #41570, #21391 ) ;
#31342 = ADVANCED_FACE ( 'NONE', ( #15719 ), #5860, .T. ) ;
#31343 = CARTESIAN_POINT ( 'NONE',  ( -52.79687664379660816, 31.00000000000000355, -30.48099731442381710 ) ) ;
#31344 = CARTESIAN_POINT ( 'NONE',  ( -30.61154013076160751, 17.11489954122029289, 25.77968906985393716 ) ) ;
#31345 = ORIENTED_EDGE ( 'NONE', *, *, #24149, .F. ) ;
#31346 = SURFACE_STYLE_USAGE ( .BOTH. , #11936 ) ;
#31347 = ORIENTED_EDGE ( 'NONE', *, *, #1679, .T. ) ;
#31348 = CARTESIAN_POINT ( 'NONE',  ( 8.999999999999998224, -54.09091620264791089, 102.6166301549515936 ) ) ;
#31349 = LINE ( 'NONE', #7777, #17922 ) ;
#31350 = CARTESIAN_POINT ( 'NONE',  ( 86.62806645044915399, 31.00000000000000000, 11.52843970785434990 ) ) ;
#31351 = CARTESIAN_POINT ( 'NONE',  ( -11.85673204381699364, 40.00000000000000000, 89.11174773313419450 ) ) ;
#31352 = CYLINDRICAL_SURFACE ( 'NONE', #11154, 120.5010000000000190 ) ;
#31353 = VERTEX_POINT ( 'NONE', #28162 ) ;
#31354 = CARTESIAN_POINT ( 'NONE',  ( -31.74999999999999289, -19.19999999999999574, 2.351321854362917684E-15 ) ) ;
#31355 = ORIENTED_EDGE ( 'NONE', *, *, #23394, .T. ) ;
#31356 = AXIS2_PLACEMENT_3D ( 'NONE', #31949, #15589, #21942 ) ;
#31357 = CARTESIAN_POINT ( 'NONE',  ( 17.99999999999999645, 30.74337109795208178, 8.695908345466650147 ) ) ;
#31358 = CARTESIAN_POINT ( 'NONE',  ( -12.55910585664918422, 0.7408941433508191565, 0.000000000000000000 ) ) ;
#31360 = EDGE_CURVE ( 'NONE', #32669, #10688, #20522, .T. ) ;
#31359 = AXIS2_PLACEMENT_3D ( 'NONE', #36220, #19688, #13998 ) ;
#31361 = EDGE_CURVE ( 'NONE', #13665, #19271, #5226, .T. ) ;
#31363 = ORIENTED_EDGE ( 'NONE', *, *, #28226, .T. ) ;
#31362 = CARTESIAN_POINT ( 'NONE',  ( 0.000000000000000000, 7.749090474611950441, -30.53094492177204700 ) ) ;
#31364 = CARTESIAN_POINT ( 'NONE',  ( 17.99999999999999645, 98.69720329640956891, 60.94966826379944536 ) ) ;
#31365 = ORIENTED_EDGE ( 'NONE', *, *, #14964, .T. ) ;
#31366 = FACE_OUTER_BOUND ( 'NONE', #30388, .T. ) ;
#31367 = CARTESIAN_POINT ( 'NONE',  ( 89.65113856817994531, 39.99999999999999289, -30.44896562292877462 ) ) ;
#31368 = CARTESIAN_POINT ( 'NONE',  ( 17.99999999999999645, -21.55123232222391394, -118.5581519187674360 ) ) ;
#31369 = VERTEX_POINT ( 'NONE', #2153 ) ;
#31370 = DIRECTION ( 'NONE',  ( 0.000000000000000000, 0.000000000000000000, 1.000000000000000000 ) ) ;
#31371 = DIRECTION ( 'NONE',  ( -0.9247238835424298475, -2.016449031586420221E-16, -0.3806385939525924744 ) ) ;
#31372 = EDGE_CURVE ( 'NONE', #36216, #8904, #15511, .T. ) ;
#31374 = FACE_OUTER_BOUND ( 'NONE', #11494, .T. ) ;
#31373 = CARTESIAN_POINT ( 'NONE',  ( 0.000000000000000000, 0.000000000000000000, 0.000000000000000000 ) ) ;
#31375 = EDGE_LOOP ( 'NONE', ( #31811, #33543, #12268, #18820 ) ) ;
#31376 = EDGE_CURVE ( 'NONE', #8384, #2260, #28880, .T. ) ;
#31377 = CARTESIAN_POINT ( 'NONE',  ( 0.000000000000000000, 47.49120266317495265, -0.8606222198177008176 ) ) ;
#31378 = ORIENTED_EDGE ( 'NONE', *, *, #4262, .F. ) ;
#31379 = DIRECTION ( 'NONE',  ( 1.000000000000000000, 0.000000000000000000, 0.000000000000000000 ) ) ;
#31380 = CARTESIAN_POINT ( 'NONE',  ( 2.319640971205140900, 40.00000000000000000, -34.59922639972668890 ) ) ;
#31381 = DIRECTION ( 'NONE',  ( 3.009274222672345096E-17, 1.000000000000000000, -2.455023325076454960E-18 ) ) ;
#31382 = DIRECTION ( 'NONE',  ( 0.000000000000000000, 0.000000000000000000, 1.000000000000000000 ) ) ;
#31383 = CARTESIAN_POINT ( 'NONE',  ( 17.99999999999999645, 0.000000000000000000, 0.000000000000000000 ) ) ;
#31384 = EDGE_LOOP ( 'NONE', ( #10189, #15897, #25923, #2887 ) ) ;
#31386 = FACE_OUTER_BOUND ( 'NONE', #29247, .T. ) ;
#31385 = CARTESIAN_POINT ( 'NONE',  ( 9.000000000000001776, -110.8621702203451065, 34.14058016547500785 ) ) ;
#31387 = EDGE_LOOP ( 'NONE', ( #37455, #9912, #28000, #15718 ) ) ;
#31388 = EDGE_CURVE ( 'NONE', #32231, #22539, #1729, .T. ) ;
#31389 = AXIS2_PLACEMENT_3D ( 'NONE', #18357, #1499, #41196 ) ;
#31390 = DIRECTION ( 'NONE',  ( -1.000000000000000000, 0.000000000000000000, 0.000000000000000000 ) ) ;
#31391 = LINE ( 'NONE', #35291, #18553 ) ;
#31392 = EDGE_CURVE ( 'NONE', #31117, #35437, #8938, .T. ) ;
#31394 = CARTESIAN_POINT ( 'NONE',  ( 19.04566582976364941, 31.00000000000000355, -14.62000746238684989 ) ) ;
#31393 = AXIS2_PLACEMENT_3D ( 'NONE', #8503, #39223, #18813 ) ;
#31395 = VERTEX_POINT ( 'NONE', #22286 ) ;
#31396 = CARTESIAN_POINT ( 'NONE',  ( 0.000000000000000000, 0.000000000000000000, 0.000000000000000000 ) ) ;
#31397 = AXIS2_PLACEMENT_3D ( 'NONE', #24678, #21639, #8054 ) ;
#31398 = FACE_OUTER_BOUND ( 'NONE', #29503, .T. ) ;
#31399 = CARTESIAN_POINT ( 'NONE',  ( 0.000000000000000000, 0.000000000000000000, 0.000000000000000000 ) ) ;
#31400 = CARTESIAN_POINT ( 'NONE',  ( -80.10416666582359824, 31.00000000000000711, -5.235987747607834031 ) ) ;
#31401 = ADVANCED_FACE ( 'NONE', ( #1514 ), #8501, .T. ) ;
#31402 = EDGE_LOOP ( 'NONE', ( #42377, #36696, #20865, #8848 ) ) ;
#31403 = CARTESIAN_POINT ( 'NONE',  ( 46.08863070263671347, 31.00000000000000355, 35.47900410130831972 ) ) ;
#31404 = CARTESIAN_POINT ( 'NONE',  ( -12.08748825390017068, 40.00000000000000000, -91.69541640458645304 ) ) ;
#31405 = ORIENTED_EDGE ( 'NONE', *, *, #3771, .T. ) ;
#31406 = FACE_OUTER_BOUND ( 'NONE', #40408, .T. ) ;
#31407 = ADVANCED_FACE ( 'NONE', ( #39015 ), #28391, .T. ) ;
#31408 = CIRCLE ( 'NONE', #9778, 47.49900000000000944 ) ;
#31409 = CARTESIAN_POINT ( 'NONE',  ( 0.000000000000000000, -90.81729652456118629, -72.16798910853708549 ) ) ;
#31410 = DIRECTION ( 'NONE',  ( 0.000000000000000000, 0.000000000000000000, 1.000000000000000000 ) ) ;
#31411 = ADVANCED_FACE ( 'NONE', ( #11810 ), #22070, .F. ) ;
#31412 = EDGE_CURVE ( 'NONE', #38968, #6578, #15311, .T. ) ;
#31413 = EDGE_CURVE ( 'NONE', #7587, #24871, #42078, .T. ) ;
#31415 = VERTEX_POINT ( 'NONE', #36385 ) ;
#31414 = DIRECTION ( 'NONE',  ( -1.000000000000000000, 0.000000000000000000, -0.000000000000000000 ) ) ;
#31416 = CARTESIAN_POINT ( 'NONE',  ( 2.649999999999762323, 150.5000000000013642, 10.00000000000041744 ) ) ;
#31417 = CIRCLE ( 'NONE', #34887, 59.00000000000000000 ) ;
#31418 = CARTESIAN_POINT ( 'NONE',  ( -2.688821387764050996E-14, -4.618802153517012954, -0.4999999999999995559 ) ) ;
#31419 = ORIENTED_EDGE ( 'NONE', *, *, #22427, .F. ) ;
#31420 = CARTESIAN_POINT ( 'NONE',  ( 4.417864660711233959, 40.00000000000000000, 67.39583333436242185 ) ) ;
#31421 = CARTESIAN_POINT ( 'NONE',  ( 18.00000000000000355, 44.75336757549799671, -14.30704879393557150 ) ) ;
#31422 = AXIS2_PLACEMENT_3D ( 'NONE', #11964, #25290, #31807 ) ;
#31423 = CIRCLE ( 'NONE', #25192, 59.00000000000000000 ) ;
#31424 = ORIENTED_EDGE ( 'NONE', *, *, #37318, .F. ) ;
#31425 = AXIS2_PLACEMENT_3D ( 'NONE', #39869, #23140, #13092 ) ;
#31426 = CARTESIAN_POINT ( 'NONE',  ( 0.000000000000000000, 0.000000000000000000, 0.000000000000000000 ) ) ;
#31427 = DIRECTION ( 'NONE',  ( -1.000000000000000000, -0.000000000000000000, -0.000000000000000000 ) ) ;
#31428 = AXIS2_PLACEMENT_3D ( 'NONE', #26586, #3629, #17001 ) ;
#31429 = VERTEX_POINT ( 'NONE', #32908 ) ;
#31430 = FACE_OUTER_BOUND ( 'NONE', #14659, .T. ) ;
#31431 = ORIENTED_EDGE ( 'NONE', *, *, #38096, .T. ) ;
#31432 = DIRECTION ( 'NONE',  ( 0.000000000000000000, -0.4817536741017223179, 0.8763066800438598092 ) ) ;
#31433 = EDGE_LOOP ( 'NONE', ( #14160, #1330, #247, #33757 ) ) ;
#31434 = CARTESIAN_POINT ( 'NONE',  ( 8.999999999999998224, -18.42432724429495394, 30.92804820215996386 ) ) ;
#31435 = DIRECTION ( 'NONE',  ( 0.000000000000000000, -0.1590634960190595026, -0.9872683547213466637 ) ) ;
#31436 = EDGE_LOOP ( 'NONE', ( #8635, #37616, #35621, #1008 ) ) ;
#31437 = FACE_OUTER_BOUND ( 'NONE', #13200, .T. ) ;
#31438 = CYLINDRICAL_SURFACE ( 'NONE', #40073, 59.00000000000000000 ) ;
#31439 = ORIENTED_EDGE ( 'NONE', *, *, #33693, .T. ) ;
#31440 = CARTESIAN_POINT ( 'NONE',  ( 147.8499999999987438, 1.400182730016050856E-12, 9.999999999999962697 ) ) ;
#31441 = DIRECTION ( 'NONE',  ( 1.000000000000000000, 0.000000000000000000, 0.000000000000000000 ) ) ;
#31442 = EDGE_LOOP ( 'NONE', ( #24950, #34684, #42062, #13549, #18573 ) ) ;
#31443 = DIRECTION ( 'NONE',  ( 1.000000000000000000, 0.000000000000000000, 0.000000000000000000 ) ) ;
#31444 = DIRECTION ( 'NONE',  ( -1.000000000000000000, -0.000000000000000000, -0.000000000000000000 ) ) ;
#31445 = APPLICATION_PROTOCOL_DEFINITION ( 'draft international standard', 'automotive_design', 1998, #24534 ) ;
#31446 = DIRECTION ( 'NONE',  ( -1.000000000000000000, -0.000000000000000000, -0.000000000000000000 ) ) ;
#31447 = CARTESIAN_POINT ( 'NONE',  ( 54.43714469963884284, 31.00000000000000355, -7.178810421751046000 ) ) ;
#31448 = CIRCLE ( 'NONE', #23801, 31.49899999999999878 ) ;
#31449 = VERTEX_POINT ( 'NONE', #3433 ) ;
#31451 = CARTESIAN_POINT ( 'NONE',  ( 0.000000000000000000, 0.000000000000000000, 0.000000000000000000 ) ) ;
#31450 = CARTESIAN_POINT ( 'NONE',  ( 17.99999999999999645, 0.000000000000000000, 0.000000000000000000 ) ) ;
#31452 = CIRCLE ( 'NONE', #12642, 58.99999999999999289 ) ;
#31453 = CARTESIAN_POINT ( 'NONE',  ( 0.000000000000000000, 36.05989434073656952, -30.12041790338580682 ) ) ;
#31454 = ORIENTED_EDGE ( 'NONE', *, *, #15131, .T. ) ;
#31455 = VECTOR ( 'NONE', #23074, 1000.000000000000000 ) ;
#31456 = DIRECTION ( 'NONE',  ( -1.000000000000000000, -0.000000000000000000, 0.000000000000000000 ) ) ;
#31457 = CARTESIAN_POINT ( 'NONE',  ( 14.80739997004469366, 40.00000000000000000, 55.25628696611591550 ) ) ;
#31458 = CARTESIAN_POINT ( 'NONE',  ( 46.08863070263672057, 40.00000000000000000, 35.47900410130833393 ) ) ;
#31459 = AXIS2_PLACEMENT_3D ( 'NONE', #7598, #2255, #15614 ) ;
#31460 = CARTESIAN_POINT ( 'NONE',  ( 18.00000000000000355, 13.56094713063571078, 50.20060470671745634 ) ) ;
#31461 = CARTESIAN_POINT ( 'NONE',  ( 0.000000000000000000, 2.357898499370431722, -2.818925648462311528E-15 ) ) ;
#31462 = ADVANCED_FACE ( 'NONE', ( #42500 ), #25960, .F. ) ;
#31463 = EDGE_CURVE ( 'NONE', #22696, #26637, #9578, .T. ) ;
#31464 = CARTESIAN_POINT ( 'NONE',  ( 17.99999999999999645, 25.52601536738592358, 19.21447964122706509 ) ) ;
#31465 = CARTESIAN_POINT ( 'NONE',  ( 5.935205493550105516, 31.00000000000000355, -22.18504493031268865 ) ) ;
#31466 = EDGE_CURVE ( 'NONE', #27712, #6599, #18448, .T. ) ;
#31467 = AXIS2_PLACEMENT_3D ( 'NONE', #32729, #39476, #32519 ) ;
#31468 = VERTEX_POINT ( 'NONE', #13090 ) ;
#31469 = CARTESIAN_POINT ( 'NONE',  ( 4.274771203358150196, 40.00000000000000000, -32.49882260841580006 ) ) ;
#31470 = VERTEX_POINT ( 'NONE', #16350 ) ;
#31471 = CARTESIAN_POINT ( 'NONE',  ( 0.000000000000000000, -12.42760411676061949, 33.78690065568420664 ) ) ;
#31472 = DIRECTION ( 'NONE',  ( 0.000000000000000000, 0.000000000000000000, -1.000000000000000000 ) ) ;
#31473 = ORIENTED_EDGE ( 'NONE', *, *, #19989, .T. ) ;
#31474 = DIRECTION ( 'NONE',  ( 0.000000000000000000, 0.5877852522924685852, 0.8090169943749507819 ) ) ;
#31475 = FACE_OUTER_BOUND ( 'NONE', #11966, .T. ) ;
#31476 = VERTEX_POINT ( 'NONE', #39221 ) ;
#31477 = CARTESIAN_POINT ( 'NONE',  ( 32.30287614962725229, -34.05525454449571754, 69.29271901957299917 ) ) ;
#31478 = ORIENTED_EDGE ( 'NONE', *, *, #32672, .T. ) ;
#31479 = CIRCLE ( 'NONE', #9840, 58.99999999999998579 ) ;
#31480 = ORIENTED_EDGE ( 'NONE', *, *, #34246, .T. ) ;
#31481 = FACE_OUTER_BOUND ( 'NONE', #33808, .T. ) ;
#31482 = CIRCLE ( 'NONE', #4288, 58.99999999999998579 ) ;
#31483 = ADVANCED_FACE ( 'NONE', ( #6291 ), #42935, .F. ) ;
#31484 = CARTESIAN_POINT ( 'NONE',  ( -19.10382689932575673, 31.00000000000000355, -71.73905014346600240 ) ) ;
#31485 = ORIENTED_EDGE ( 'NONE', *, *, #191, .F. ) ;
#31486 = CYLINDRICAL_SURFACE ( 'NONE', #30053, 116.0000000000000000 ) ;
#31487 = AXIS2_PLACEMENT_3D ( 'NONE', #36214, #6335, #19680 ) ;
#31488 = DIRECTION ( 'NONE',  ( 0.000000000000000000, 0.000000000000000000, 1.000000000000000000 ) ) ;
#31489 = ORIENTED_EDGE ( 'NONE', *, *, #29830, .F. ) ;
#31490 = DIRECTION ( 'NONE',  ( -1.000000000000000000, -0.000000000000000000, -0.000000000000000000 ) ) ;
#31491 = ORIENTED_EDGE ( 'NONE', *, *, #3246, .F. ) ;
#31492 = CARTESIAN_POINT ( 'NONE',  ( 44.33290732825513203, 40.00000000000000000, 77.00207852759155003 ) ) ;
#31493 = CARTESIAN_POINT ( 'NONE',  ( 12.70938237924789327, 31.00000000000000355, -21.97768283340561979 ) ) ;
#31495 = DIRECTION ( 'NONE',  ( -1.000000000000000000, -0.000000000000000000, -0.000000000000000000 ) ) ;
#31494 = CARTESIAN_POINT ( 'NONE',  ( 17.99999999999999645, 109.1131968883998695, -26.12628443611929896 ) ) ;
#31496 = DIRECTION ( 'NONE',  ( 1.000000000000000000, 0.000000000000000000, 0.000000000000000000 ) ) ;
#31497 = EDGE_CURVE ( 'NONE', #28805, #41404, #35118, .T. ) ;
#31498 = CARTESIAN_POINT ( 'NONE',  ( 0.000000000000000000, 0.000000000000000000, 0.000000000000000000 ) ) ;
#31499 = ORIENTED_EDGE ( 'NONE', *, *, #14841, .F. ) ;
#31500 = DIRECTION ( 'NONE',  ( 0.000000000000000000, 0.000000000000000000, 1.000000000000000000 ) ) ;
#31501 = ORIENTED_EDGE ( 'NONE', *, *, #7287, .T. ) ;
#31502 = DIRECTION ( 'NONE',  ( 0.000000000000000000, 0.000000000000000000, 1.000000000000000000 ) ) ;
#31503 = CARTESIAN_POINT ( 'NONE',  ( 24.08498528996878107, 31.00000000000000355, -89.94621034038658536 ) ) ;
#31504 = CARTESIAN_POINT ( 'NONE',  ( 0.000000000000000000, -56.51398178981757070, -96.92493144647505687 ) ) ;
#31505 = VERTEX_POINT ( 'NONE', #9348 ) ;
#31506 = CARTESIAN_POINT ( 'NONE',  ( -30.58448433907587827, 40.00000000000000000, 8.146263651249089577 ) ) ;
#31507 = VERTEX_POINT ( 'NONE', #2576 ) ;
#31508 = AXIS2_PLACEMENT_3D ( 'NONE', #33218, #3301, #26256 ) ;
#31509 = EDGE_LOOP ( 'NONE', ( #24627, #36052, #14212, #11081 ) ) ;
#31510 = LINE ( 'NONE', #21300, #29686 ) ;
#31511 = DIRECTION ( 'NONE',  ( 1.000000000000000000, 0.000000000000000000, -0.000000000000000000 ) ) ;
#31512 = DIRECTION ( 'NONE',  ( 0.000000000000000000, 0.000000000000000000, 1.000000000000000000 ) ) ;
#31513 = AXIS2_PLACEMENT_3D ( 'NONE', #31211, #1722, #4798 ) ;
#31514 = ADVANCED_FACE ( 'NONE', ( #33124, #16141, #3212, #22706 ), #33351, .F. ) ;
#31515 = FACE_BOUND ( 'NONE', #31029, .T. ) ;
#31516 = ORIENTED_EDGE ( 'NONE', *, *, #23701, .F. ) ;
#31517 = FACE_OUTER_BOUND ( 'NONE', #23942, .T. ) ;
#31518 = ORIENTED_EDGE ( 'NONE', *, *, #16653, .T. ) ;
#31519 = DIRECTION ( 'NONE',  ( 1.000000000000000000, 0.000000000000000000, 0.000000000000000000 ) ) ;
#31520 = VECTOR ( 'NONE', #14498, 1000.000000000000000 ) ;
#31521 = FACE_OUTER_BOUND ( 'NONE', #13965, .T. ) ;
#31522 = EDGE_CURVE ( 'NONE', #13721, #1418, #43149, .T. ) ;
#31523 = CARTESIAN_POINT ( 'NONE',  ( 9.000000000000001776, 12.30077720129095198, 50.52416135122086160 ) ) ;
#31524 = DIRECTION ( 'NONE',  ( 1.000000000000000000, 0.000000000000000000, 0.000000000000000000 ) ) ;
#31525 = EDGE_LOOP ( 'NONE', ( #23603, #27403, #38303, #9957 ) ) ;
#31526 = ORIENTED_EDGE ( 'NONE', *, *, #37560, .T. ) ;
#31527 = CARTESIAN_POINT ( 'NONE',  ( 42.80287614962790599, -40.05525454449572464, 69.29271901957253021 ) ) ;
#31528 = DIRECTION ( 'NONE',  ( 1.000000000000000000, 0.000000000000000000, 0.000000000000000000 ) ) ;
#31529 = ADVANCED_FACE ( 'NONE', ( #13303 ), #2777, .F. ) ;
#31530 = VERTEX_POINT ( 'NONE', #35955 ) ;
#31532 = ORIENTED_EDGE ( 'NONE', *, *, #1489, .F. ) ;
#31531 = DIRECTION ( 'NONE',  ( 0.000000000000000000, -0.8443279255020087470, -0.5358267949790065376 ) ) ;
#31533 = ADVANCED_FACE ( 'NONE', ( #23561 ), #20087, .F. ) ;
#31534 = CARTESIAN_POINT ( 'NONE',  ( 42.86166521170756027, 31.00000000000000355, 21.22462828018744219 ) ) ;
#31535 = LINE ( 'NONE', #1622, #4199 ) ;
#31536 = CARTESIAN_POINT ( 'NONE',  ( -4.000000000000000000, 0.9868501483902560878, -0.09357334158579519445 ) ) ;
#31537 = ORIENTED_EDGE ( 'NONE', *, *, #21673, .T. ) ;
#31538 = AXIS2_PLACEMENT_3D ( 'NONE', #42945, #35744, #3224 ) ;
#31539 = CARTESIAN_POINT ( 'NONE',  ( 0.000000000000000000, 10.40101730206529140, -120.0512800434970018 ) ) ;
#31540 = CARTESIAN_POINT ( 'NONE',  ( -54.47698434027259395, 40.00000000000000000, -31.57393205620729404 ) ) ;
#31541 = AXIS2_PLACEMENT_3D ( 'NONE', #6060, #32250, #2328 ) ;
#31542 = CARTESIAN_POINT ( 'NONE',  ( 17.99999999999999645, -73.51007459736489125, 89.73443560133338792 ) ) ;
#31543 = DIRECTION ( 'NONE',  ( -1.000000000000000000, -0.000000000000000000, -0.000000000000000000 ) ) ;
#31544 = ORIENTED_EDGE ( 'NONE', *, *, #25808, .T. ) ;
#31545 = FACE_OUTER_BOUND ( 'NONE', #33994, .T. ) ;
#31546 = EDGE_LOOP ( 'NONE', ( #25026, #42269, #37842, #9100, #21770 ) ) ;
#31547 = ADVANCED_FACE ( 'NONE', ( #146 ), #36829, .F. ) ;
#31548 = VECTOR ( 'NONE', #28407, 1000.000000000000000 ) ;
#31549 = DIRECTION ( 'NONE',  ( -1.000000000000000000, 0.000000000000000000, 0.000000000000000000 ) ) ;
#31550 = DIRECTION ( 'NONE',  ( -1.000000000000000000, -0.000000000000000000, -0.000000000000000000 ) ) ;
#31551 = CARTESIAN_POINT ( 'NONE',  ( 59.08215048199704711, 31.00000000000000000, 29.12166076728773589 ) ) ;
#31552 = DIRECTION ( 'NONE',  ( 0.000000000000000000, 0.000000000000000000, 1.000000000000000000 ) ) ;
#31553 = ORIENTED_EDGE ( 'NONE', *, *, #35197, .T. ) ;
#31554 = LINE ( 'NONE', #14568, #29632 ) ;
#31555 = ORIENTED_EDGE ( 'NONE', *, *, #22433, .F. ) ;
#31556 = CARTESIAN_POINT ( 'NONE',  ( 17.99999999999999645, 104.0201923570382405, -51.34003878070953419 ) ) ;
#31557 = CARTESIAN_POINT ( 'NONE',  ( 18.00000000000000355, 17.50309955389612426, 43.60271849949370448 ) ) ;
#31558 = CARTESIAN_POINT ( 'NONE',  ( -81.27520743792995006, 31.00000000000000711, 10.59408403752164851 ) ) ;
#31559 = CARTESIAN_POINT ( 'NONE',  ( -92.09225407318750456, 40.00000000000000711, -6.144973693751363264 ) ) ;
#31560 = CARTESIAN_POINT ( 'NONE',  ( 0.000000000000000000, -111.8797445107945236, 8.437727291342365987 ) ) ;
#31561 = EDGE_CURVE ( 'NONE', #11934, #34763, #29443, .T. ) ;
#31562 = CIRCLE ( 'NONE', #17647, 20.00000000000000711 ) ;
#31563 = ORIENTED_EDGE ( 'NONE', *, *, #27597, .T. ) ;
#31564 = FACE_OUTER_BOUND ( 'NONE', #4935, .T. ) ;
#31565 = VERTEX_POINT ( 'NONE', #29233 ) ;
#31566 = LINE ( 'NONE', #15012, #15810 ) ;
#31567 = CARTESIAN_POINT ( 'NONE',  ( 17.99999999999999645, -11.41303419185048185, 111.6154788735835410 ) ) ;
#31568 = AXIS2_PLACEMENT_3D ( 'NONE', #29388, #26116, #19380 ) ;
#31570 = ORIENTED_EDGE ( 'NONE', *, *, #15526, .F. ) ;
#31569 = DIRECTION ( 'NONE',  ( 0.000000000000000000, 1.000000000000000000, 0.000000000000000000 ) ) ;
#31571 = DIRECTION ( 'NONE',  ( 0.000000000000000000, 0.000000000000000000, 1.000000000000000000 ) ) ;
#31572 = VERTEX_POINT ( 'NONE', #39443 ) ;
#31573 = DIRECTION ( 'NONE',  ( 0.000000000000000000, 0.000000000000000000, -1.000000000000000000 ) ) ;
#31574 = ADVANCED_FACE ( 'NONE', ( #13734 ), #14372, .T. ) ;
#31575 = CARTESIAN_POINT ( 'NONE',  ( -86.05617919112455638, 40.00000000000000711, 49.70311056393224192 ) ) ;
#31576 = CARTESIAN_POINT ( 'NONE',  ( 18.00000000000000355, 0.000000000000000000, 0.000000000000000000 ) ) ;
#31577 = AXIS2_PLACEMENT_3D ( 'NONE', #822, #28360, #37700 ) ;
#31578 = VERTEX_POINT ( 'NONE', #37476 ) ;
#31579 = CARTESIAN_POINT ( 'NONE',  ( 0.000000000000000000, 0.000000000000000000, -1.199999999999999956 ) ) ;
#31580 = CARTESIAN_POINT ( 'NONE',  ( 17.99999999999999645, -120.4984140710909344, 0.7894348306980537577 ) ) ;
#31581 = EDGE_CURVE ( 'NONE', #8344, #9503, #369, .T. ) ;
#31583 = FACE_OUTER_BOUND ( 'NONE', #22746, .T. ) ;
#31582 = DIRECTION ( 'NONE',  ( 0.000000000000000000, -0.7164567402983209599, 0.6976315211349787271 ) ) ;
#31584 = ORIENTED_EDGE ( 'NONE', *, *, #11768, .T. ) ;
#31585 = CARTESIAN_POINT ( 'NONE',  ( 0.000000000000000000, 114.1157422997285806, -20.82300072952825332 ) ) ;
#31586 = EDGE_LOOP ( 'NONE', ( #14287, #34744, #22760, #28894 ) ) ;
#31587 = FACE_OUTER_BOUND ( 'NONE', #23455, .T. ) ;
#31588 = CARTESIAN_POINT ( 'NONE',  ( 3.798394181604433761, 40.00000000000000000, 29.10671710469611284 ) ) ;
#31589 = DIRECTION ( 'NONE',  ( 0.000000000000000000, 0.000000000000000000, 1.000000000000000000 ) ) ;
#31590 = CARTESIAN_POINT ( 'NONE',  ( 17.99999999999999645, -22.66088087769196235, 21.87856208362548571 ) ) ;
#31591 = CARTESIAN_POINT ( 'NONE',  ( -10.00000000000000000, 0.000000000000000000, 0.000000000000000000 ) ) ;
#31592 = EDGE_LOOP ( 'NONE', ( #7381, #33349, #38216, #32140 ) ) ;
#31593 = DIRECTION ( 'NONE',  ( 0.000000000000000000, -1.000000000000000000, 5.297542245118643184E-16 ) ) ;
#31594 = ORIENTED_EDGE ( 'NONE', *, *, #5750, .T. ) ;
#31595 = AXIS2_PLACEMENT_3D ( 'NONE', #3393, #106, #13474 ) ;
#31596 = ADVANCED_FACE ( 'NONE', ( #10439 ), #7803, .T. ) ;
#31597 = CARTESIAN_POINT ( 'NONE',  ( 102.9999999999993463, -2.265858372770185743E-13, -32.00000000000000000 ) ) ;
#31598 = DIRECTION ( 'NONE',  ( -1.000000000000000000, -0.000000000000000000, 0.000000000000000000 ) ) ;
#31600 = EDGE_CURVE ( 'NONE', #28601, #5117, #10880, .T. ) ;
#31599 = CARTESIAN_POINT ( 'NONE',  ( -39.12533628356670334, 31.00000000000000355, -10.47265044290268499 ) ) ;
#31601 = ORIENTED_EDGE ( 'NONE', *, *, #22927, .F. ) ;
#31602 = DIRECTION ( 'NONE',  ( -1.000000000000000000, -0.000000000000000000, 0.000000000000000000 ) ) ;
#31603 = DIRECTION ( 'NONE',  ( 0.000000000000000000, 0.000000000000000000, 1.000000000000000000 ) ) ;
#31604 = CARTESIAN_POINT ( 'NONE',  ( 24.81019160154284720, 31.00000000000000355, 73.04493173762017477 ) ) ;
#31605 = VERTEX_POINT ( 'NONE', #3643 ) ;
#31606 = CARTESIAN_POINT ( 'NONE',  ( -26.77709713317330653, 31.00000000000000355, 54.08981485145582013 ) ) ;
#31607 = CARTESIAN_POINT ( 'NONE',  ( 85.10416666585589951, 39.99999999999999289, 5.563236982362346872 ) ) ;
#31608 = AXIS2_PLACEMENT_3D ( 'NONE', #41004, #3907, #17293 ) ;
#31609 = EDGE_CURVE ( 'NONE', #1751, #35293, #14945, .T. ) ;
#31610 = VERTEX_POINT ( 'NONE', #17240 ) ;
#31611 = DIRECTION ( 'NONE',  ( 0.000000000000000000, 0.000000000000000000, 1.000000000000000000 ) ) ;
#31612 = FACE_OUTER_BOUND ( 'NONE', #13159, .T. ) ;
#31613 = AXIS2_PLACEMENT_3D ( 'NONE', #31504, #1590, #31069 ) ;
#31614 = DIRECTION ( 'NONE',  ( 0.000000000000000000, 0.000000000000000000, 1.000000000000000000 ) ) ;
#31615 = CIRCLE ( 'NONE', #37173, 0.2500000000000002220 ) ;
#31617 = ORIENTED_EDGE ( 'NONE', *, *, #8796, .T. ) ;
#31616 = LINE ( 'NONE', #28793, #30701 ) ;
#31618 = DIRECTION ( 'NONE',  ( 1.000000000000000000, 0.000000000000000000, -0.000000000000000000 ) ) ;
#31619 = LINE ( 'NONE', #34676, #4910 ) ;
#31620 = EDGE_CURVE ( 'NONE', #5769, #7227, #25411, .T. ) ;
#31621 = AXIS2_PLACEMENT_3D ( 'NONE', #5684, #25587, #38843 ) ;
#31622 = VERTEX_POINT ( 'NONE', #30938 ) ;
#31623 = CARTESIAN_POINT ( 'NONE',  ( -8.160545988181935328, 40.00000000000000000, -61.88879904071598048 ) ) ;
#31624 = CYLINDRICAL_SURFACE ( 'NONE', #41690, 59.00000000000000000 ) ;
#31625 = VERTEX_POINT ( 'NONE', #11310 ) ;
#31626 = EDGE_CURVE ( 'NONE', #5016, #27790, #5893, .T. ) ;
#31627 = CYLINDRICAL_SURFACE ( 'NONE', #12037, 47.49900000000000233 ) ;
#31628 = DIRECTION ( 'NONE',  ( -1.000000000000000000, 0.000000000000000000, -0.000000000000000000 ) ) ;
#31629 = CARTESIAN_POINT ( 'NONE',  ( 18.00000000000000355, 46.90537658765331486, 2.727856614654470491 ) ) ;
#31630 = ORIENTED_EDGE ( 'NONE', *, *, #18295, .T. ) ;
#31631 =( GEOMETRIC_REPRESENTATION_CONTEXT ( 3 ) GLOBAL_UNCERTAINTY_ASSIGNED_CONTEXT ( ( #38599 ) ) GLOBAL_UNIT_ASSIGNED_CONTEXT ( ( #18440, #18671, #4870 ) ) REPRESENTATION_CONTEXT ( 'NONE', 'WORKASPACE' ) );
#31632 = ORIENTED_EDGE ( 'NONE', *, *, #35960, .F. ) ;
#31633 = CARTESIAN_POINT ( 'NONE',  ( 0.000000000000000000, 35.89808275599445153, -2.706964063997353342 ) ) ;
#31634 = AXIS2_PLACEMENT_3D ( 'NONE', #2481, #22619, #16057 ) ;
#31635 = ORIENTED_EDGE ( 'NONE', *, *, #9222, .F. ) ;
#31636 = FACE_OUTER_BOUND ( 'NONE', #31801, .T. ) ;
#31637 = DIRECTION ( 'NONE',  ( 1.000000000000000000, 0.000000000000000000, -0.000000000000000000 ) ) ;
#31638 = CARTESIAN_POINT ( 'NONE',  ( -15.99999999999997691, 40.00000000000000000, 5.571627607371296764E-15 ) ) ;
#31639 = FACE_OUTER_BOUND ( 'NONE', #13088, .T. ) ;
#31641 = VERTEX_POINT ( 'NONE', #7146 ) ;
#31640 = VECTOR ( 'NONE', #25340, 1000.000000000000000 ) ;
#31642 = DIRECTION ( 'NONE',  ( 1.000000000000000000, 0.000000000000000000, 0.000000000000000000 ) ) ;
#31643 = CIRCLE ( 'NONE', #38601, 120.5010000000000190 ) ;
#31644 = CARTESIAN_POINT ( 'NONE',  ( 0.000000000000000000, -30.01658535635190361, -108.1077105353201233 ) ) ;
#31645 = EDGE_CURVE ( 'NONE', #7685, #38997, #42781, .T. ) ;
#31646 = EDGE_CURVE ( 'NONE', #33231, #22420, #27688, .T. ) ;
#31647 = ORIENTED_EDGE ( 'NONE', *, *, #13791, .T. ) ;
#31648 = CYLINDRICAL_SURFACE ( 'NONE', #13433, 13.59999999999999787 ) ;
#31649 = EDGE_CURVE ( 'NONE', #18913, #22284, #3854, .T. ) ;
#31650 = EDGE_CURVE ( 'NONE', #33431, #42007, #33053, .T. ) ;
#31651 = CIRCLE ( 'NONE', #26085, 59.00000000000000000 ) ;
#31652 = DIRECTION ( 'NONE',  ( 0.000000000000000000, 0.000000000000000000, 1.000000000000000000 ) ) ;
#31653 = SHAPE_DEFINITION_REPRESENTATION ( #26999, #16840 ) ;
#31655 = CIRCLE ( 'NONE', #12849, 59.00000000000000000 ) ;
#31654 = CYLINDRICAL_SURFACE ( 'NONE', #41373, 51.99999999999999289 ) ;
#31656 = CARTESIAN_POINT ( 'NONE',  ( 6.197074855318628117, 31.00000000000000355, 46.98549035852928313 ) ) ;
#31657 = ORIENTED_EDGE ( 'NONE', *, *, #13190, .F. ) ;
#31659 = DIRECTION ( 'NONE',  ( -1.000000000000000000, 0.000000000000000000, -0.000000000000000000 ) ) ;
#31658 = CYLINDRICAL_SURFACE ( 'NONE', #28194, 116.0000000000000000 ) ;
#31660 = ORIENTED_EDGE ( 'NONE', *, *, #33189, .T. ) ;
#31661 = CARTESIAN_POINT ( 'NONE',  ( -35.70415035507907930, 40.00000000000000000, 46.55071329160319493 ) ) ;
#31662 = PRODUCT_DEFINITION_FORMATION_WITH_SPECIFIED_SOURCE ( 'ANY', '', #19330, .NOT_KNOWN. ) ;
#31663 = CARTESIAN_POINT ( 'NONE',  ( -49.80813925210025417, 40.00000000000000000, -17.00652635548005520 ) ) ;
#31664 = COLOUR_RGB ( '', 0.66274510, 0.83137255, 0.94901961) ;
#31665 = DIRECTION ( 'NONE',  ( -1.000000000000000000, -0.000000000000000000, -0.000000000000000000 ) ) ;
#31666 = CARTESIAN_POINT ( 'NONE',  ( 6.200000000000003730, 6.971071669133949438E-15, 0.000000000000000000 ) ) ;
#31667 = CARTESIAN_POINT ( 'NONE',  ( 18.00000000000000355, 42.03146605346817921, -22.12489237027272893 ) ) ;
#31668 = CIRCLE ( 'NONE', #16358, 58.99999999999999289 ) ;
#31669 = CARTESIAN_POINT ( 'NONE',  ( 19.04566582976364941, 31.00000000000000355, -14.62000746238684989 ) ) ;
#31670 = AXIS2_PLACEMENT_3D ( 'NONE', #19017, #41670, #15316 ) ;
#31671 = EDGE_CURVE ( 'NONE', #10423, #2044, #7591, .T. ) ;
#31672 = ORIENTED_EDGE ( 'NONE', *, *, #17921, .T. ) ;
#31673 = CARTESIAN_POINT ( 'NONE',  ( 8.528031178950213231, 40.00000000000000000, -31.86521141804621493 ) ) ;
#31674 = ORIENTED_EDGE ( 'NONE', *, *, #29915, .F. ) ;
#31675 = CARTESIAN_POINT ( 'NONE',  ( -10.00000000000000000, 0.000000000000000000, 0.000000000000000000 ) ) ;
#31676 = DIRECTION ( 'NONE',  ( 0.000000000000000000, -0.9980267284282722251, 0.06279051952930256308 ) ) ;
#31677 = AXIS2_PLACEMENT_3D ( 'NONE', #41955, #5318, #18690 ) ;
#31678 = VERTEX_POINT ( 'NONE', #33993 ) ;
#31679 = ADVANCED_FACE ( 'NONE', ( #13948 ), #11103, .T. ) ;
#31680 = CARTESIAN_POINT ( 'NONE',  ( 18.00000000000000355, 0.000000000000000000, 0.000000000000000000 ) ) ;
#31681 = DIRECTION ( 'NONE',  ( -1.000000000000000000, 0.000000000000000000, -0.000000000000000000 ) ) ;
#31682 = ORIENTED_EDGE ( 'NONE', *, *, #24608, .F. ) ;
#31683 = FACE_OUTER_BOUND ( 'NONE', #15621, .T. ) ;
#31684 = ORIENTED_EDGE ( 'NONE', *, *, #22144, .T. ) ;
#31685 = AXIS2_PLACEMENT_3D ( 'NONE', #24628, #24853, #37880 ) ;
#31686 = ORIENTED_EDGE ( 'NONE', *, *, #1189, .F. ) ;
#31687 = CARTESIAN_POINT ( 'NONE',  ( 17.99999999999999645, 95.38615066513983720, 59.07414607872858170 ) ) ;
#31688 = CARTESIAN_POINT ( 'NONE',  ( -41.82916961767931951, 31.00000000000000355, -72.66191475361131324 ) ) ;
#31689 = ORIENTED_EDGE ( 'NONE', *, *, #15425, .F. ) ;
#31690 = CYLINDRICAL_SURFACE ( 'NONE', #9134, 20.00000000000000711 ) ;
#31691 = DIRECTION ( 'NONE',  ( -1.000000000000000000, -0.000000000000000000, 0.000000000000000000 ) ) ;
#31692 = AXIS2_PLACEMENT_3D ( 'NONE', #27945, #22055, #17932 ) ;
#31693 = EDGE_LOOP ( 'NONE', ( #25038, #11831, #27259, #5385 ) ) ;
#31695 = VECTOR ( 'NONE', #23253, 1000.000000000000000 ) ;
#31694 = DIRECTION ( 'NONE',  ( 1.000000000000000000, 0.000000000000000000, 0.000000000000000000 ) ) ;
#31696 = CARTESIAN_POINT ( 'NONE',  ( 0.000000000000000000, 15.49408907645234201, -44.90087086784576087 ) ) ;
#31697 = CARTESIAN_POINT ( 'NONE',  ( -3.925388345519843725, 31.00000000000000355, 29.51202942214661462 ) ) ;
#31699 = CARTESIAN_POINT ( 'NONE',  ( 0.000000000000000000, 116.0452958106480708, 32.46506308663498430 ) ) ;
#31698 = DIRECTION ( 'NONE',  ( 1.000000000000000000, 0.000000000000000000, 0.000000000000000000 ) ) ;
#31700 = ADVANCED_FACE ( 'NONE', ( #33556 ), #17670, .T. ) ;
#31701 = EDGE_CURVE ( 'NONE', #40182, #18148, #42102, .T. ) ;
#31702 = VECTOR ( 'NONE', #32541, 1000.000000000000000 ) ;
#31703 = DIRECTION ( 'NONE',  ( 0.000000000000000000, 0.000000000000000000, 1.000000000000000000 ) ) ;
#31704 = DIRECTION ( 'NONE',  ( 1.000000000000000000, 0.000000000000000000, 0.000000000000000000 ) ) ;
#31705 = AXIS2_PLACEMENT_3D ( 'NONE', #29078, #12282, #42348 ) ;
#31706 = ORIENTED_EDGE ( 'NONE', *, *, #24248, .T. ) ;
#31707 = EDGE_CURVE ( 'NONE', #11569, #25432, #24214, .T. ) ;
#31708 = FACE_OUTER_BOUND ( 'NONE', #5495, .T. ) ;
#31709 = VERTEX_POINT ( 'NONE', #1021 ) ;
#31710 = AXIS2_PLACEMENT_3D ( 'NONE', #35936, #6704, #33334 ) ;
#31711 = CARTESIAN_POINT ( 'NONE',  ( 17.99999999999999645, 0.000000000000000000, 0.000000000000000000 ) ) ;
#31712 = CARTESIAN_POINT ( 'NONE',  ( 92.36625196220676060, 31.00000000000000000, 24.73319171124347093 ) ) ;
#31713 = CARTESIAN_POINT ( 'NONE',  ( 0.000000000000000000, -30.93515269692137792, 36.04401931830242489 ) ) ;
#31714 = ORIENTED_EDGE ( 'NONE', *, *, #683, .F. ) ;
#31715 = AXIS2_PLACEMENT_3D ( 'NONE', #17420, #7558, #774 ) ;
#31716 = CARTESIAN_POINT ( 'NONE',  ( 9.304442065600174061, 40.00000000000000000, 27.50946418541003169 ) ) ;
#31717 = CIRCLE ( 'NONE', #14285, 58.99999999999998579 ) ;
#31718 = ORIENTED_EDGE ( 'NONE', *, *, #34899, .F. ) ;
#31719 = EDGE_CURVE ( 'NONE', #10605, #23617, #28913, .T. ) ;
#31720 = ORIENTED_EDGE ( 'NONE', *, *, #13170, .F. ) ;
#31721 = DIRECTION ( 'NONE',  ( -1.000000000000000000, 0.000000000000000000, 0.000000000000000000 ) ) ;
#31722 = CARTESIAN_POINT ( 'NONE',  ( 20.00000000000001776, -1.127613248556852545E-13, -39.99999999999999289 ) ) ;
#31723 = FACE_OUTER_BOUND ( 'NONE', #4187, .T. ) ;
#31724 = FACE_BOUND ( 'NONE', #19696, .T. ) ;
#31725 = DIRECTION ( 'NONE',  ( 1.000000000000000000, 0.000000000000000000, 0.000000000000000000 ) ) ;
#31726 = ORIENTED_EDGE ( 'NONE', *, *, #40674, .F. ) ;
#31727 = PLANE ( 'NONE',  #4730 ) ;
#31728 = VERTEX_POINT ( 'NONE', #41820 ) ;
#31729 = DIRECTION ( 'NONE',  ( 0.000000000000000000, 0.000000000000000000, -1.000000000000000000 ) ) ;
#31730 = CIRCLE ( 'NONE', #35902, 59.00000000000000711 ) ;
#31731 = DIRECTION ( 'NONE',  ( -1.000000000000000000, -0.000000000000000000, 0.000000000000000000 ) ) ;
#31732 = CIRCLE ( 'NONE', #18542, 2.649999999999985700 ) ;
#31733 = CARTESIAN_POINT ( 'NONE',  ( 17.99999999999999645, 11.41303419185120482, -111.6154788735834700 ) ) ;
#31734 = CIRCLE ( 'NONE', #5922, 2.649999999999973266 ) ;
#31735 = CARTESIAN_POINT ( 'NONE',  ( 0.000000000000000000, -26.17370628620681927, 39.63700417846155233 ) ) ;
#31736 = ORIENTED_EDGE ( 'NONE', *, *, #21329, .T. ) ;
#31737 = CIRCLE ( 'NONE', #12926, 10.49999999999999467 ) ;
#31738 = EDGE_CURVE ( 'NONE', #26000, #21350, #2384, .T. ) ;
#31739 = ORIENTED_EDGE ( 'NONE', *, *, #6314, .F. ) ;
#31740 = DIRECTION ( 'NONE',  ( 1.000000000000000000, 0.000000000000000000, 0.000000000000000000 ) ) ;
#31741 = CIRCLE ( 'NONE', #16421, 116.0000000000000000 ) ;
#31742 = DIRECTION ( 'NONE',  ( 3.996523416598930318E-16, -2.658563593772947863E-15, -1.000000000000000000 ) ) ;
#31743 = AXIS2_PLACEMENT_3D ( 'NONE', #26364, #19191, #39630 ) ;
#31744 = VERTEX_POINT ( 'NONE', #12395 ) ;
#31745 = AXIS2_PLACEMENT_3D ( 'NONE', #35257, #18747, #28096 ) ;
#31747 = VERTEX_POINT ( 'NONE', #22239 ) ;
#31746 = DIRECTION ( 'NONE',  ( -1.000000000000000000, 0.000000000000000000, -0.000000000000000000 ) ) ;
#31748 = CARTESIAN_POINT ( 'NONE',  ( 20.11321884379921343, 31.00000000000000355, -40.61652209561064097 ) ) ;
#31749 = AXIS2_PLACEMENT_3D ( 'NONE', #42468, #13261, #39188 ) ;
#31750 = ORIENTED_EDGE ( 'NONE', *, *, #33042, .T. ) ;
#31751 = DIRECTION ( 'NONE',  ( 0.000000000000000000, 0.000000000000000000, 1.000000000000000000 ) ) ;
#31752 = VECTOR ( 'NONE', #39790, 1000.000000000000000 ) ;
#31754 = CARTESIAN_POINT ( 'NONE',  ( 0.000000000000000000, 46.77034588191335018, -22.72740077717179474 ) ) ;
#31753 = LINE ( 'NONE', #1410, #18255 ) ;
#31755 = AXIS2_PLACEMENT_3D ( 'NONE', #25430, #12326, #38269 ) ;
#31756 = ORIENTED_EDGE ( 'NONE', *, *, #10930, .F. ) ;
#31757 = CARTESIAN_POINT ( 'NONE',  ( -22.66037885604484359, 40.00000000000000000, 66.40833514169634100 ) ) ;
#31758 = CARTESIAN_POINT ( 'NONE',  ( 17.99999999999999645, -35.72777019205596361, -106.3569410558020962 ) ) ;
#31759 = EDGE_CURVE ( 'NONE', #38173, #8515, #37896, .T. ) ;
#31760 = DIRECTION ( 'NONE',  ( 0.000000000000000000, -0.9826841245925190815, -0.1852887240871243513 ) ) ;
#31761 = ORIENTED_EDGE ( 'NONE', *, *, #17545, .F. ) ;
#31762 = CARTESIAN_POINT ( 'NONE',  ( 2.500000000000000000, 0.000000000000000000, 0.000000000000000000 ) ) ;
#31763 = ORIENTED_EDGE ( 'NONE', *, *, #16812, .T. ) ;
#31764 = SHAPE_REPRESENTATION_RELATIONSHIP ( 'NONE' , 'NONE' ,  #13509, #1547 ) ;
#31765 = FACE_OUTER_BOUND ( 'NONE', #22264, .T. ) ;
#31766 = DIRECTION ( 'NONE',  ( 1.000000000000000000, 0.000000000000000000, -6.546126324440850663E-16 ) ) ;
#31767 = CARTESIAN_POINT ( 'NONE',  ( 20.30000058474805869, 31.00000000000000355, -59.80472289869057789 ) ) ;
#31768 = DIRECTION ( 'NONE',  ( 3.009274222672345096E-17, 1.000000000000000000, -2.455023325076455345E-18 ) ) ;
#31769 = CIRCLE ( 'NONE', #26189, 15.99999999999998579 ) ;
#31770 = ORIENTED_EDGE ( 'NONE', *, *, #1347, .T. ) ;
#31771 = CIRCLE ( 'NONE', #3848, 120.5010000000000332 ) ;
#31772 = CIRCLE ( 'NONE', #1090, 58.99999999999999289 ) ;
#31773 = ADVANCED_FACE ( 'NONE', ( #11760 ), #8017, .T. ) ;
#31774 = AXIS2_PLACEMENT_3D ( 'NONE', #20000, #26723, #36306 ) ;
#31775 = LINE ( 'NONE', #29155, #1006 ) ;
#31776 = CIRCLE ( 'NONE', #4593, 20.00000000000000355 ) ;
#31777 = EDGE_CURVE ( 'NONE', #37135, #12470, #36530, .T. ) ;
#31778 = EDGE_LOOP ( 'NONE', ( #8217, #11770, #19031, #42407 ) ) ;
#31780 = AXIS2_PLACEMENT_3D ( 'NONE', #24603, #35232, #28520 ) ;
#31779 = CARTESIAN_POINT ( 'NONE',  ( 9.000000000000001776, -31.17727234463623631, -111.7317219465823115 ) ) ;
#31781 = DIRECTION ( 'NONE',  ( -0.000000000000000000, -0.000000000000000000, 1.000000000000000000 ) ) ;
#31782 = CARTESIAN_POINT ( 'NONE',  ( 58.29702017945731285, 31.00000000000000000, 66.63806913872474524 ) ) ;
#31784 = CARTESIAN_POINT ( 'NONE',  ( -71.82650799747224823, 40.00000000000000711, -41.60779115366585756 ) ) ;
#31783 = AXIS2_PLACEMENT_3D ( 'NONE', #41952, #3460, #6962 ) ;
#31785 = AXIS2_PLACEMENT_3D ( 'NONE', #26100, #32838, #13014 ) ;
#31786 = CARTESIAN_POINT ( 'NONE',  ( 17.99999999999999645, 0.000000000000000000, 0.000000000000000000 ) ) ;
#31787 = AXIS2_PLACEMENT_3D ( 'NONE', #13086, #38423, #39651 ) ;
#31788 = ADVANCED_BREP_SHAPE_REPRESENTATION ( '', ( #42324, #13552 ), #18474 ) ;
#31789 = VERTEX_POINT ( 'NONE', #28340 ) ;
#31790 = FACE_OUTER_BOUND ( 'NONE', #17849, .T. ) ;
#31791 = ORIENTED_EDGE ( 'NONE', *, *, #4195, .F. ) ;
#31792 = CARTESIAN_POINT ( 'NONE',  ( 17.99999999999999645, 0.000000000000000000, 0.000000000000000000 ) ) ;
#31793 = DIRECTION ( 'NONE',  ( 1.000000000000000000, 0.000000000000000000, 0.000000000000000000 ) ) ;
#31795 = ORIENTED_EDGE ( 'NONE', *, *, #31701, .F. ) ;
#31794 = CARTESIAN_POINT ( 'NONE',  ( 8.999999999999998224, -29.09613215194468339, -21.19941258140352858 ) ) ;
#31796 = DIRECTION ( 'NONE',  ( 0.000000000000000000, -1.000000000000000000, 5.297542245118643184E-16 ) ) ;
#31797 = ORIENTED_EDGE ( 'NONE', *, *, #8944, .F. ) ;
#31798 = CARTESIAN_POINT ( 'NONE',  ( 17.99999999999999645, 0.000000000000000000, 0.000000000000000000 ) ) ;
#31799 = CARTESIAN_POINT ( 'NONE',  ( 18.00000000000000355, -6.109652351742118626, 46.58570277113506819 ) ) ;
#31800 = EDGE_CURVE ( 'NONE', #35367, #12837, #15684, .T. ) ;
#31801 = EDGE_LOOP ( 'NONE', ( #20596, #2345, #14172, #10326 ) ) ;
#31802 = DIRECTION ( 'NONE',  ( 0.000000000000000000, 0.000000000000000000, 1.000000000000000000 ) ) ;
#31803 = CARTESIAN_POINT ( 'NONE',  ( 0.000000000000000000, 46.21320724403663860, -10.97699764141904843 ) ) ;
#31804 = CIRCLE ( 'NONE', #27632, 116.0000000000000000 ) ;
#31805 = CIRCLE ( 'NONE', #32503, 14.70000000000000107 ) ;
#31806 = AXIS2_PLACEMENT_3D ( 'NONE', #8668, #22452, #14820 ) ;
#31808 = CARTESIAN_POINT ( 'NONE',  ( -10.50000000000000178, 1.285879139104721028E-15, -1.199999999999999956 ) ) ;
#31807 = DIRECTION ( 'NONE',  ( 0.000000000000000000, 0.7865515558026394682, 0.6175246149461958156 ) ) ;
#31809 = ORIENTED_EDGE ( 'NONE', *, *, #25007, .T. ) ;
#31810 = CARTESIAN_POINT ( 'NONE',  ( 0.000000000000000000, 0.000000000000000000, 0.000000000000000000 ) ) ;
#31811 = ORIENTED_EDGE ( 'NONE', *, *, #40550, .F. ) ;
#31812 = DIRECTION ( 'NONE',  ( 0.000000000000000000, 0.3641605752528168649, 0.9313361774523405412 ) ) ;
#31813 = CARTESIAN_POINT ( 'NONE',  ( -2.197745971917953511, 40.00000000000000000, -34.39891587002171747 ) ) ;
#31814 = CIRCLE ( 'NONE', #38787, 20.00000000000001066 ) ;
#31815 = CARTESIAN_POINT ( 'NONE',  ( 6.004904395537136175, 0.000000000000000000, 19.19999999999999574 ) ) ;
#31816 = AXIS2_PLACEMENT_3D ( 'NONE', #19070, #12924, #22554 ) ;
#31817 = AXIS2_PLACEMENT_3D ( 'NONE', #37928, #17479, #24017 ) ;
#31818 = FACE_OUTER_BOUND ( 'NONE', #10607, .T. ) ;
#31819 = CARTESIAN_POINT ( 'NONE',  ( 0.000000000000000000, -35.54274411428134073, 115.1399337407605259 ) ) ;
#31820 = ORIENTED_EDGE ( 'NONE', *, *, #39111, .T. ) ;
#31821 = DIRECTION ( 'NONE',  ( 0.000000000000000000, 0.000000000000000000, 1.000000000000000000 ) ) ;
#31822 = EDGE_CURVE ( 'NONE', #38233, #41436, #24036, .T. ) ;
#31823 = ORIENTED_EDGE ( 'NONE', *, *, #4329, .T. ) ;
#31824 = DIRECTION ( 'NONE',  ( 0.000000000000000000, 0.3681245526846719240, 0.9297764858882537897 ) ) ;
#31825 = DIRECTION ( 'NONE',  ( 1.000000000000000000, 0.000000000000000000, 0.000000000000000000 ) ) ;
#31826 = CARTESIAN_POINT ( 'NONE',  ( -37.46020281470095625, 31.00000000000000355, 12.72710441276525017 ) ) ;
#31827 = EDGE_LOOP ( 'NONE', ( #6935, #15130 ) ) ;
#31828 = CARTESIAN_POINT ( 'NONE',  ( 0.000000000000000000, -110.1579703617964725, -21.29539948940357164 ) ) ;
#31829 = CIRCLE ( 'NONE', #18630, 59.00000000000000000 ) ;
#31830 = EDGE_CURVE ( 'NONE', #2394, #17019, #35059, .T. ) ;
#31831 = DIRECTION ( 'NONE',  ( 0.8191520442889902442, 1.003171929053522651E-16, -0.5735764363510482688 ) ) ;
#31832 = CARTESIAN_POINT ( 'NONE',  ( -36.24314215638268877, 31.00000000000000355, -73.49571118816069770 ) ) ;
#31833 = ADVANCED_FACE ( 'NONE', ( #38757 ), #4750, .T. ) ;
#31835 = ORIENTED_EDGE ( 'NONE', *, *, #26874, .T. ) ;
#31834 = CIRCLE ( 'NONE', #20026, 11.00000000000023803 ) ;
#31836 = CARTESIAN_POINT ( 'NONE',  ( 17.81483206087466442, 31.00000000000000355, -52.17936214187551514 ) ) ;
#31837 = CARTESIAN_POINT ( 'NONE',  ( -80.23695839127151430, 40.00000000000000711, 39.56677620416681407 ) ) ;
#31838 = CIRCLE ( 'NONE', #8158, 59.00000000000000000 ) ;
#31839 = EDGE_LOOP ( 'NONE', ( #30634, #17483, #14602, #24598 ) ) ;
#31840 = AXIS2_PLACEMENT_3D ( 'NONE', #19670, #32935, #33744 ) ;
#31841 = DIRECTION ( 'NONE',  ( 0.000000000000000000, -6.887872625202028030E-15, 1.000000000000000000 ) ) ;
#31842 = DIRECTION ( 'NONE',  ( -1.000000000000000000, 0.000000000000000000, 0.000000000000000000 ) ) ;
#31843 = DIRECTION ( 'NONE',  ( 1.000000000000000000, 0.000000000000000000, 0.000000000000000000 ) ) ;
#31844 = AXIS2_PLACEMENT_3D ( 'NONE', #31792, #28741, #24623 ) ;
#31846 = VERTEX_POINT ( 'NONE', #31585 ) ;
#31845 = CYLINDRICAL_SURFACE ( 'NONE', #24438, 59.00000000000000000 ) ;
#31847 = DIRECTION ( 'NONE',  ( 1.000000000000000000, 0.000000000000000000, -6.546126324440850663E-16 ) ) ;
#31848 = CARTESIAN_POINT ( 'NONE',  ( 1.655952806101427033, -3.662737355149048302, -1.182683869819604841E-14 ) ) ;
#31849 = AXIS2_PLACEMENT_3D ( 'NONE', #33129, #36388, #16146 ) ;
#31850 = EDGE_LOOP ( 'NONE', ( #12540, #18802, #9719, #3065 ) ) ;
#31851 = CARTESIAN_POINT ( 'NONE',  ( -45.35818215263140019, 40.00000000000000000, 51.72168634911185592 ) ) ;
#31852 = DIRECTION ( 'NONE',  ( -1.000000000000000000, -0.000000000000000000, -0.000000000000000000 ) ) ;
#31853 = ADVANCED_FACE ( 'NONE', ( #8452 ), #1897, .T. ) ;
#31854 = ORIENTED_EDGE ( 'NONE', *, *, #5110, .F. ) ;
#31855 = EDGE_CURVE ( 'NONE', #7746, #40221, #31668, .T. ) ;
#31856 = CARTESIAN_POINT ( 'NONE',  ( 18.00000000000000355, -46.21320724403656044, 10.97699764141937173 ) ) ;
#31857 = CARTESIAN_POINT ( 'NONE',  ( 9.000000000000001776, 98.69720329640956891, 60.94966826379944536 ) ) ;
#31858 = DIRECTION ( 'NONE',  ( -1.000000000000000000, 0.000000000000000000, -0.000000000000000000 ) ) ;
#31859 = EDGE_LOOP ( 'NONE', ( #17441, #8526, #25292, #746 ) ) ;
#31860 = ORIENTED_EDGE ( 'NONE', *, *, #32723, .F. ) ;
#31861 = DIRECTION ( 'NONE',  ( -1.000000000000000000, 0.000000000000000000, 0.000000000000000000 ) ) ;
#31862 = VERTEX_POINT ( 'NONE', #32022 ) ;
#31863 = CARTESIAN_POINT ( 'NONE',  ( -12.69999999999999929, 1.641026710857453510E-15, 13.40000000000000213 ) ) ;
#31864 = CARTESIAN_POINT ( 'NONE',  ( 17.99999999999999645, 47.31079789947627745, -105.9135893174946119 ) ) ;
#31865 = CIRCLE ( 'NONE', #33936, 59.00000000000000000 ) ;
#31866 = CARTESIAN_POINT ( 'NONE',  ( 18.00000000000000355, 46.11014828289831513, 9.022736828081521665 ) ) ;
#31867 = DIRECTION ( 'NONE',  ( 0.000000000000000000, 0.000000000000000000, 1.000000000000000000 ) ) ;
#31868 = EDGE_LOOP ( 'NONE', ( #25346, #43144, #21409, #29816 ) ) ;
#31869 = CIRCLE ( 'NONE', #500, 59.00000000000000000 ) ;
#31870 = DIRECTION ( 'NONE',  ( -1.000000000000000000, 1.373900992973641671E-15, 4.270088556250623393E-16 ) ) ;
#31871 = AXIS2_PLACEMENT_3D ( 'NONE', #7903, #20601, #33872 ) ;
#31873 = CYLINDRICAL_SURFACE ( 'NONE', #33601, 120.5010000000000190 ) ;
#31872 = AXIS2_PLACEMENT_3D ( 'NONE', #39597, #81, #36321 ) ;
#31874 = ORIENTED_EDGE ( 'NONE', *, *, #31620, .T. ) ;
#31875 = CARTESIAN_POINT ( 'NONE',  ( 9.000000000000001776, 41.60679253225764285, 108.2814610871947423 ) ) ;
#31876 = AXIS2_PLACEMENT_3D ( 'NONE', #33484, #23706, #3571 ) ;
#31877 = CARTESIAN_POINT ( 'NONE',  ( 17.99999999999999645, 75.03166794516801019, 94.29071961951534320 ) ) ;
#31878 = APPLICATION_PROTOCOL_DEFINITION ( 'draft international standard', 'automotive_design', 1998, #5815 ) ;
#31879 = EDGE_CURVE ( 'NONE', #25968, #11466, #29591, .T. ) ;
#31880 = CARTESIAN_POINT ( 'NONE',  ( 0.000000000000000000, -0.04937522221144796664, 31.94951095880159997 ) ) ;
#31881 = CARTESIAN_POINT ( 'NONE',  ( 23.58227068755204314, 31.00000000000000355, -47.84673847638903510 ) ) ;
#31882 = VERTEX_POINT ( 'NONE', #41610 ) ;
#31884 = CYLINDRICAL_SURFACE ( 'NONE', #35972, 2.649999999999957723 ) ;
#31883 = CARTESIAN_POINT ( 'NONE',  ( 0.000000000000000000, 31.48608500567870294, 0.9019157472705636724 ) ) ;
#31885 = AXIS2_PLACEMENT_3D ( 'NONE', #1581, #41727, #15156 ) ;
#31886 = EDGE_CURVE ( 'NONE', #19539, #29967, #26110, .T. ) ;
#31887 = ORIENTED_EDGE ( 'NONE', *, *, #4431, .F. ) ;
#31888 = CARTESIAN_POINT ( 'NONE',  ( 52.68777711438346500, 40.00000000000000000, 17.88338314711659294 ) ) ;
#31889 = DIRECTION ( 'NONE',  ( 1.000000000000000000, -1.373900992973642263E-15, -3.016910393003158636E-16 ) ) ;
#31890 = CARTESIAN_POINT ( 'NONE',  ( 0.000000000000000000, -29.09613215194497826, 21.19941258140312002 ) ) ;
#31891 = AXIS2_PLACEMENT_3D ( 'NONE', #9448, #22804, #22585 ) ;
#31892 = CARTESIAN_POINT ( 'NONE',  ( 0.000000000000000000, 0.000000000000000000, -4.484454397937119197 ) ) ;
#31893 = CARTESIAN_POINT ( 'NONE',  ( 14.35450763783260797, 31.00000000000000355, -18.72194639494853874 ) ) ;
#31894 = AXIS2_PLACEMENT_3D ( 'NONE', #18145, #40544, #27065 ) ;
#31895 = AXIS2_PLACEMENT_3D ( 'NONE', #23821, #33818, #24264 ) ;
#31896 = VERTEX_POINT ( 'NONE', #21385 ) ;
#31897 = CARTESIAN_POINT ( 'NONE',  ( 2.454369252093185239, 40.00000000000000000, 37.39583333513270702 ) ) ;
#31898 = ORIENTED_EDGE ( 'NONE', *, *, #39918, .F. ) ;
#31899 = AXIS2_PLACEMENT_3D ( 'NONE', #12927, #40370, #26235 ) ;
#31900 = DIRECTION ( 'NONE',  ( -1.000000000000000000, 0.000000000000000000, -0.000000000000000000 ) ) ;
#31901 = FACE_OUTER_BOUND ( 'NONE', #31988, .T. ) ;
#31902 = CIRCLE ( 'NONE', #17327, 120.5010000000000474 ) ;
#31903 = EDGE_CURVE ( 'NONE', #25511, #2475, #23349, .T. ) ;
#31904 = VERTEX_POINT ( 'NONE', #31377 ) ;
#31905 = EDGE_CURVE ( 'NONE', #16730, #34938, #14275, .T. ) ;
#31906 = LINE ( 'NONE', #28639, #41688 ) ;
#31907 = EDGE_CURVE ( 'NONE', #21438, #40692, #21603, .T. ) ;
#31908 = EDGE_CURVE ( 'NONE', #14639, #37442, #15030, .T. ) ;
#31909 = DIRECTION ( 'NONE',  ( -1.000000000000000000, 0.000000000000000000, 0.000000000000000000 ) ) ;
#31910 = ORIENTED_EDGE ( 'NONE', *, *, #18614, .T. ) ;
#31911 = CARTESIAN_POINT ( 'NONE',  ( 17.99999999999999645, 92.25992191227497585, -77.51514567967304004 ) ) ;
#31912 = EDGE_LOOP ( 'NONE', ( #6990, #33418, #23251, #490 ) ) ;
#31913 = ORIENTED_EDGE ( 'NONE', *, *, #22193, .T. ) ;
#31914 = DIRECTION ( 'NONE',  ( -1.000000000000000000, 0.000000000000000000, 0.000000000000000000 ) ) ;
#31915 = CARTESIAN_POINT ( 'NONE',  ( -21.69137426901471954, 31.00000000000000355, -81.42030341110597647 ) ) ;
#31916 = VERTEX_POINT ( 'NONE', #36125 ) ;
#31917 = CARTESIAN_POINT ( 'NONE',  ( 18.00000000000000355, 0.000000000000000000, 0.000000000000000000 ) ) ;
#31918 = CARTESIAN_POINT ( 'NONE',  ( 0.000000000000000000, 63.55543939553766108, 97.03971415477347762 ) ) ;
#31919 = VERTEX_POINT ( 'NONE', #16301 ) ;
#31920 = CARTESIAN_POINT ( 'NONE',  ( 4.198928548860774157, -0.8158838809860124996, -3.526471437616918170 ) ) ;
#31921 = CARTESIAN_POINT ( 'NONE',  ( 9.000000000000001776, -115.9750404417044223, 2.406240749597103434 ) ) ;
#31922 = CARTESIAN_POINT ( 'NONE',  ( 26.53203760875093309, 31.00000000000000355, 7.134992448514335450 ) ) ;
#31923 = CIRCLE ( 'NONE', #11765, 1.999999999999988010 ) ;
#31925 = CARTESIAN_POINT ( 'NONE',  ( 18.00000000000000355, -40.47821179127736713, 32.64221760512744908 ) ) ;
#31924 = CARTESIAN_POINT ( 'NONE',  ( 17.99999999999999645, -19.69434969228056787, -24.58291258574069360 ) ) ;
#31926 = CARTESIAN_POINT ( 'NONE',  ( 5.200000000000002842, 0.000000000000000000, 0.000000000000000000 ) ) ;
#31927 = DIRECTION ( 'NONE',  ( 0.000000000000000000, 0.000000000000000000, 1.000000000000000000 ) ) ;
#31928 = AXIS2_PLACEMENT_3D ( 'NONE', #16785, #30072, #13494 ) ;
#31929 = EDGE_LOOP ( 'NONE', ( #8203, #31355, #43091, #21934 ) ) ;
#31930 = AXIS2_PLACEMENT_3D ( 'NONE', #32404, #41994, #41578 ) ;
#31931 = PRESENTATION_STYLE_ASSIGNMENT (( #1804 ) ) ;
#31932 = EDGE_CURVE ( 'NONE', #14426, #9049, #30042, .T. ) ;
#31933 = VECTOR ( 'NONE', #1825, 1000.000000000000000 ) ;
#31934 = ORIENTED_EDGE ( 'NONE', *, *, #14326, .F. ) ;
#31935 = CARTESIAN_POINT ( 'NONE',  ( 17.99999999999999645, -7.749090474611724844, 30.53094492177211094 ) ) ;
#31936 = CARTESIAN_POINT ( 'NONE',  ( -6.381360069252544953, 31.00000000000000355, 97.60416666604666602 ) ) ;
#31937 = ADVANCED_FACE ( 'NONE', ( #12597 ), #16751, .F. ) ;
#31938 = DIRECTION ( 'NONE',  ( -1.000000000000000000, -0.000000000000000000, -0.000000000000000000 ) ) ;
#31940 = VERTEX_POINT ( 'NONE', #29834 ) ;
#31939 = CIRCLE ( 'NONE', #13134, 142.5000000000000284 ) ;
#31941 = CARTESIAN_POINT ( 'NONE',  ( -28.63582912838407069, 40.00000000000000000, 7.677129336082076705 ) ) ;
#31942 = CARTESIAN_POINT ( 'NONE',  ( -35.75974951333986240, 40.00000000000000000, 20.56794350806610794 ) ) ;
#31943 = ORIENTED_EDGE ( 'NONE', *, *, #5779, .F. ) ;
#31944 = ORIENTED_EDGE ( 'NONE', *, *, #10617, .F. ) ;
#31945 = DIRECTION ( 'NONE',  ( 2.731800627175558911E-17, 1.000000000000000000, -3.170996607629411740E-18 ) ) ;
#31946 = DIRECTION ( 'NONE',  ( -1.000000000000000000, 0.000000000000000000, 0.000000000000000000 ) ) ;
#31947 = CARTESIAN_POINT ( 'NONE',  ( 7.000000000000006217, 7.118024431592600946E-15, 0.000000000000000000 ) ) ;
#31948 = CARTESIAN_POINT ( 'NONE',  ( -2.682243648011671588, -3.070208061305317759, -0.04852650426602272971 ) ) ;
#31949 = CARTESIAN_POINT ( 'NONE',  ( -10.00000000000000000, 0.000000000000000000, 0.000000000000000000 ) ) ;
#31950 = ORIENTED_EDGE ( 'NONE', *, *, #7219, .F. ) ;
#31951 = FACE_OUTER_BOUND ( 'NONE', #28937, .T. ) ;
#31952 = ORIENTED_EDGE ( 'NONE', *, *, #18892, .F. ) ;
#31953 = DIRECTION ( 'NONE',  ( 0.000000000000000000, 0.8993121301712173610, 0.4373073204588593388 ) ) ;
#31954 = DIRECTION ( 'NONE',  ( -1.000000000000000000, -0.000000000000000000, -0.000000000000000000 ) ) ;
#31955 = EDGE_CURVE ( 'NONE', #3154, #11369, #25442, .T. ) ;
#31956 = ADVANCED_FACE ( 'NONE', ( #16531 ), #26542, .T. ) ;
#31957 = VECTOR ( 'NONE', #13503, 1000.000000000000000 ) ;
#31958 = CARTESIAN_POINT ( 'NONE',  ( 0.000000000000000000, -117.6086855750636460, 26.24286718912064487 ) ) ;
#31959 = EDGE_CURVE ( 'NONE', #8862, #40989, #91, .T. ) ;
#31960 = ADVANCED_FACE ( 'NONE', ( #39814 ), #2731, .F. ) ;
#31961 = DIRECTION ( 'NONE',  ( 0.000000000000000000, -0.9213119778704086382, -0.3888241754733309241 ) ) ;
#31962 = ORIENTED_EDGE ( 'NONE', *, *, #42790, .T. ) ;
#31963 = VERTEX_POINT ( 'NONE', #9941 ) ;
#31964 = CIRCLE ( 'NONE', #26416, 59.00000000000000000 ) ;
#31965 = CYLINDRICAL_SURFACE ( 'NONE', #10271, 1.999999999999988010 ) ;
#31966 = EDGE_CURVE ( 'NONE', #3869, #37135, #7992, .T. ) ;
#31967 = AXIS2_PLACEMENT_3D ( 'NONE', #6378, #19949, #3515 ) ;
#31968 = ORIENTED_EDGE ( 'NONE', *, *, #24054, .F. ) ;
#31970 = ORIENTED_EDGE ( 'NONE', *, *, #34295, .F. ) ;
#31969 = DIRECTION ( 'NONE',  ( -1.000000000000000000, -0.000000000000000000, -0.000000000000000000 ) ) ;
#31971 = CARTESIAN_POINT ( 'NONE',  ( 51.84393115708665079, 31.00000000000000355, 25.66707601012906892 ) ) ;
#31972 = ORIENTED_EDGE ( 'NONE', *, *, #6434, .F. ) ;
#31973 = DIRECTION ( 'NONE',  ( 0.000000000000000000, 0.000000000000000000, -1.000000000000000000 ) ) ;
#31974 = FACE_OUTER_BOUND ( 'NONE', #545, .T. ) ;
#31975 = VERTEX_POINT ( 'NONE', #42877 ) ;
#31976 = CARTESIAN_POINT ( 'NONE',  ( 34.31975892712151222, 40.00000000000000000, 59.64049725130580271 ) ) ;
#31977 = CYLINDRICAL_SURFACE ( 'NONE', #37400, 59.00000000000000000 ) ;
#31978 = LINE ( 'NONE', #1631, #34520 ) ;
#31979 = ORIENTED_EDGE ( 'NONE', *, *, #4888, .F. ) ;
#31980 = CARTESIAN_POINT ( 'NONE',  ( 17.99999999999999645, -29.36437154451924059, -116.8684075565139295 ) ) ;
#31981 = ORIENTED_EDGE ( 'NONE', *, *, #5272, .T. ) ;
#31982 = CARTESIAN_POINT ( 'NONE',  ( -4.121423858225412573, -12.61643262889541184, -1.199999999999999956 ) ) ;
#31983 = DIRECTION ( 'NONE',  ( 0.000000000000000000, 0.000000000000000000, 1.000000000000000000 ) ) ;
#31984 = CARTESIAN_POINT ( 'NONE',  ( -54.82550897924149069, 31.00000000000000711, 42.06954809655981364 ) ) ;
#31985 = CIRCLE ( 'NONE', #18795, 19.19999999999999574 ) ;
#31986 = LINE ( 'NONE', #22408, #19791 ) ;
#31987 = AXIS2_PLACEMENT_3D ( 'NONE', #36323, #36117, #29822 ) ;
#31988 = EDGE_LOOP ( 'NONE', ( #42009, #28556, #41684, #30702 ) ) ;
#31989 = CIRCLE ( 'NONE', #22958, 4.500000000000002665 ) ;
#31990 = SURFACE_STYLE_FILL_AREA ( #13005 ) ;
#31991 = VERTEX_POINT ( 'NONE', #39387 ) ;
#31992 = DIRECTION ( 'NONE',  ( 0.000000000000000000, 0.3681245526846785854, -0.9297764858882511252 ) ) ;
#31993 = CARTESIAN_POINT ( 'NONE',  ( 17.99999999999999645, 18.35539002514383711, 110.6858262410710410 ) ) ;
#31994 = CARTESIAN_POINT ( 'NONE',  ( -5.410573124821301150, 31.00000000000000355, -84.40011308935179102 ) ) ;
#31995 = CARTESIAN_POINT ( 'NONE',  ( -26.95034633362163845, 40.00000000000000000, -79.72278128421112342 ) ) ;
#31996 = CYLINDRICAL_SURFACE ( 'NONE', #37625, 20.00000000000000711 ) ;
#31997 = ORIENTED_EDGE ( 'NONE', *, *, #736, .F. ) ;
#31998 = DIRECTION ( 'NONE',  ( -1.000000000000000000, -0.000000000000000000, -0.000000000000000000 ) ) ;
#31999 = ORIENTED_EDGE ( 'NONE', *, *, #13677, .T. ) ;
#32000 = FACE_OUTER_BOUND ( 'NONE', #1431, .T. ) ;
#32001 = FACE_OUTER_BOUND ( 'NONE', #9241, .T. ) ;
#32003 = ORIENTED_EDGE ( 'NONE', *, *, #27934, .T. ) ;
#32002 = DIRECTION ( 'NONE',  ( 0.000000000000000000, 0.05322217484217219019, 0.9985826956767622775 ) ) ;
#32004 = EDGE_CURVE ( 'NONE', #38581, #41253, #24766, .T. ) ;
#32005 = EDGE_CURVE ( 'NONE', #26722, #6283, #41430, .T. ) ;
#32006 = DIRECTION ( 'NONE',  ( 0.000000000000000000, -0.1062934856473523454, -0.9943348002101385363 ) ) ;
#32007 = ORIENTED_EDGE ( 'NONE', *, *, #19819, .F. ) ;
#32008 = CARTESIAN_POINT ( 'NONE',  ( 17.99999999999999645, -75.03166794516862126, 94.29071961951481740 ) ) ;
#32009 = PLANE ( 'NONE',  #40177 ) ;
#32010 = ADVANCED_FACE ( 'NONE', ( #29605 ), #39610, .T. ) ;
#32011 = DIRECTION ( 'NONE',  ( -1.000000000000000000, 0.000000000000000000, 0.000000000000000000 ) ) ;
#32012 = ORIENTED_EDGE ( 'NONE', *, *, #24388, .F. ) ;
#32013 = CARTESIAN_POINT ( 'NONE',  ( 27.10182830755124428, 31.00000000000000355, 1.799748011963437033 ) ) ;
#32014 = VECTOR ( 'NONE', #3319, 1000.000000000000000 ) ;
#32015 = DIRECTION ( 'NONE',  ( 0.000000000000000000, -0.2113826236296113270, -0.9774033898178695612 ) ) ;
#32016 = CIRCLE ( 'NONE', #22981, 11.00000000000000000 ) ;
#32017 = VECTOR ( 'NONE', #20173, 1000.000000000000000 ) ;
#32018 = EDGE_CURVE ( 'NONE', #40947, #239, #36543, .T. ) ;
#32020 = DIRECTION ( 'NONE',  ( 0.000000000000000000, 0.000000000000000000, 1.000000000000000000 ) ) ;
#32019 = CYLINDRICAL_SURFACE ( 'NONE', #30669, 142.4999999999992610 ) ;
#32021 = ORIENTED_EDGE ( 'NONE', *, *, #3613, .F. ) ;
#32022 = CARTESIAN_POINT ( 'NONE',  ( 2.100000000000000089, 0.000000000000000000, -4.694516984716113228 ) ) ;
#32023 = CARTESIAN_POINT ( 'NONE',  ( -106.4195705685741871, -106.4195705685773135, 9.999999999999751310 ) ) ;
#32024 = CARTESIAN_POINT ( 'NONE',  ( 19.31996883371318674, 40.00000000000000000, 33.58758284028577634 ) ) ;
#32025 = DIRECTION ( 'NONE',  ( -1.000000000000000000, 0.000000000000000000, -0.000000000000000000 ) ) ;
#32026 = EDGE_CURVE ( 'NONE', #11221, #21496, #6609, .T. ) ;
#32027 = FACE_OUTER_BOUND ( 'NONE', #1317, .T. ) ;
#32028 = DIRECTION ( 'NONE',  ( 0.000000000000000000, 0.000000000000000000, 1.000000000000000000 ) ) ;
#32029 = ORIENTED_EDGE ( 'NONE', *, *, #40844, .F. ) ;
#32030 = DIRECTION ( 'NONE',  ( -1.000000000000000000, -0.000000000000000000, -0.000000000000000000 ) ) ;
#32031 = VERTEX_POINT ( 'NONE', #15886 ) ;
#32032 = DIRECTION ( 'NONE',  ( 1.000000000000000000, 0.000000000000000000, 0.000000000000000000 ) ) ;
#32033 = CARTESIAN_POINT ( 'NONE',  ( 8.999999999999998224, -83.58328028049714931, 80.43528614701294543 ) ) ;
#32034 = CARTESIAN_POINT ( 'NONE',  ( 14.71924655979513297, 31.00000000000000355, -29.87007926703815741 ) ) ;
#32035 = ORIENTED_EDGE ( 'NONE', *, *, #34704, .T. ) ;
#32036 = DIRECTION ( 'NONE',  ( 0.000000000000000000, 0.7525707698561399095, -0.6585113790650372056 ) ) ;
#32037 = ORIENTED_EDGE ( 'NONE', *, *, #21847, .T. ) ;
#32038 = CONTEXT_DEPENDENT_SHAPE_REPRESENTATION ( #36776, #15564 ) ;
#32039 = CARTESIAN_POINT ( 'NONE',  ( 4.000000000000000000, -1.942223658245635809, -0.3516579909967643691 ) ) ;
#32040 = CARTESIAN_POINT ( 'NONE',  ( 55.27058341129635721, 31.00000000000000000, -63.02248852588876105 ) ) ;
#32041 = CIRCLE ( 'NONE', #41805, 51.99999999999999289 ) ;
#32042 = ORIENTED_EDGE ( 'NONE', *, *, #39207, .T. ) ;
#32043 = CARTESIAN_POINT ( 'NONE',  ( 29.31577600746836154, 31.00000000000000355, 50.95836110721448620 ) ) ;
#32044 = CARTESIAN_POINT ( 'NONE',  ( 46.76839422406115432, 39.99999999999999289, -81.00140361174831583 ) ) ;
#32045 = ORIENTED_EDGE ( 'NONE', *, *, #3610, .F. ) ;
#32046 = CARTESIAN_POINT ( 'NONE',  ( 17.99999999999999645, -88.56657216608662964, 68.87840567545892156 ) ) ;
#32047 = LINE ( 'NONE', #1496, #16626 ) ;
#32048 = DIRECTION ( 'NONE',  ( 0.000000000000000000, 0.000000000000000000, 1.000000000000000000 ) ) ;
#32050 = ORIENTED_EDGE ( 'NONE', *, *, #22193, .F. ) ;
#32049 = DIRECTION ( 'NONE',  ( 0.000000000000000000, 0.000000000000000000, 1.000000000000000000 ) ) ;
#32051 = EDGE_CURVE ( 'NONE', #13471, #41650, #39361, .T. ) ;
#32052 = CYLINDRICAL_SURFACE ( 'NONE', #26087, 59.00000000000000711 ) ;
#32053 = CARTESIAN_POINT ( 'NONE',  ( -10.00000000000000000, 0.000000000000000000, 0.000000000000000000 ) ) ;
#32054 = EDGE_CURVE ( 'NONE', #31287, #3430, #22703, .T. ) ;
#32055 = PRODUCT_DEFINITION ( 'UNKNOWN', '', #20536, #3803 ) ;
#32056 = ORIENTED_EDGE ( 'NONE', *, *, #35907, .F. ) ;
#32057 = CARTESIAN_POINT ( 'NONE',  ( -62.26029918285335896, 40.00000000000000711, 30.70375207684418228 ) ) ;
#32058 = DIRECTION ( 'NONE',  ( 0.000000000000000000, -0.6382441836448262684, 0.7698339834299010587 ) ) ;
#32059 = EDGE_LOOP ( 'NONE', ( #14890, #23549, #13993, #27451 ) ) ;
#32060 = CARTESIAN_POINT ( 'NONE',  ( 142.5000000000000284, 0.000000000000000000, -25.00000000000000000 ) ) ;
#32061 = ADVANCED_FACE ( 'NONE', ( #22655 ), #35899, .F. ) ;
#32062 = LINE ( 'NONE', #8497, #16602 ) ;
#32063 = ORIENTED_EDGE ( 'NONE', *, *, #20409, .T. ) ;
#32064 = EDGE_CURVE ( 'NONE', #2350, #32806, #35875, .T. ) ;
#32065 = VERTEX_POINT ( 'NONE', #312 ) ;
#32066 = CARTESIAN_POINT ( 'NONE',  ( 17.99999999999999645, -16.77727049691090500, -27.19001440037564166 ) ) ;
#32068 = ORIENTED_EDGE ( 'NONE', *, *, #5348, .F. ) ;
#32067 = AXIS2_PLACEMENT_3D ( 'NONE', #29966, #37285, #29748 ) ;
#32069 = CARTESIAN_POINT ( 'NONE',  ( 17.99999999999999645, 12.43843445475471832, -111.5058645182328405 ) ) ;
#32070 = AXIS2_PLACEMENT_3D ( 'NONE', #13924, #23536, #30912 ) ;
#32071 = CYLINDRICAL_SURFACE ( 'NONE', #20725, 47.49900000000000233 ) ;
#32072 = EDGE_CURVE ( 'NONE', #32077, #37143, #1028, .T. ) ;
#32073 = AXIS2_PLACEMENT_3D ( 'NONE', #38429, #37786, #14486 ) ;
#32074 = DIRECTION ( 'NONE',  ( 0.000000000000000000, -0.6736956436465638687, 0.7390089172206529833 ) ) ;
#32075 = CIRCLE ( 'NONE', #31692, 20.00000000000000355 ) ;
#32076 = DIRECTION ( 'NONE',  ( 0.000000000000000000, 0.3681245526846786964, -0.9297764858882511252 ) ) ;
#32077 = VERTEX_POINT ( 'NONE', #41056 ) ;
#32078 = FACE_OUTER_BOUND ( 'NONE', #14286, .T. ) ;
#32079 = ORIENTED_EDGE ( 'NONE', *, *, #963, .T. ) ;
#32080 = DIRECTION ( 'NONE',  ( -1.000000000000000000, 0.000000000000000000, -0.000000000000000000 ) ) ;
#32081 = ORIENTED_EDGE ( 'NONE', *, *, #29985, .F. ) ;
#32082 = CARTESIAN_POINT ( 'NONE',  ( 0.000000000000000000, 27.83061035786954918, 117.2431154827798281 ) ) ;
#32083 = DIRECTION ( 'NONE',  ( -1.000000000000000000, -0.000000000000000000, -0.000000000000000000 ) ) ;
#32084 = EDGE_CURVE ( 'NONE', #26722, #31096, #34751, .T. ) ;
#32085 = DIRECTION ( 'NONE',  ( -1.000000000000000000, -0.000000000000000000, -0.000000000000000000 ) ) ;
#32086 = CARTESIAN_POINT ( 'NONE',  ( 44.91824650936478491, 31.00000000000000355, 5.910997147197376123 ) ) ;
#32087 = EDGE_CURVE ( 'NONE', #41253, #34763, #16386, .T. ) ;
#32088 = ORIENTED_EDGE ( 'NONE', *, *, #32051, .T. ) ;
#32089 = DIRECTION ( 'NONE',  ( -0.000000000000000000, 1.000000000000000000, 1.224646799147353207E-16 ) ) ;
#32090 = VECTOR ( 'NONE', #31652, 1000.000000000000000 ) ;
#32091 = EDGE_CURVE ( 'NONE', #30296, #31298, #16961, .T. ) ;
#32092 = ORIENTED_EDGE ( 'NONE', *, *, #21258, .T. ) ;
#32093 = CARTESIAN_POINT ( 'NONE',  ( 20.30000058474805869, 40.00000000000000000, -59.80472289869057789 ) ) ;
#32094 = AXIS2_PLACEMENT_3D ( 'NONE', #38977, #25924, #19596 ) ;
#32095 = AXIS2_PLACEMENT_3D ( 'NONE', #31373, #1456, #42021 ) ;
#32096 = AXIS2_PLACEMENT_3D ( 'NONE', #13457, #16955, #26970 ) ;
#32097 = DIRECTION ( 'NONE',  ( 0.000000000000000000, 0.000000000000000000, 1.000000000000000000 ) ) ;
#32098 = CARTESIAN_POINT ( 'NONE',  ( 17.99999999999999645, 0.000000000000000000, 0.000000000000000000 ) ) ;
#32099 = VECTOR ( 'NONE', #12228, 1000.000000000000000 ) ;
#32100 = AXIS2_PLACEMENT_3D ( 'NONE', #32260, #29220, #38796 ) ;
#32101 = DIRECTION ( 'NONE',  ( -1.000000000000000000, -0.000000000000000000, -0.000000000000000000 ) ) ;
#32102 = DIRECTION ( 'NONE',  ( 3.996523416598930318E-16, -2.658563593772947863E-15, -1.000000000000000000 ) ) ;
#32103 = EDGE_CURVE ( 'NONE', #21287, #14763, #27539, .T. ) ;
#32104 = EDGE_LOOP ( 'NONE', ( #19904, #13524, #12990, #12559 ) ) ;
#32105 = CARTESIAN_POINT ( 'NONE',  ( 16.69935377588158332, 40.00000000000000000, -28.93150767131472989 ) ) ;
#32106 = ORIENTED_EDGE ( 'NONE', *, *, #19041, .T. ) ;
#32107 = DIRECTION ( 'NONE',  ( -3.009274222672345096E-17, -1.000000000000000000, 2.455023325076454960E-18 ) ) ;
#32108 = CYLINDRICAL_SURFACE ( 'NONE', #6843, 13.60000000000000142 ) ;
#32109 = ORIENTED_EDGE ( 'NONE', *, *, #41049, .T. ) ;
#32110 = CARTESIAN_POINT ( 'NONE',  ( 17.99999999999999645, -87.74575819880118388, -75.87280091124561920 ) ) ;
#32111 = ORIENTED_EDGE ( 'NONE', *, *, #885, .F. ) ;
#32112 = DIRECTION ( 'NONE',  ( 1.000000000000000000, 0.000000000000000000, 0.000000000000000000 ) ) ;
#32113 = ORIENTED_EDGE ( 'NONE', *, *, #13591, .T. ) ;
#32114 = ADVANCED_FACE ( 'NONE', ( #40025 ), #24984, .F. ) ;
#32115 = VERTEX_POINT ( 'NONE', #26977 ) ;
#32116 = DIRECTION ( 'NONE',  ( -1.000000000000000000, -0.000000000000000000, -0.000000000000000000 ) ) ;
#32117 = CARTESIAN_POINT ( 'NONE',  ( -25.88810397299713628, 31.00000000000000355, 75.89534075019484760 ) ) ;
#32118 = ORIENTED_EDGE ( 'NONE', *, *, #27351, .T. ) ;
#32119 = FACE_OUTER_BOUND ( 'NONE', #31131, .T. ) ;
#32120 = CIRCLE ( 'NONE', #29, 120.5010000000000332 ) ;
#32121 = CARTESIAN_POINT ( 'NONE',  ( 17.99999999999999645, -107.2885202478269946, 54.86040852957277281 ) ) ;
#32122 = ORIENTED_EDGE ( 'NONE', *, *, #41850, .T. ) ;
#32123 = CARTESIAN_POINT ( 'NONE',  ( 17.99999999999999645, 98.39501399267960835, 53.91376164787712355 ) ) ;
#32124 = CARTESIAN_POINT ( 'NONE',  ( -32.34013556242301490, 40.00000000000000000, 94.87070470178476000 ) ) ;
#32125 = AXIS2_PLACEMENT_3D ( 'NONE', #22819, #6190, #12548 ) ;
#32126 = CARTESIAN_POINT ( 'NONE',  ( -80.34276469473088866, 40.00000000000000711, 61.48650092628135866 ) ) ;
#32128 = FACE_OUTER_BOUND ( 'NONE', #21824, .T. ) ;
#32127 = FACE_OUTER_BOUND ( 'NONE', #25643, .T. ) ;
#32129 = CIRCLE ( 'NONE', #34234, 116.0000000000000000 ) ;
#32130 = LINE ( 'NONE', #24549, #15798 ) ;
#32131 = DIRECTION ( 'NONE',  ( 1.000000000000000000, 0.000000000000000000, 0.000000000000000000 ) ) ;
#32132 = EDGE_LOOP ( 'NONE', ( #33536, #9467, #40603, #29958 ) ) ;
#32133 = DIRECTION ( 'NONE',  ( 1.000000000000000000, 0.000000000000000000, 0.000000000000000000 ) ) ;
#32134 = EDGE_CURVE ( 'NONE', #35058, #28496, #4633, .T. ) ;
#32135 = AXIS2_PLACEMENT_3D ( 'NONE', #15948, #16151, #42080 ) ;
#32136 = EDGE_LOOP ( 'NONE', ( #29090, #4880, #19655, #6798 ) ) ;
#32137 = CARTESIAN_POINT ( 'NONE',  ( 0.000000000000000000, -34.74871106919551522, -106.6808302961375148 ) ) ;
#32138 = EDGE_CURVE ( 'NONE', #27302, #30882, #5223, .T. ) ;
#32139 = DIRECTION ( 'NONE',  ( -1.000000000000000000, -0.000000000000000000, 0.000000000000000000 ) ) ;
#32140 = ORIENTED_EDGE ( 'NONE', *, *, #30681, .T. ) ;
#32141 = CARTESIAN_POINT ( 'NONE',  ( -27.62299686580952240, 40.00000000000000000, -13.61136854378590577 ) ) ;
#32142 = CARTESIAN_POINT ( 'NONE',  ( -40.27082278478597033, 40.00000000000000000, 10.71261860272680977 ) ) ;
#32143 = ORIENTED_EDGE ( 'NONE', *, *, #30689, .T. ) ;
#32144 = ORIENTED_EDGE ( 'NONE', *, *, #19851, .F. ) ;
#32145 = CARTESIAN_POINT ( 'NONE',  ( 150.5000000000000284, 1.576403824487674918E-12, 10.00000000000000000 ) ) ;
#32146 = CARTESIAN_POINT ( 'NONE',  ( -2.000000000000006661, 3.464101615137750834, 0.000000000000000000 ) ) ;
#32147 =( NAMED_UNIT ( * ) SI_UNIT ( $, .STERADIAN. ) SOLID_ANGLE_UNIT ( ) );
#32148 = CARTESIAN_POINT ( 'NONE',  ( 17.99999999999999645, 0.000000000000000000, 0.000000000000000000 ) ) ;
#32149 = EDGE_CURVE ( 'NONE', #27071, #29862, #36987, .T. ) ;
#32150 = DIRECTION ( 'NONE',  ( 0.000000000000000000, 0.000000000000000000, 1.000000000000000000 ) ) ;
#32151 = ORIENTED_EDGE ( 'NONE', *, *, #28284, .F. ) ;
#32152 = DIRECTION ( 'NONE',  ( 0.000000000000000000, 0.000000000000000000, 1.000000000000000000 ) ) ;
#32153 = ORIENTED_EDGE ( 'NONE', *, *, #37368, .F. ) ;
#32154 = CARTESIAN_POINT ( 'NONE',  ( 0.000000000000000000, 83.49789599728902090, -86.88263557826680028 ) ) ;
#32155 = CIRCLE ( 'NONE', #14773, 36.00000000000000000 ) ;
#32156 = DIRECTION ( 'NONE',  ( -0.7071067811865364705, 0.000000000000000000, 0.7071067811865584529 ) ) ;
#32157 = AXIS2_PLACEMENT_3D ( 'NONE', #29492, #19266, #32540 ) ;
#32158 = LINE ( 'NONE', #9024, #22860 ) ;
#32159 = FACE_BOUND ( 'NONE', #15517, .T. ) ;
#32160 = VERTEX_POINT ( 'NONE', #14491 ) ;
#32161 = ORIENTED_EDGE ( 'NONE', *, *, #3057, .F. ) ;
#32162 = CARTESIAN_POINT ( 'NONE',  ( 0.000000000000000000, -19.74581912682808493, -48.10512059033413834 ) ) ;
#32163 = EDGE_CURVE ( 'NONE', #36189, #40193, #13464, .T. ) ;
#32164 = AXIS2_PLACEMENT_3D ( 'NONE', #28919, #24649, #14170 ) ;
#32165 = ORIENTED_EDGE ( 'NONE', *, *, #37005, .T. ) ;
#32167 = ORIENTED_EDGE ( 'NONE', *, *, #9084, .T. ) ;
#32166 = CARTESIAN_POINT ( 'NONE',  ( 18.00000000000000355, -15.49408907645202937, 44.90087086784588166 ) ) ;
#32168 = CARTESIAN_POINT ( 'NONE',  ( 57.09498703527648900, 31.00000000000000355, 3.831922229400927637 ) ) ;
#32169 = EDGE_CURVE ( 'NONE', #3831, #25049, #25473, .T. ) ;
#32170 = VERTEX_POINT ( 'NONE', #18218 ) ;
#32171 = DIRECTION ( 'NONE',  ( 0.000000000000000000, -0.9968120070307493474, -0.07978610555309334496 ) ) ;
#32172 = FACE_BOUND ( 'NONE', #875, .T. ) ;
#32173 = PRODUCT_DEFINITION_SHAPE ( 'NONE', 'NONE',  #43200 ) ;
#32174 = ORIENTED_EDGE ( 'NONE', *, *, #8131, .T. ) ;
#32175 = CARTESIAN_POINT ( 'NONE',  ( -63.15125318177969405, 40.00000000000000711, -36.59163237596791163 ) ) ;
#32177 = LINE ( 'NONE', #17360, #35322 ) ;
#32176 = DIRECTION ( 'NONE',  ( 0.000000000000000000, 0.9510565162951521989, 0.3090169943749515036 ) ) ;
#32178 = DIRECTION ( 'NONE',  ( -1.000000000000000000, -0.000000000000000000, 0.000000000000000000 ) ) ;
#32179 = EDGE_LOOP ( 'NONE', ( #14151, #2834, #35636, #36183 ) ) ;
#32180 = LINE ( 'NONE', #32815, #14737 ) ;
#32181 = ORIENTED_EDGE ( 'NONE', *, *, #191, .T. ) ;
#32182 = AXIS2_PLACEMENT_3D ( 'NONE', #17304, #13147, #6992 ) ;
#32183 = DIRECTION ( 'NONE',  ( 1.000000000000000000, 0.000000000000000000, -6.546126324440832913E-16 ) ) ;
#32184 = FACE_BOUND ( 'NONE', #5334, .T. ) ;
#32185 = AXIS2_PLACEMENT_3D ( 'NONE', #18119, #29394, #39388 ) ;
#32186 = ADVANCED_FACE ( 'NONE', ( #1574 ), #27802, .T. ) ;
#32187 = CARTESIAN_POINT ( 'NONE',  ( -68.16583574478268304, 31.00000000000000711, -18.25112749842637427 ) ) ;
#32188 = EDGE_CURVE ( 'NONE', #30917, #12490, #5924, .T. ) ;
#32190 = CARTESIAN_POINT ( 'NONE',  ( 17.99999999999999645, 57.69704296431325474, -105.7900857083224224 ) ) ;
#32189 = DIRECTION ( 'NONE',  ( 0.9396926207859138680, 1.150791560227856926E-16, -0.3420201433256536139 ) ) ;
#32191 = ORIENTED_EDGE ( 'NONE', *, *, #19700, .T. ) ;
#32192 = EDGE_CURVE ( 'NONE', #14078, #10279, #36561, .T. ) ;
#32193 = EDGE_CURVE ( 'NONE', #1690, #5524, #24540, .T. ) ;
#32194 = AXIS2_PLACEMENT_3D ( 'NONE', #7951, #34569, #31097 ) ;
#32195 = DIRECTION ( 'NONE',  ( 0.000000000000000000, 0.000000000000000000, 1.000000000000000000 ) ) ;
#32196 = ORIENTED_EDGE ( 'NONE', *, *, #14033, .F. ) ;
#32197 = CARTESIAN_POINT ( 'NONE',  ( -10.00000000000000000, 0.000000000000000000, 0.000000000000000000 ) ) ;
#32198 = DIRECTION ( 'NONE',  ( 1.000000000000000000, 0.000000000000000000, 0.000000000000000000 ) ) ;
#32199 = CARTESIAN_POINT ( 'NONE',  ( 84.84057271803867195, 31.00000000000000000, 49.13019966417499518 ) ) ;
#32200 = CARTESIAN_POINT ( 'NONE',  ( -83.29221842949013421, 40.00000000000000711, -41.19657635676244922 ) ) ;
#32201 = DIRECTION ( 'NONE',  ( 0.000000000000000000, -0.9996456111234529596, 0.02662052143776450636 ) ) ;
#32202 = ORIENTED_EDGE ( 'NONE', *, *, #1791, .T. ) ;
#32203 = DIRECTION ( 'NONE',  ( -1.000000000000000000, -0.000000000000000000, -0.000000000000000000 ) ) ;
#32204 = ORIENTED_EDGE ( 'NONE', *, *, #3271, .T. ) ;
#32205 = FACE_OUTER_BOUND ( 'NONE', #1905, .T. ) ;
#32207 = ORIENTED_EDGE ( 'NONE', *, *, #14322, .F. ) ;
#32206 = CARTESIAN_POINT ( 'NONE',  ( 0.000000000000000000, 1.836970198721029589E-15, -15.00000000000000000 ) ) ;
#32208 = FACE_OUTER_BOUND ( 'NONE', #27118, .T. ) ;
#32209 = VERTEX_POINT ( 'NONE', #14707 ) ;
#32210 = CARTESIAN_POINT ( 'NONE',  ( 17.99999999999999645, -69.90696807222417419, -98.15042952503588936 ) ) ;
#32211 = FACE_OUTER_BOUND ( 'NONE', #37617, .T. ) ;
#32212 = AXIS2_PLACEMENT_3D ( 'NONE', #23788, #36842, #3445 ) ;
#32213 = CARTESIAN_POINT ( 'NONE',  ( 17.99999999999999645, -112.1427988504407551, -3.502162136924565239 ) ) ;
#32214 = CIRCLE ( 'NONE', #14836, 59.00000000000000000 ) ;
#32215 = ORIENTED_EDGE ( 'NONE', *, *, #31966, .T. ) ;
#32216 = CARTESIAN_POINT ( 'NONE',  ( 17.33436897218374639, 31.00000000000000355, 22.64673195036552755 ) ) ;
#32217 = EDGE_CURVE ( 'NONE', #12532, #16411, #20580, .T. ) ;
#32218 = CARTESIAN_POINT ( 'NONE',  ( -24.74979319748359785, 5.944745455504278020, 2.972870684497277427 ) ) ;
#32219 = CIRCLE ( 'NONE', #25289, 52.00000000000000000 ) ;
#32220 = EDGE_CURVE ( 'NONE', #38361, #6792, #38659, .T. ) ;
#32222 = ORIENTED_EDGE ( 'NONE', *, *, #5243, .T. ) ;
#32221 = CARTESIAN_POINT ( 'NONE',  ( 0.000000000000000000, 0.000000000000000000, 0.000000000000000000 ) ) ;
#32223 = ORIENTED_EDGE ( 'NONE', *, *, #27740, .T. ) ;
#32224 = CARTESIAN_POINT ( 'NONE',  ( 8.999999999999998224, 23.79363200506992015, -27.01597816121622486 ) ) ;
#32225 = DIRECTION ( 'NONE',  ( 0.000000000000000000, 0.000000000000000000, 1.000000000000000000 ) ) ;
#32227 = CARTESIAN_POINT ( 'NONE',  ( -35.75974951333986240, 40.00000000000000000, 20.56794350806610794 ) ) ;
#32226 = CIRCLE ( 'NONE', #20421, 47.49900000000000233 ) ;
#32228 = DIRECTION ( 'NONE',  ( 0.000000000000000000, 1.881733940042637923E-15, -1.000000000000000000 ) ) ;
#32229 = CARTESIAN_POINT ( 'NONE',  ( 17.99999999999999645, 0.000000000000000000, 0.000000000000000000 ) ) ;
#32230 = CYLINDRICAL_SURFACE ( 'NONE', #31806, 120.5010000000000190 ) ;
#32231 = VERTEX_POINT ( 'NONE', #31918 ) ;
#32232 = CARTESIAN_POINT ( 'NONE',  ( -0.6448876103708541807, -4.246476118072358474, -0.2256878752776773356 ) ) ;
#32233 = VERTEX_POINT ( 'NONE', #32121 ) ;
#32234 = CYLINDRICAL_SURFACE ( 'NONE', #25311, 59.00000000000000000 ) ;
#32235 = FACE_OUTER_BOUND ( 'NONE', #8691, .T. ) ;
#32236 = CARTESIAN_POINT ( 'NONE',  ( -33.98628324864968420, 31.00000000000000355, 19.63407011443918293 ) ) ;
#32237 = ORIENTED_EDGE ( 'NONE', *, *, #23747, .F. ) ;
#32238 = SURFACE_SIDE_STYLE ('',( #11990 ) ) ;
#32239 = ORIENTED_EDGE ( 'NONE', *, *, #39664, .F. ) ;
#32240 = EDGE_CURVE ( 'NONE', #31896, #35898, #17819, .T. ) ;
#32241 = EDGE_CURVE ( 'NONE', #7956, #1973, #3815, .T. ) ;
#32242 = EDGE_CURVE ( 'NONE', #20215, #41335, #19214, .T. ) ;
#32243 = CARTESIAN_POINT ( 'NONE',  ( 8.919999999999994600, 1.836970198721029589E-15, -14.99999999999999822 ) ) ;
#32244 = AXIS2_PLACEMENT_3D ( 'NONE', #9311, #15898, #42252 ) ;
#32245 = CARTESIAN_POINT ( 'NONE',  ( -89.21153162435624040, 31.00000000000000711, 11.76024306507019901 ) ) ;
#32246 = CARTESIAN_POINT ( 'NONE',  ( 0.000000000000000000, 11.90021268425617329, -45.45261810511203038 ) ) ;
#32247 = ORIENTED_EDGE ( 'NONE', *, *, #32138, .F. ) ;
#32248 = CARTESIAN_POINT ( 'NONE',  ( -52.09564885853935579, 31.00000000000000355, -3.498939618562641574 ) ) ;
#32249 = ADVANCED_FACE ( 'NONE', ( #12071 ), #42123, .T. ) ;
#32250 = DIRECTION ( 'NONE',  ( 1.000000000000000000, 0.000000000000000000, 0.000000000000000000 ) ) ;
#32251 = ORIENTED_EDGE ( 'NONE', *, *, #12968, .F. ) ;
#32252 = AXIS2_PLACEMENT_3D ( 'NONE', #40746, #10898, #27703 ) ;
#32253 = DIRECTION ( 'NONE',  ( -1.000000000000000000, -0.000000000000000000, 0.000000000000000000 ) ) ;
#32254 = EDGE_CURVE ( 'NONE', #18421, #23373, #2404, .T. ) ;
#32255 = CARTESIAN_POINT ( 'NONE',  ( 0.000000000000000000, 0.000000000000000000, 0.000000000000000000 ) ) ;
#32256 = DIRECTION ( 'NONE',  ( 0.000000000000000000, 0.000000000000000000, 1.000000000000000000 ) ) ;
#32258 = ORIENTED_EDGE ( 'NONE', *, *, #3528, .F. ) ;
#32257 = DIRECTION ( 'NONE',  ( 0.000000000000000000, 0.000000000000000000, 1.000000000000000000 ) ) ;
#32259 = DIRECTION ( 'NONE',  ( 0.000000000000000000, 0.000000000000000000, 1.000000000000000000 ) ) ;
#32260 = CARTESIAN_POINT ( 'NONE',  ( -106.4195705685749402, 106.4195705685765745, 10.00000000000033751 ) ) ;
#32261 = ORIENTED_EDGE ( 'NONE', *, *, #23158, .T. ) ;
#32262 = CARTESIAN_POINT ( 'NONE',  ( 72.19657831791809599, 39.99999999999999289, -19.34484491892447622 ) ) ;
#32263 = DIRECTION ( 'NONE',  ( -1.000000000000000000, 0.000000000000000000, 0.000000000000000000 ) ) ;
#32264 = ORIENTED_EDGE ( 'NONE', *, *, #32217, .F. ) ;
#32265 = DIRECTION ( 'NONE',  ( -3.996523416598930318E-16, 2.658563593772947863E-15, 1.000000000000000000 ) ) ;
#32266 = ORIENTED_EDGE ( 'NONE', *, *, #23962, .F. ) ;
#32267 = EDGE_CURVE ( 'NONE', #43001, #20513, #28944, .T. ) ;
#32268 = AXIS2_PLACEMENT_3D ( 'NONE', #24823, #11719, #34157 ) ;
#32269 = ORIENTED_EDGE ( 'NONE', *, *, #16677, .F. ) ;
#32270 = DIRECTION ( 'NONE',  ( 0.000000000000000000, 0.000000000000000000, 1.000000000000000000 ) ) ;
#32271 = ORIENTED_EDGE ( 'NONE', *, *, #26794, .T. ) ;
#32272 = DIRECTION ( 'NONE',  ( 0.000000000000000000, 0.000000000000000000, 1.000000000000000000 ) ) ;
#32273 = CARTESIAN_POINT ( 'NONE',  ( 17.99999999999999645, -35.72777019205596361, -106.3569410558020962 ) ) ;
#32274 = DIRECTION ( 'NONE',  ( -1.000000000000000000, 0.000000000000000000, -0.000000000000000000 ) ) ;
#32275 = DIRECTION ( 'NONE',  ( -1.000000000000000000, -0.000000000000000000, 0.000000000000000000 ) ) ;
#32276 = VERTEX_POINT ( 'NONE', #39272 ) ;
#32278 = DIRECTION ( 'NONE',  ( -1.000000000000000000, 0.000000000000000000, 0.000000000000000000 ) ) ;
#32277 =( GEOMETRIC_REPRESENTATION_CONTEXT ( 3 ) GLOBAL_UNCERTAINTY_ASSIGNED_CONTEXT ( ( #34368 ) ) GLOBAL_UNIT_ASSIGNED_CONTEXT ( ( #18724, #41567, #11717 ) ) REPRESENTATION_CONTEXT ( 'NONE', 'WORKASPACE' ) );
#32279 = VERTEX_POINT ( 'NONE', #19061 ) ;
#32280 = CIRCLE ( 'NONE', #26031, 59.00000000000000000 ) ;
#32281 = CARTESIAN_POINT ( 'NONE',  ( -10.00000000000000000, 0.000000000000000000, 0.000000000000000000 ) ) ;
#32282 = ORIENTED_EDGE ( 'NONE', *, *, #26748, .T. ) ;
#32283 = CARTESIAN_POINT ( 'NONE',  ( -15.99999999999997691, 31.00000000000000355, 5.571627607371296764E-15 ) ) ;
#32284 = EDGE_CURVE ( 'NONE', #19290, #39162, #34492, .T. ) ;
#32285 = DIRECTION ( 'NONE',  ( -1.000000000000000000, -0.000000000000000000, -0.000000000000000000 ) ) ;
#32286 =( NAMED_UNIT ( * ) SI_UNIT ( $, .STERADIAN. ) SOLID_ANGLE_UNIT ( ) );
#32287 = PLANE ( 'NONE',  #10019 ) ;
#32288 = CARTESIAN_POINT ( 'NONE',  ( 28.40420691229738281, 31.00000000000000355, 49.17333623205379922 ) ) ;
#32289 = ORIENTED_EDGE ( 'NONE', *, *, #33539, .T. ) ;
#32290 = DIRECTION ( 'NONE',  ( -1.000000000000000000, 0.000000000000000000, 0.000000000000000000 ) ) ;
#32291 = CIRCLE ( 'NONE', #38567, 13.59999999999999787 ) ;
#32292 = EDGE_LOOP ( 'NONE', ( #3738, #28054, #40328, #15257 ) ) ;
#32293 = ADVANCED_FACE ( 'NONE', ( #28858 ), #12497, .F. ) ;
#32294 = AXIS2_PLACEMENT_3D ( 'NONE', #31007, #39569, #24057 ) ;
#32295 = CARTESIAN_POINT ( 'NONE',  ( -16.10381281257427943, 40.00000000000000000, -60.09637020943575436 ) ) ;
#32296 = ADVANCED_FACE ( 'NONE', ( #25815 ), #39070, .T. ) ;
#32297 = CIRCLE ( 'NONE', #41345, 120.5010000000000190 ) ;
#32298 = FACE_OUTER_BOUND ( 'NONE', #39184, .T. ) ;
#32299 = EDGE_CURVE ( 'NONE', #35337, #959, #29623, .T. ) ;
#32300 = LINE ( 'NONE', #5481, #33255 ) ;
#32301 = EDGE_CURVE ( 'NONE', #24349, #5717, #15359, .T. ) ;
#32302 = DIRECTION ( 'NONE',  ( -1.000000000000000000, 0.000000000000000000, -0.000000000000000000 ) ) ;
#32303 = DIRECTION ( 'NONE',  ( 1.000000000000000000, 0.000000000000000000, 0.000000000000000000 ) ) ;
#32304 = PRESENTATION_LAYER_ASSIGNMENT (  '', '', ( #42040 ) ) ;
#32305 = EDGE_LOOP ( 'NONE', ( #16920, #12225, #4598, #27454 ) ) ;
#32306 = CARTESIAN_POINT ( 'NONE',  ( -20.88694679984194380, 40.00000000000000000, -36.15586224631631751 ) ) ;
#32307 = DIRECTION ( 'NONE',  ( 1.000000000000000000, 0.000000000000000000, 0.000000000000000000 ) ) ;
#32308 = CIRCLE ( 'NONE', #5151, 51.99999999999999289 ) ;
#32309 = DIRECTION ( 'NONE',  ( -1.000000000000000000, 1.373900992973642263E-15, 0.000000000000000000 ) ) ;
#32310 = ORIENTED_EDGE ( 'NONE', *, *, #23210, .F. ) ;
#32311 = CARTESIAN_POINT ( 'NONE',  ( 0.000000000000000000, -0.2227391519113303131, -46.98410307550732057 ) ) ;
#32312 = ORIENTED_EDGE ( 'NONE', *, *, #38400, .T. ) ;
#32313 = CARTESIAN_POINT ( 'NONE',  ( 2.000000000000000444, 3.464101615137754830, -3.142992957459231018 ) ) ;
#32314 = EDGE_LOOP ( 'NONE', ( #6482, #1781, #13392, #29809 ) ) ;
#32315 = CIRCLE ( 'NONE', #12131, 120.5010000000000474 ) ;
#32316 = EDGE_CURVE ( 'NONE', #16818, #7516, #26841, .T. ) ;
#32317 = VERTEX_POINT ( 'NONE', #5915 ) ;
#32318 =( REPRESENTATION_RELATIONSHIP ('NONE','NONE', #330, #7878 ) REPRESENTATION_RELATIONSHIP_WITH_TRANSFORMATION ( #24233 )SHAPE_REPRESENTATION_RELATIONSHIP( ) );
#32319 = CARTESIAN_POINT ( 'NONE',  ( 17.99999999999999645, 89.07460286905958924, -81.15544420874873310 ) ) ;
#32320 = CARTESIAN_POINT ( 'NONE',  ( 78.79907178683629354, 31.00000000000000000, 38.97904116289377185 ) ) ;
#32321 = ORIENTED_EDGE ( 'NONE', *, *, #12794, .T. ) ;
#32322 = DIRECTION ( 'NONE',  ( -1.000000000000000000, 1.084202172485505174E-16, 0.000000000000000000 ) ) ;
#32323 = CIRCLE ( 'NONE', #42053, 2.649999999999985700 ) ;
#32324 = DIRECTION ( 'NONE',  ( 0.000000000000000000, -0.7980172272802447120, 0.6026346363792492999 ) ) ;
#32325 = VERTEX_POINT ( 'NONE', #2630 ) ;
#32326 = CARTESIAN_POINT ( 'NONE',  ( 17.99999999999999645, 0.000000000000000000, 0.000000000000000000 ) ) ;
#32327 = AXIS2_PLACEMENT_3D ( 'NONE', #4791, #4552, #20982 ) ;
#32328 = CARTESIAN_POINT ( 'NONE',  ( 18.00000000000000355, -36.05989434073592292, -30.12041790338656710 ) ) ;
#32329 = CARTESIAN_POINT ( 'NONE',  ( -91.96080130434573618, -34.05525454449571043, 14.45886780445633946 ) ) ;
#32331 = CARTESIAN_POINT ( 'NONE',  ( 17.99999999999999645, 0.000000000000000000, 0.000000000000000000 ) ) ;
#32330 = DIRECTION ( 'NONE',  ( -1.000000000000000000, -0.000000000000000000, -0.000000000000000000 ) ) ;
#32332 = CARTESIAN_POINT ( 'NONE',  ( 1.472621547668719444, 31.00000000000000355, -22.60416666365413718 ) ) ;
#32333 = FACE_OUTER_BOUND ( 'NONE', #19056, .T. ) ;
#32334 = AXIS2_PLACEMENT_3D ( 'NONE', #41885, #37966, #1746 ) ;
#32335 = EDGE_CURVE ( 'NONE', #1632, #6408, #40736, .T. ) ;
#32336 = VERTEX_POINT ( 'NONE', #6139 ) ;
#32337 = VECTOR ( 'NONE', #1753, 1000.000000000000000 ) ;
#32338 = CARTESIAN_POINT ( 'NONE',  ( -26.76192867387533170, 31.00000000000000355, -15.44647709060871321 ) ) ;
#32339 = AXIS2_PLACEMENT_3D ( 'NONE', #28186, #41240, #15111 ) ;
#32340 = ORIENTED_EDGE ( 'NONE', *, *, #31561, .T. ) ;
#32341 = CARTESIAN_POINT ( 'NONE',  ( 0.000000000000000000, 51.98489025774451733, -108.7109110710156159 ) ) ;
#32342 = DIRECTION ( 'NONE',  ( 0.000000000000000000, 0.7980172272802408262, -0.6026346363792547400 ) ) ;
#32343 = ORIENTED_EDGE ( 'NONE', *, *, #27982, .T. ) ;
#32344 = CARTESIAN_POINT ( 'NONE',  ( 24.60508655230852781, 40.00000000000000000, 6.583411914924224284 ) ) ;
#32345 = CARTESIAN_POINT ( 'NONE',  ( -39.38196478160931946, 40.00000000000000000, 13.29643045357694753 ) ) ;
#32346 = EDGE_CURVE ( 'NONE', #19537, #15044, #24800, .T. ) ;
#32347 = CIRCLE ( 'NONE', #12166, 2.649999999999985700 ) ;
#32348 = EDGE_LOOP ( 'NONE', ( #21396, #31419, #32916, #34889 ) ) ;
#32349 = AXIS2_PLACEMENT_3D ( 'NONE', #23908, #27382, #37176 ) ;
#32350 = ORIENTED_EDGE ( 'NONE', *, *, #30974, .T. ) ;
#32351 = DIRECTION ( 'NONE',  ( -1.000000000000000000, -0.000000000000000000, -0.000000000000000000 ) ) ;
#32352 = CARTESIAN_POINT ( 'NONE',  ( -12.69999999999999929, 1.543054966925665076E-15, 12.59999999999999964 ) ) ;
#32353 = CARTESIAN_POINT ( 'NONE',  ( 17.99999999999999645, -84.09610293794118263, 74.27057253242982426 ) ) ;
#32354 = VECTOR ( 'NONE', #25108, 1000.000000000000000 ) ;
#32355 = EDGE_CURVE ( 'NONE', #28896, #14673, #22129, .T. ) ;
#32356 = CARTESIAN_POINT ( 'NONE',  ( 0.000000000000000000, -2.418575551220017328, -120.4767259403369053 ) ) ;
#32357 = CYLINDRICAL_SURFACE ( 'NONE', #2054, 59.00000000000000000 ) ;
#32358 = AXIS2_PLACEMENT_3D ( 'NONE', #29175, #12586, #22002 ) ;
#32359 = EDGE_LOOP ( 'NONE', ( #8551, #12426, #21154, #22907 ) ) ;
#32360 = DIRECTION ( 'NONE',  ( 0.000000000000000000, 0.000000000000000000, 1.000000000000000000 ) ) ;
#32361 = EDGE_LOOP ( 'NONE', ( #33854, #17855, #41639, #6194 ) ) ;
#32362 = DIRECTION ( 'NONE',  ( -1.000000000000000000, -0.000000000000000000, -0.000000000000000000 ) ) ;
#32363 = CYLINDRICAL_SURFACE ( 'NONE', #10276, 22.99999999999987921 ) ;
#32364 = CARTESIAN_POINT ( 'NONE',  ( -10.00000000000000178, 0.000000000000000000, 0.000000000000000000 ) ) ;
#32365 = DIRECTION ( 'NONE',  ( 1.000000000000000000, 0.000000000000000000, 0.000000000000000000 ) ) ;
#32366 = ORIENTED_EDGE ( 'NONE', *, *, #21450, .T. ) ;
#32367 = CARTESIAN_POINT ( 'NONE',  ( -23.88228986782336349, 40.00000000000000000, -89.13686966975919290 ) ) ;
#32368 = ORIENTED_EDGE ( 'NONE', *, *, #8602, .F. ) ;
#32369 = FACE_OUTER_BOUND ( 'NONE', #6457, .T. ) ;
#32370 = AXIS2_PLACEMENT_3D ( 'NONE', #33466, #20413, #31502 ) ;
#32371 = ADVANCED_FACE ( 'NONE', ( #21913 ), #18860, .T. ) ;
#32372 = ORIENTED_EDGE ( 'NONE', *, *, #17193, .T. ) ;
#32374 = ORIENTED_EDGE ( 'NONE', *, *, #31338, .F. ) ;
#32373 = DIRECTION ( 'NONE',  ( 0.000000000000000000, -0.5264321628773450668, -0.8502171357296208765 ) ) ;
#32375 = CARTESIAN_POINT ( 'NONE',  ( 33.95200755730775199, 31.00000000000000355, -44.10258293179329314 ) ) ;
#32377 = EDGE_CURVE ( 'NONE', #21133, #13162, #17070, .T. ) ;
#32376 = VERTEX_POINT ( 'NONE', #5506 ) ;
#32378 = CARTESIAN_POINT ( 'NONE',  ( 18.00000000000000355, 0.000000000000000000, 0.000000000000000000 ) ) ;
#32379 = AXIS2_PLACEMENT_3D ( 'NONE', #33069, #25717, #22882 ) ;
#32380 = DIRECTION ( 'NONE',  ( 1.000000000000000000, -1.373900992973641868E-15, -6.546126324440886161E-16 ) ) ;
#32381 = CIRCLE ( 'NONE', #10810, 120.5010000000000332 ) ;
#32382 = ORIENTED_EDGE ( 'NONE', *, *, #21032, .F. ) ;
#32383 = CARTESIAN_POINT ( 'NONE',  ( 69.81317433577432041, 39.99999999999999289, 34.54326205988235188 ) ) ;
#32384 = AXIS2_PLACEMENT_3D ( 'NONE', #9017, #26465, #27275 ) ;
#32386 = DIRECTION ( 'NONE',  ( -3.996523416598930318E-16, 2.658563593772947863E-15, 1.000000000000000000 ) ) ;
#32385 = DIRECTION ( 'NONE',  ( -1.000000000000000000, 0.000000000000000000, 0.000000000000000000 ) ) ;
#32387 = AXIS2_PLACEMENT_3D ( 'NONE', #8216, #1216, #7983 ) ;
#32388 = CARTESIAN_POINT ( 'NONE',  ( 9.000000000000000000, -35.78425302087541127, 3.935382540232670312 ) ) ;
#32389 = ORIENTED_EDGE ( 'NONE', *, *, #40138, .F. ) ;
#32390 = DIRECTION ( 'NONE',  ( 1.000000000000000000, 0.000000000000000000, -3.273063162220416457E-16 ) ) ;
#32391 = ADVANCED_FACE ( 'NONE', ( #19914, #16863 ), #10050, .T. ) ;
#32392 = EDGE_LOOP ( 'NONE', ( #11876, #4428 ) ) ;
#32393 = CIRCLE ( 'NONE', #7307, 120.5010000000000190 ) ;
#32394 = DIRECTION ( 'NONE',  ( 0.000000000000000000, -0.05322217484218558226, 0.9985826956767615004 ) ) ;
#32395 = CARTESIAN_POINT ( 'NONE',  ( 9.000000000000001776, -5.871425383721168956, -51.66745943012288222 ) ) ;
#32396 = CARTESIAN_POINT ( 'NONE',  ( -31.81163009274181519, 31.00000000000000355, -64.50738158386226928 ) ) ;
#32398 = DIRECTION ( 'NONE',  ( -1.000000000000000000, -0.000000000000000000, 0.000000000000000000 ) ) ;
#32397 = CYLINDRICAL_SURFACE ( 'NONE', #31634, 20.00000000000001066 ) ;
#32399 = ORIENTED_EDGE ( 'NONE', *, *, #10949, .T. ) ;
#32400 = AXIS2_PLACEMENT_3D ( 'NONE', #31711, #25406, #38664 ) ;
#32401 = LINE ( 'NONE', #25684, #40020 ) ;
#32402 = EDGE_CURVE ( 'NONE', #41964, #19993, #32963, .T. ) ;
#32403 = ORIENTED_EDGE ( 'NONE', *, *, #9886, .F. ) ;
#32404 = CARTESIAN_POINT ( 'NONE',  ( 0.000000000000000000, 0.000000000000000000, 0.000000000000000000 ) ) ;
#32405 = EDGE_CURVE ( 'NONE', #17146, #9453, #15070, .T. ) ;
#32406 = CARTESIAN_POINT ( 'NONE',  ( 0.000000000000000000, -5.871425383721900815, 51.66745943012280406 ) ) ;
#32407 = CARTESIAN_POINT ( 'NONE',  ( 12.87762912550514827, 31.00000000000000355, 98.66289914823325091 ) ) ;
#32408 = CARTESIAN_POINT ( 'NONE',  ( 94.26586287999622016, 39.99999999999999289, 25.37251369638877563 ) ) ;
#32409 = AXIS2_PLACEMENT_3D ( 'NONE', #19694, #3484, #26008 ) ;
#32410 = CARTESIAN_POINT ( 'NONE',  ( 17.99999999999999645, 17.77780072541695944, 114.6296200873376563 ) ) ;
#32411 = AXIS2_PLACEMENT_3D ( 'NONE', #21704, #31691, #41492 ) ;
#32412 = VERTEX_POINT ( 'NONE', #42988 ) ;
#32413 = CYLINDRICAL_SURFACE ( 'NONE', #4695, 116.0000000000000000 ) ;
#32414 = ORIENTED_EDGE ( 'NONE', *, *, #42652, .T. ) ;
#32415 = DIRECTION ( 'NONE',  ( -1.000000000000000000, 0.000000000000000000, 0.000000000000000000 ) ) ;
#32416 = VECTOR ( 'NONE', #23120, 1000.000000000000000 ) ;
#32417 = CIRCLE ( 'NONE', #2464, 59.00000000000000711 ) ;
#32418 = CARTESIAN_POINT ( 'NONE',  ( 17.99999999999999645, 35.78484819117785776, -110.3423972910429143 ) ) ;
#32419 = CARTESIAN_POINT ( 'NONE',  ( 17.99999999999999645, 0.000000000000000000, 0.000000000000000000 ) ) ;
#32420 = VERTEX_POINT ( 'NONE', #432 ) ;
#32421 = LINE ( 'NONE', #5386, #42566 ) ;
#32422 = CYLINDRICAL_SURFACE ( 'NONE', #8843, 59.00000000000000000 ) ;
#32423 = AXIS2_PLACEMENT_3D ( 'NONE', #7736, #21097, #21315 ) ;
#32424 = DIRECTION ( 'NONE',  ( 0.000000000000000000, -0.7705132427757949154, 0.6374239897486827511 ) ) ;
#32425 = ORIENTED_EDGE ( 'NONE', *, *, #23368, .F. ) ;
#32426 = EDGE_CURVE ( 'NONE', #10195, #15282, #12928, .T. ) ;
#32427 = CARTESIAN_POINT ( 'NONE',  ( -17.43724119492662794, 31.00000000000000355, -15.29674861594511448 ) ) ;
#32428 = ADVANCED_FACE ( 'NONE', ( #23397 ), #6349, .F. ) ;
#32429 = DIRECTION ( 'NONE',  ( 0.000000000000000000, 0.000000000000000000, 1.000000000000000000 ) ) ;
#32430 = EDGE_CURVE ( 'NONE', #6784, #9051, #38006, .T. ) ;
#32431 = EDGE_CURVE ( 'NONE', #42007, #15552, #10494, .T. ) ;
#32433 = ORIENTED_EDGE ( 'NONE', *, *, #16677, .T. ) ;
#32432 = DIRECTION ( 'NONE',  ( -1.000000000000000000, -0.000000000000000000, 0.000000000000000000 ) ) ;
#32434 = ORIENTED_EDGE ( 'NONE', *, *, #39892, .T. ) ;
#32435 = CARTESIAN_POINT ( 'NONE',  ( 9.000000000000001776, 41.60679253225906393, -108.2814610871942165 ) ) ;
#32436 = CARTESIAN_POINT ( 'NONE',  ( 8.999999999999998224, 35.89808275599445153, 2.706964063997355119 ) ) ;
#32437 = CARTESIAN_POINT ( 'NONE',  ( -41.52979953745317232, 40.00000000000000000, 5.398177843167591305 ) ) ;
#32438 = CARTESIAN_POINT ( 'NONE',  ( 0.000000000000000000, -110.3490479609630910, -20.28201389785511211 ) ) ;
#32439 = AXIS2_PLACEMENT_3D ( 'NONE', #27634, #4466, #11058 ) ;
#32440 = CARTESIAN_POINT ( 'NONE',  ( -0.3461262719736137305, 4.658553426539289610, -3.671615880910373608 ) ) ;
#32441 = CIRCLE ( 'NONE', #26876, 120.5010000000000190 ) ;
#32442 = CARTESIAN_POINT ( 'NONE',  ( 17.99999999999999645, 34.03109950475727175, 115.5957406979051285 ) ) ;
#32443 = VERTEX_POINT ( 'NONE', #36658 ) ;
#32444 = DIRECTION ( 'NONE',  ( 0.000000000000000000, -0.3612416661871601375, 0.9324722294043530368 ) ) ;
#32445 = ORIENTED_EDGE ( 'NONE', *, *, #30864, .T. ) ;
#32446 = PRESENTATION_LAYER_ASSIGNMENT (  '', '', ( #9421 ) ) ;
#32447 = DIRECTION ( 'NONE',  ( 1.000000000000000000, 0.000000000000000000, 0.000000000000000000 ) ) ;
#32448 = DIRECTION ( 'NONE',  ( 1.000000000000000000, 0.000000000000000000, 0.000000000000000000 ) ) ;
#32449 = CARTESIAN_POINT ( 'NONE',  ( -4.929261580875707871, 31.00000000000000355, 37.46659216873931797 ) ) ;
#32450 = DIRECTION ( 'NONE',  ( 1.000000000000000000, 0.000000000000000000, 0.000000000000000000 ) ) ;
#32452 = EDGE_LOOP ( 'NONE', ( #1969, #37094, #4556, #9659 ) ) ;
#32451 = AXIS2_PLACEMENT_3D ( 'NONE', #21735, #34988, #18456 ) ;
#32453 = AXIS2_PLACEMENT_3D ( 'NONE', #33772, #5122, #11262 ) ;
#32455 = AXIS2_PLACEMENT_3D ( 'NONE', #21046, #17765, #3961 ) ;
#32454 = CARTESIAN_POINT ( 'NONE',  ( 17.99999999999999645, -117.9424311864587480, -24.69967462999156638 ) ) ;
#32456 = ADVANCED_FACE ( 'NONE', ( #2833 ), #33185, .F. ) ;
#32457 = CARTESIAN_POINT ( 'NONE',  ( 77.05880969081472642, 31.00000000000000000, 37.98468489477117771 ) ) ;
#32458 = EDGE_CURVE ( 'NONE', #29185, #18549, #30364, .T. ) ;
#32459 = CARTESIAN_POINT ( 'NONE',  ( 8.999999999999998224, -74.56001736500559218, -88.86396238369110279 ) ) ;
#32460 = ORIENTED_EDGE ( 'NONE', *, *, #10461, .F. ) ;
#32461 = CARTESIAN_POINT ( 'NONE',  ( -53.12901929300349479, 31.00000000000000355, 30.56653509229933618 ) ) ;
#32462 = CARTESIAN_POINT ( 'NONE',  ( -43.11175393642376719, 40.00000000000000000, 56.02072642018850246 ) ) ;
#32463 = CARTESIAN_POINT ( 'NONE',  ( -6.381360069252544953, 40.00000000000000000, 97.60416666604666602 ) ) ;
#32464 = VERTEX_POINT ( 'NONE', #16200 ) ;
#32465 = CARTESIAN_POINT ( 'NONE',  ( 0.1410422978106145031, -4.700232962125109104, -3.687027686973628704 ) ) ;
#32466 = DIRECTION ( 'NONE',  ( -1.000000000000000000, -0.000000000000000000, -0.000000000000000000 ) ) ;
#32467 = CYLINDRICAL_SURFACE ( 'NONE', #3787, 13.60000000000000142 ) ;
#32468 = VECTOR ( 'NONE', #23682, 1000.000000000000000 ) ;
#32470 = ORIENTED_EDGE ( 'NONE', *, *, #16704, .T. ) ;
#32469 = DIRECTION ( 'NONE',  ( 0.000000000000000000, 0.1062934856473655293, -0.9943348002101370930 ) ) ;
#32471 = VECTOR ( 'NONE', #27254, 1000.000000000000000 ) ;
#32472 = DIRECTION ( 'NONE',  ( 1.000000000000000000, 0.000000000000000000, 0.000000000000000000 ) ) ;
#32473 = VECTOR ( 'NONE', #30304, 1000.000000000000000 ) ;
#32474 = DIRECTION ( 'NONE',  ( -1.000000000000000000, -0.000000000000000000, 0.000000000000000000 ) ) ;
#32475 = ORIENTED_EDGE ( 'NONE', *, *, #32623, .F. ) ;
#32476 = CARTESIAN_POINT ( 'NONE',  ( -70.10416666575086708, 40.00000000000000711, -4.581489278090966621 ) ) ;
#32477 = CARTESIAN_POINT ( 'NONE',  ( 17.99999999999999645, -104.2166695095716591, 60.49278301857773243 ) ) ;
#32478 = EDGE_LOOP ( 'NONE', ( #31970, #2510, #21119, #32003 ) ) ;
#32479 = AXIS2_PLACEMENT_3D ( 'NONE', #25458, #8618, #11720 ) ;
#32480 = EDGE_CURVE ( 'NONE', #39282, #5822, #23623, .T. ) ;
#32481 = DIRECTION ( 'NONE',  ( -1.000000000000000000, -0.000000000000000000, 0.000000000000000000 ) ) ;
#32482 = EDGE_CURVE ( 'NONE', #12118, #24229, #25507, .T. ) ;
#32483 = EDGE_CURVE ( 'NONE', #10144, #5055, #6783, .T. ) ;
#32484 = CIRCLE ( 'NONE', #26919, 13.59999999999999964 ) ;
#32485 = ORIENTED_EDGE ( 'NONE', *, *, #14881, .T. ) ;
#32486 = EDGE_CURVE ( 'NONE', #27767, #17459, #42168, .T. ) ;
#32487 = AXIS2_PLACEMENT_3D ( 'NONE', #24042, #24272, #4350 ) ;
#32488 = ORIENTED_EDGE ( 'NONE', *, *, #40509, .T. ) ;
#32489 = DIRECTION ( 'NONE',  ( -1.000000000000000000, 0.000000000000000000, -0.000000000000000000 ) ) ;
#32490 = ORIENTED_EDGE ( 'NONE', *, *, #21622, .T. ) ;
#32491 = CARTESIAN_POINT ( 'NONE',  ( 18.00000000000001421, 0.000000000000000000, 0.000000000000000000 ) ) ;
#32492 = CARTESIAN_POINT ( 'NONE',  ( 17.99999999999999645, -92.25992191227339845, -77.51514567967485902 ) ) ;
#32493 = CARTESIAN_POINT ( 'NONE',  ( 0.000000000000000000, -46.77034588191318676, 22.72740077717213936 ) ) ;
#32494 = CARTESIAN_POINT ( 'NONE',  ( 17.99999999999999645, 0.000000000000000000, 0.000000000000000000 ) ) ;
#32495 = ORIENTED_EDGE ( 'NONE', *, *, #3344, .T. ) ;
#32496 = CARTESIAN_POINT ( 'NONE',  ( -2.649999999999993694, -150.5000000000000284, 6.999999999999998224 ) ) ;
#32497 = PRODUCT_DEFINITION_CONTEXT ( 'detailed design', #27897, 'design' ) ;
#32498 = ORIENTED_EDGE ( 'NONE', *, *, #36160, .T. ) ;
#32499 = DIRECTION ( 'NONE',  ( 0.000000000000000000, 0.000000000000000000, -1.000000000000000000 ) ) ;
#32501 = VERTEX_POINT ( 'NONE', #36434 ) ;
#32500 = AXIS2_PLACEMENT_3D ( 'NONE', #12293, #33571, #30313 ) ;
#32502 = FACE_OUTER_BOUND ( 'NONE', #17192, .T. ) ;
#32503 = AXIS2_PLACEMENT_3D ( 'NONE', #30535, #37052, #40525 ) ;
#32504 = CARTESIAN_POINT ( 'NONE',  ( 17.99999999999999645, 0.000000000000000000, 0.000000000000000000 ) ) ;
#32505 = AXIS2_PLACEMENT_3D ( 'NONE', #21168, #34418, #21395 ) ;
#32506 = DIRECTION ( 'NONE',  ( -1.000000000000000000, 3.009274222672345096E-17, 0.000000000000000000 ) ) ;
#32507 = CARTESIAN_POINT ( 'NONE',  ( -16.10381281257427943, 31.00000000000000355, -60.09637020943575436 ) ) ;
#32508 = CIRCLE ( 'NONE', #42926, 120.5010000000000190 ) ;
#32509 = DIRECTION ( 'NONE',  ( 1.000000000000000000, 0.000000000000000000, 0.000000000000000000 ) ) ;
#32510 = ORIENTED_EDGE ( 'NONE', *, *, #21743, .T. ) ;
#32512 = CARTESIAN_POINT ( 'NONE',  ( 35.58384423644163519, 31.00000000000000355, 12.14845634898874138 ) ) ;
#32511 = CIRCLE ( 'NONE', #25579, 116.0000000000000000 ) ;
#32513 = ADVANCED_FACE ( 'NONE', ( #33610 ), #26223, .T. ) ;
#32514 = CARTESIAN_POINT ( 'NONE',  ( 21.58803501788969115, 40.00000000000000000, 63.55567069162312777 ) ) ;
#32515 = AXIS2_PLACEMENT_3D ( 'NONE', #28920, #9047, #36288 ) ;
#32516 = LINE ( 'NONE', #42529, #33226 ) ;
#32517 = CARTESIAN_POINT ( 'NONE',  ( 9.000000000000001776, -25.61928775981074935, 45.25098998563468200 ) ) ;
#32518 = DIRECTION ( 'NONE',  ( -1.000000000000000000, -0.000000000000000000, -0.000000000000000000 ) ) ;
#32519 = DIRECTION ( 'NONE',  ( 0.000000000000000000, 0.4817536741017162671, -0.8763066800438630288 ) ) ;
#32520 = PRODUCT_DEFINITION_SHAPE ( 'NONE', 'NONE',  #43194 ) ;
#32521 = ORIENTED_EDGE ( 'NONE', *, *, #2383, .F. ) ;
#32522 = CARTESIAN_POINT ( 'NONE',  ( -39.12533628356670334, 40.00000000000000000, -10.47265044290268499 ) ) ;
#32523 = CYLINDRICAL_SURFACE ( 'NONE', #35483, 58.99999999999998579 ) ;
#32524 = CARTESIAN_POINT ( 'NONE',  ( 9.000000000000001776, 111.2559044912529345, -32.83479428644565701 ) ) ;
#32525 = EDGE_LOOP ( 'NONE', ( #7932, #9745 ) ) ;
#32526 = AXIS2_PLACEMENT_3D ( 'NONE', #31148, #38522, #8642 ) ;
#32527 = CARTESIAN_POINT ( 'NONE',  ( 0.000000000000000000, 0.000000000000000000, 0.000000000000000000 ) ) ;
#32528 = CARTESIAN_POINT ( 'NONE',  ( 0.000000000000000000, -116.0452958106478434, -32.46506308663576590 ) ) ;
#32529 = EDGE_CURVE ( 'NONE', #36025, #24485, #2453, .T. ) ;
#32530 = ORIENTED_EDGE ( 'NONE', *, *, #17271, .T. ) ;
#32531 = CARTESIAN_POINT ( 'NONE',  ( -106.4195705685748550, -106.4195705685759776, 10.00000000000000000 ) ) ;
#32532 = ORIENTED_EDGE ( 'NONE', *, *, #27297, .F. ) ;
#32533 = AXIS2_PLACEMENT_3D ( 'NONE', #11886, #25637, #38460 ) ;
#32534 = ADVANCED_FACE ( 'NONE', ( #29714 ), #13145, .T. ) ;
#32535 = ORIENTED_EDGE ( 'NONE', *, *, #15661, .T. ) ;
#32536 = CARTESIAN_POINT ( 'NONE',  ( 17.99999999999999645, -115.0622509503833442, 14.72000021165104755 ) ) ;
#32537 = CIRCLE ( 'NONE', #14441, 36.00000000000000000 ) ;
#32538 = CARTESIAN_POINT ( 'NONE',  ( -53.37462671637112521, 31.00000000000000711, 60.68184199296217685 ) ) ;
#32539 = EDGE_LOOP ( 'NONE', ( #32264, #15372, #40155, #28330 ) ) ;
#32540 = DIRECTION ( 'NONE',  ( 0.000000000000000000, 0.000000000000000000, 1.000000000000000000 ) ) ;
#32541 = DIRECTION ( 'NONE',  ( -0.000000000000000000, -0.000000000000000000, 1.000000000000000000 ) ) ;
#32542 = CARTESIAN_POINT ( 'NONE',  ( -10.00000000000000000, 0.000000000000000000, 0.000000000000000000 ) ) ;
#32543 = ORIENTED_EDGE ( 'NONE', *, *, #6549, .T. ) ;
#32544 = EDGE_CURVE ( 'NONE', #33622, #8604, #5958, .T. ) ;
#32545 = CARTESIAN_POINT ( 'NONE',  ( 8.919999999999994600, 0.000000000000000000, 14.99999999999999822 ) ) ;
#32546 = AXIS2_PLACEMENT_3D ( 'NONE', #18485, #28291, #3647 ) ;
#32547 = CARTESIAN_POINT ( 'NONE',  ( 49.34100556531813453, 40.00000000000000000, 85.68208892729249726 ) ) ;
#32548 = AXIS2_PLACEMENT_3D ( 'NONE', #14930, #38239, #17784 ) ;
#32549 = DIRECTION ( 'NONE',  ( 0.000000000000000000, -0.3612416661871603596, 0.9324722294043529258 ) ) ;
#32550 = ADVANCED_FACE ( 'NONE', ( #10706 ), #31438, .F. ) ;
#32552 = LINE ( 'NONE', #9412, #3203 ) ;
#32551 = CARTESIAN_POINT ( 'NONE',  ( -6.600000000000001421, 3.469446951953649688E-15, 0.000000000000000000 ) ) ;
#32553 = DIRECTION ( 'NONE',  ( -1.000000000000000000, -0.000000000000000000, 0.000000000000000000 ) ) ;
#32554 = VERTEX_POINT ( 'NONE', #3918 ) ;
#32555 = CARTESIAN_POINT ( 'NONE',  ( -3.620280825866593055, 31.00000000000000355, 27.53105304817175636 ) ) ;
#32556 = VERTEX_POINT ( 'NONE', #27964 ) ;
#32557 = DIRECTION ( 'NONE',  ( 0.000000000000000000, 0.000000000000000000, 1.000000000000000000 ) ) ;
#32558 = DIRECTION ( 'NONE',  ( -1.000000000000000000, -0.000000000000000000, 0.000000000000000000 ) ) ;
#32559 = CIRCLE ( 'NONE', #10969, 2.649999999999971934 ) ;
#32560 = ORIENTED_EDGE ( 'NONE', *, *, #25870, .T. ) ;
#32561 = CARTESIAN_POINT ( 'NONE',  ( 11.92156526682413720, 40.00000000000000000, 35.08788755311113761 ) ) ;
#32562 = CIRCLE ( 'NONE', #38817, 36.00000000000000000 ) ;
#32563 = CARTESIAN_POINT ( 'NONE',  ( -29.39530816626169596, 40.00000000000000000, -14.54745122861429252 ) ) ;
#32564 = AXIS2_PLACEMENT_3D ( 'NONE', #17344, #32112, #41912 ) ;
#32565 = VECTOR ( 'NONE', #36891, 1000.000000000000000 ) ;
#32566 = CIRCLE ( 'NONE', #20787, 116.0000000000000000 ) ;
#32567 = EDGE_LOOP ( 'NONE', ( #1363, #6187, #9908, #14495 ) ) ;
#32568 = VECTOR ( 'NONE', #28273, 1000.000000000000000 ) ;
#32569 = ORIENTED_EDGE ( 'NONE', *, *, #36697, .F. ) ;
#32570 =( NAMED_UNIT ( * ) SI_UNIT ( $, .STERADIAN. ) SOLID_ANGLE_UNIT ( ) );
#32571 = CARTESIAN_POINT ( 'NONE',  ( 17.99999999999999645, 31.81777574834305966, -2.898764365605425830 ) ) ;
#32572 = SURFACE_STYLE_USAGE ( .BOTH. , #19298 ) ;
#32573 = AXIS2_PLACEMENT_3D ( 'NONE', #34505, #17991, #8332 ) ;
#32574 = LINE ( 'NONE', #2656, #19190 ) ;
#32575 = DIRECTION ( 'NONE',  ( 1.000000000000000000, -0.000000000000000000, -0.000000000000000000 ) ) ;
#32576 = CARTESIAN_POINT ( 'NONE',  ( -99.67789407897798526, 31.00000000000000000, -5.066036069491916649 ) ) ;
#32577 = EDGE_LOOP ( 'NONE', ( #25890, #40649 ) ) ;
#32578 = DIRECTION ( 'NONE',  ( 0.000000000000000000, 0.000000000000000000, 1.000000000000000000 ) ) ;
#32579 = VERTEX_POINT ( 'NONE', #1312 ) ;
#32580 = DIRECTION ( 'NONE',  ( -1.000000000000000000, -0.000000000000000000, 0.000000000000000000 ) ) ;
#32581 = LINE ( 'NONE', #28899, #31192 ) ;
#32582 = CYLINDRICAL_SURFACE ( 'NONE', #31891, 59.00000000000000000 ) ;
#32583 = EDGE_CURVE ( 'NONE', #6410, #13842, #18545, .T. ) ;
#32584 = FACE_OUTER_BOUND ( 'NONE', #7144, .T. ) ;
#32585 = VERTEX_POINT ( 'NONE', #7859 ) ;
#32586 = LINE ( 'NONE', #3523, #29171 ) ;
#32587 = ORIENTED_EDGE ( 'NONE', *, *, #1784, .F. ) ;
#32588 = ADVANCED_FACE ( 'NONE', ( #41439 ), #40571, .F. ) ;
#32589 = DIRECTION ( 'NONE',  ( -1.000000000000000000, 0.000000000000000000, -0.000000000000000000 ) ) ;
#32590 = VERTEX_POINT ( 'NONE', #20561 ) ;
#32592 = EDGE_LOOP ( 'NONE', ( #19868, #7001, #16848, #26026 ) ) ;
#32591 = LINE ( 'NONE', #25437, #644 ) ;
#32593 = CARTESIAN_POINT ( 'NONE',  ( -13.02511903071888355, 31.00000000000000355, 48.29538318457647961 ) ) ;
#32594 = EDGE_LOOP ( 'NONE', ( #42822, #35956 ) ) ;
#32595 = CARTESIAN_POINT ( 'NONE',  ( 17.99999999999999645, 5.456439917446431309, -112.0647122740741253 ) ) ;
#32596 = CIRCLE ( 'NONE', #27730, 13.40000000000000036 ) ;
#32597 = ORIENTED_EDGE ( 'NONE', *, *, #26843, .F. ) ;
#32598 = EDGE_CURVE ( 'NONE', #20215, #36754, #27517, .T. ) ;
#32599 = VECTOR ( 'NONE', #42544, 1000.000000000000000 ) ;
#32600 = CARTESIAN_POINT ( 'NONE',  ( 17.99999999999999645, -35.54274411427983438, -115.1399337407609949 ) ) ;
#32601 = ORIENTED_EDGE ( 'NONE', *, *, #41954, .T. ) ;
#32602 = CARTESIAN_POINT ( 'NONE',  ( -64.10496366469683949, 40.00000000000000711, 31.48763712508877077 ) ) ;
#32603 = CIRCLE ( 'NONE', #11013, 58.99999999999999289 ) ;
#32604 = EDGE_CURVE ( 'NONE', #40591, #9049, #31741, .T. ) ;
#32605 = AXIS2_PLACEMENT_3D ( 'NONE', #27074, #3251, #6533 ) ;
#32607 = CARTESIAN_POINT ( 'NONE',  ( 17.99999999999999645, 59.07817985939002625, 105.0250430397510968 ) ) ;
#32606 = DIRECTION ( 'NONE',  ( -1.000000000000000000, -0.000000000000000000, 0.000000000000000000 ) ) ;
#32608 = DIRECTION ( 'NONE',  ( -0.000000000000000000, -0.000000000000000000, 1.000000000000000000 ) ) ;
#32609 = VERTEX_POINT ( 'NONE', #27750 ) ;
#32610 = LINE ( 'NONE', #42829, #41857 ) ;
#32611 = ORIENTED_EDGE ( 'NONE', *, *, #31108, .T. ) ;
#32612 = DIRECTION ( 'NONE',  ( -1.000000000000000000, -0.000000000000000000, 0.000000000000000000 ) ) ;
#32613 = DIRECTION ( 'NONE',  ( -1.000000000000000000, 0.000000000000000000, -0.000000000000000000 ) ) ;
#32614 = CARTESIAN_POINT ( 'NONE',  ( -25.13323546007955045, 31.00000000000000355, 74.03861446737784036 ) ) ;
#32616 = CYLINDRICAL_SURFACE ( 'NONE', #42258, 10.49999999999999112 ) ;
#32615 = CYLINDRICAL_SURFACE ( 'NONE', #25374, 59.00000000000000000 ) ;
#32617 = CIRCLE ( 'NONE', #8853, 59.00000000000001421 ) ;
#32618 = ORIENTED_EDGE ( 'NONE', *, *, #20755, .T. ) ;
#32619 = DIRECTION ( 'NONE',  ( 1.000000000000000000, 0.000000000000000000, 0.000000000000000000 ) ) ;
#32620 = ADVANCED_FACE ( 'NONE', ( #37741 ), #8079, .F. ) ;
#32621 = ORIENTED_EDGE ( 'NONE', *, *, #23810, .T. ) ;
#32622 = LINE ( 'NONE', #2702, #14370 ) ;
#32623 = EDGE_CURVE ( 'NONE', #4717, #22785, #37289, .T. ) ;
#32624 = CARTESIAN_POINT ( 'NONE',  ( -10.00000000000000000, 0.000000000000000000, 0.000000000000000000 ) ) ;
#32625 = CIRCLE ( 'NONE', #7518, 20.00000000000000711 ) ;
#32626 = CARTESIAN_POINT ( 'NONE',  ( -92.09225407318749035, 31.00000000000000711, -6.144973693751363264 ) ) ;
#32627 = CIRCLE ( 'NONE', #29161, 58.99999999999999289 ) ;
#32628 = CARTESIAN_POINT ( 'NONE',  ( -13.16936484334534008, 40.00000000000000000, 99.04657264458933241 ) ) ;
#32629 = DIRECTION ( 'NONE',  ( 1.000000000000000000, 0.000000000000000000, 0.000000000000000000 ) ) ;
#32630 = AXIS2_PLACEMENT_3D ( 'NONE', #36808, #36154, #39637 ) ;
#32631 = EDGE_LOOP ( 'NONE', ( #3745, #35846 ) ) ;
#32632 = LINE ( 'NONE', #36313, #30538 ) ;
#32633 = CIRCLE ( 'NONE', #13856, 20.00000000000000711 ) ;
#32634 = ORIENTED_EDGE ( 'NONE', *, *, #42652, .F. ) ;
#32635 = AXIS2_PLACEMENT_3D ( 'NONE', #9667, #19728, #39307 ) ;
#32636 = CARTESIAN_POINT ( 'NONE',  ( 0.000000000000000000, -5.456439917444183330, -112.0647122740742390 ) ) ;
#32637 = DIRECTION ( 'NONE',  ( -1.000000000000000000, 0.000000000000000000, 0.000000000000000000 ) ) ;
#32638 = PLANE ( 'NONE',  #14257 ) ;
#32639 = VERTEX_POINT ( 'NONE', #21446 ) ;
#32640 = CARTESIAN_POINT ( 'NONE',  ( 0.000000000000000000, -107.5680526044917542, -31.89649718262205269 ) ) ;
#32641 = ADVANCED_FACE ( 'NONE', ( #4577 ), #17952, .F. ) ;
#32642 = CARTESIAN_POINT ( 'NONE',  ( 9.000000000000001776, -107.1354928292872728, 44.47455650398029547 ) ) ;
#32643 = DIRECTION ( 'NONE',  ( 1.000000000000000000, 0.000000000000000000, 0.000000000000000000 ) ) ;
#32645 = VERTEX_POINT ( 'NONE', #18172 ) ;
#32644 = CARTESIAN_POINT ( 'NONE',  ( -10.00000000000000000, 0.000000000000000000, 0.000000000000000000 ) ) ;
#32646 = CARTESIAN_POINT ( 'NONE',  ( -22.06642698273766356, 31.00000000000000355, -2.901557744773885616 ) ) ;
#32647 = CARTESIAN_POINT ( 'NONE',  ( 8.999999999999998224, 83.58328028049660929, 80.43528614701352808 ) ) ;
#32648 = ADVANCED_FACE ( 'NONE', ( #4142 ), #1758, .T. ) ;
#32650 = ORIENTED_EDGE ( 'NONE', *, *, #12261, .T. ) ;
#32649 = DIRECTION ( 'NONE',  ( 0.000000000000000000, 1.000000000000000000, 0.000000000000000000 ) ) ;
#32651 = UNCERTAINTY_MEASURE_WITH_UNIT (LENGTH_MEASURE( 1.000000000000000082E-05 ), #3756, 'distance_accuracy_value', 'NONE');
#32652 = VERTEX_POINT ( 'NONE', #14870 ) ;
#32653 = DIRECTION ( 'NONE',  ( -1.000000000000000000, 0.000000000000000000, 0.000000000000000000 ) ) ;
#32654 = CARTESIAN_POINT ( 'NONE',  ( 4.121423858225410797, -12.61643262889541006, -1.199999999999999956 ) ) ;
#32655 = CARTESIAN_POINT ( 'NONE',  ( 31.88898475262399401, 40.00000000000000000, 36.48290236124523744 ) ) ;
#32656 = CARTESIAN_POINT ( 'NONE',  ( 17.99999999999999645, 0.000000000000000000, 0.000000000000000000 ) ) ;
#32657 = EDGE_CURVE ( 'NONE', #26052, #32990, #24277, .T. ) ;
#32658 = CIRCLE ( 'NONE', #8279, 20.00000000000000711 ) ;
#32659 = CARTESIAN_POINT ( 'NONE',  ( 9.000000000000001776, 44.25018368420742831, 27.31155879685195842 ) ) ;
#32660 = DIRECTION ( 'NONE',  ( 0.000000000000000000, 0.000000000000000000, 1.000000000000000000 ) ) ;
#32661 = EDGE_LOOP ( 'NONE', ( #10537, #4816, #30011, #38680 ) ) ;
#32662 = AXIS2_PLACEMENT_3D ( 'NONE', #5326, #9022, #39107 ) ;
#32663 = DIRECTION ( 'NONE',  ( -1.000000000000000000, -0.000000000000000000, 0.000000000000000000 ) ) ;
#32664 = ORIENTED_EDGE ( 'NONE', *, *, #2722, .F. ) ;
#32665 = DIRECTION ( 'NONE',  ( -1.000000000000000000, 0.000000000000000000, 0.000000000000000000 ) ) ;
#32666 = DIRECTION ( 'NONE',  ( 0.000000000000000000, 0.000000000000000000, -1.000000000000000000 ) ) ;
#32667 = CARTESIAN_POINT ( 'NONE',  ( 6.197074855318628117, 31.00000000000000355, 46.98549035852928313 ) ) ;
#32668 = CARTESIAN_POINT ( 'NONE',  ( 0.000000000000000000, 6.007673836298004666, 35.49518073029998533 ) ) ;
#32669 = VERTEX_POINT ( 'NONE', #38182 ) ;
#32670 = CARTESIAN_POINT ( 'NONE',  ( 17.99999999999999645, -103.4151313792866489, -61.85306461934516875 ) ) ;
#32671 = CARTESIAN_POINT ( 'NONE',  ( 74.49266661913014786, 31.00000000000000000, 43.00976416799198176 ) ) ;
#32672 = EDGE_CURVE ( 'NONE', #31034, #21299, #14214, .T. ) ;
#32673 = CARTESIAN_POINT ( 'NONE',  ( 17.99999999999999645, -104.6166166098448826, 50.11350645393640235 ) ) ;
#32674 = EDGE_LOOP ( 'NONE', ( #21001, #10098, #20898, #41093 ) ) ;
#32675 = CARTESIAN_POINT ( 'NONE',  ( -40.14822235767833547, 31.00000000000000355, 45.62378674120104449 ) ) ;
#32676 = EDGE_CURVE ( 'NONE', #17317, #30034, #42851, .T. ) ;
#32677 = CARTESIAN_POINT ( 'NONE',  ( 41.67488199336423804, 40.00000000000000000, 54.49293397273886086 ) ) ;
#32678 = CARTESIAN_POINT ( 'NONE',  ( -106.4195705685741871, -106.4195705685773135, 9.999999999999751310 ) ) ;
#32679 = ORIENTED_EDGE ( 'NONE', *, *, #38829, .T. ) ;
#32680 = DIRECTION ( 'NONE',  ( -1.000000000000000000, -0.000000000000000000, -0.000000000000000000 ) ) ;
#32681 = CARTESIAN_POINT ( 'NONE',  ( -6.999999999999999112, 4.546351088565595293E-15, 0.000000000000000000 ) ) ;
#32682 = CARTESIAN_POINT ( 'NONE',  ( 42.80287614962723808, -35.35525454449572180, 69.29271901957299917 ) ) ;
#32683 = AXIS2_PLACEMENT_3D ( 'NONE', #1402, #34796, #11254 ) ;
#32684 = CIRCLE ( 'NONE', #20177, 20.00000000000000355 ) ;
#32686 = ORIENTED_EDGE ( 'NONE', *, *, #32486, .F. ) ;
#32685 = CARTESIAN_POINT ( 'NONE',  ( 17.99999999999999645, -31.80866420683989304, -2.997093558041628025 ) ) ;
#32687 = DIRECTION ( 'NONE',  ( -1.000000000000000000, 0.000000000000000000, 0.000000000000000000 ) ) ;
#32688 = CARTESIAN_POINT ( 'NONE',  ( 17.99999999999999645, -13.22719389141960100, -28.58720592780609593 ) ) ;
#32689 = AXIS2_PLACEMENT_3D ( 'NONE', #33865, #39536, #36259 ) ;
#32690 = EDGE_CURVE ( 'NONE', #18694, #36912, #3129, .T. ) ;
#32691 = CARTESIAN_POINT ( 'NONE',  ( 9.510694223897102617, 40.00000000000000000, -72.24097909213479340 ) ) ;
#32692 = DIRECTION ( 'NONE',  ( 0.000000000000000000, 0.000000000000000000, -1.000000000000000000 ) ) ;
#32693 = VERTEX_POINT ( 'NONE', #38391 ) ;
#32694 = CARTESIAN_POINT ( 'NONE',  ( 0.000000000000000000, 0.000000000000000000, 0.000000000000000000 ) ) ;
#32695 = CARTESIAN_POINT ( 'NONE',  ( -23.00000000000000000, 0.000000000000000000, -20.00000000000000000 ) ) ;
#32696 = ORIENTED_EDGE ( 'NONE', *, *, #24865, .T. ) ;
#32697 = EDGE_CURVE ( 'NONE', #42073, #23910, #13652, .T. ) ;
#32698 = VERTEX_POINT ( 'NONE', #8720 ) ;
#32699 = CARTESIAN_POINT ( 'NONE',  ( 0.000000000000000000, 0.000000000000000000, 0.000000000000000000 ) ) ;
#32700 = EDGE_LOOP ( 'NONE', ( #21584, #42189, #17594, #40905 ) ) ;
#32701 = DIRECTION ( 'NONE',  ( -1.000000000000000000, 0.000000000000000000, -0.000000000000000000 ) ) ;
#32702 = DIRECTION ( 'NONE',  ( -3.996523416598930318E-16, 2.658563593772947863E-15, 1.000000000000000000 ) ) ;
#32703 = EDGE_CURVE ( 'NONE', #28999, #41125, #40764, .T. ) ;
#32704 = CARTESIAN_POINT ( 'NONE',  ( 0.000000000000000000, 42.87700105098607395, 107.7847984684006377 ) ) ;
#32705 = DIRECTION ( 'NONE',  ( 0.000000000000000000, 0.000000000000000000, 1.000000000000000000 ) ) ;
#32706 = VERTEX_POINT ( 'NONE', #42299 ) ;
#32707 = CYLINDRICAL_SURFACE ( 'NONE', #9822, 120.5010000000000190 ) ;
#32708 = VERTEX_POINT ( 'NONE', #5458 ) ;
#32709 = CIRCLE ( 'NONE', #39048, 59.00000000000000000 ) ;
#32710 = CARTESIAN_POINT ( 'NONE',  ( 0.000000000000000000, 47.32430374665963058, -21.55018039121477713 ) ) ;
#32711 = ADVANCED_FACE ( 'NONE', ( #28813 ), #28607, .T. ) ;
#32712 = ORIENTED_EDGE ( 'NONE', *, *, #12100, .T. ) ;
#32713 = DIRECTION ( 'NONE',  ( 0.000000000000000000, 0.000000000000000000, 1.000000000000000000 ) ) ;
#32714 = CARTESIAN_POINT ( 'NONE',  ( -10.00000000000000000, 0.000000000000000000, 0.000000000000000000 ) ) ;
#32715 = CIRCLE ( 'NONE', #23597, 120.5010000000000332 ) ;
#32716 = CARTESIAN_POINT ( 'NONE',  ( 17.99999999999999645, 0.000000000000000000, 0.000000000000000000 ) ) ;
#32717 = CARTESIAN_POINT ( 'NONE',  ( 62.51641183113888900, 31.00000000000000000, -16.75201923384928548 ) ) ;
#32718 = CARTESIAN_POINT ( 'NONE',  ( 130.0000000000000000, 1.638195277402996435E-14, 6.938893903907228378E-15 ) ) ;
#32719 = ADVANCED_FACE ( 'NONE', ( #11815 ), #25140, .F. ) ;
#32720 = EDGE_CURVE ( 'NONE', #37013, #9440, #5994, .T. ) ;
#32721 = ORIENTED_EDGE ( 'NONE', *, *, #4012, .F. ) ;
#32722 = CARTESIAN_POINT ( 'NONE',  ( -18.66214908251421534, 31.00000000000000355, 24.25811346063288454 ) ) ;
#32723 = EDGE_CURVE ( 'NONE', #28707, #12063, #29011, .T. ) ;
#32724 = ADVANCED_FACE ( 'NONE', ( #18601 ), #12232, .F. ) ;
#32725 = CARTESIAN_POINT ( 'NONE',  ( 44.85399723358655422, 40.00000000000000000, -58.47732767552992073 ) ) ;
#32726 = CYLINDRICAL_SURFACE ( 'NONE', #31156, 13.59999999999999964 ) ;
#32727 = DIRECTION ( 'NONE',  ( -1.000000000000000000, -0.000000000000000000, -0.000000000000000000 ) ) ;
#32728 = DIRECTION ( 'NONE',  ( -1.000000000000000000, -0.000000000000000000, -0.000000000000000000 ) ) ;
#32729 = CARTESIAN_POINT ( 'NONE',  ( 18.00000000000000355, 0.000000000000000000, 0.000000000000000000 ) ) ;
#32730 = ORIENTED_EDGE ( 'NONE', *, *, #686, .T. ) ;
#32731 = CARTESIAN_POINT ( 'NONE',  ( 2.781618486875130358, 40.00000000000000000, -42.60416666509636485 ) ) ;
#32732 = DIRECTION ( 'NONE',  ( -1.000000000000000000, -0.000000000000000000, -0.000000000000000000 ) ) ;
#32734 = CARTESIAN_POINT ( 'NONE',  ( -2.095696658341510008E-13, 150.5000000000013642, 7.000000000000419220 ) ) ;
#32733 = CIRCLE ( 'NONE', #668, 58.99999999999999289 ) ;
#32735 = AXIS2_PLACEMENT_3D ( 'NONE', #4942, #4488, #17865 ) ;
#32736 = ORIENTED_EDGE ( 'NONE', *, *, #1705, .T. ) ;
#32737 = CIRCLE ( 'NONE', #12554, 59.00000000000000711 ) ;
#32738 = CARTESIAN_POINT ( 'NONE',  ( 17.99999999999999645, -19.69434969228056787, -24.58291258574069360 ) ) ;
#32739 = DIRECTION ( 'NONE',  ( 1.000000000000000000, 0.000000000000000000, 0.000000000000000000 ) ) ;
#32740 = ORIENTED_EDGE ( 'NONE', *, *, #26730, .T. ) ;
#32741 = DIRECTION ( 'NONE',  ( 0.000000000000000000, -0.7865515558026479059, 0.6175246149461850464 ) ) ;
#32742 = VERTEX_POINT ( 'NONE', #35336 ) ;
#32743 = ORIENTED_EDGE ( 'NONE', *, *, #31777, .F. ) ;
#32744 = DIRECTION ( 'NONE',  ( 0.000000000000000000, 0.000000000000000000, 1.000000000000000000 ) ) ;
#32745 = CARTESIAN_POINT ( 'NONE',  ( 59.96221986557396377, 31.00000000000000355, 78.35452998770438171 ) ) ;
#32746 = ORIENTED_EDGE ( 'NONE', *, *, #1976, .F. ) ;
#32747 = CARTESIAN_POINT ( 'NONE',  ( 17.99999999999999645, 0.000000000000000000, 0.000000000000000000 ) ) ;
#32748 = EDGE_CURVE ( 'NONE', #22186, #27071, #31772, .T. ) ;
#32749 = DIRECTION ( 'NONE',  ( 1.000000000000000000, 0.000000000000000000, 0.000000000000000000 ) ) ;
#32750 = DIRECTION ( 'NONE',  ( -1.000000000000000000, -0.000000000000000000, 0.000000000000000000 ) ) ;
#32751 = ORIENTED_EDGE ( 'NONE', *, *, #14557, .T. ) ;
#32752 = CARTESIAN_POINT ( 'NONE',  ( -99.67789407897798526, 17.11489954122025736, -5.066036069491909544 ) ) ;
#32753 = DIRECTION ( 'NONE',  ( 1.000000000000000000, 0.000000000000000000, 0.000000000000000000 ) ) ;
#32754 = DIRECTION ( 'NONE',  ( -1.000000000000000000, 3.035766082959412415E-17, 0.000000000000000000 ) ) ;
#32755 = AXIS2_PLACEMENT_3D ( 'NONE', #3452, #23583, #39675 ) ;
#32757 = CYLINDRICAL_SURFACE ( 'NONE', #21291, 59.00000000000000000 ) ;
#32756 = DIRECTION ( 'NONE',  ( -1.000000000000000000, 0.000000000000000000, 0.000000000000000000 ) ) ;
#32758 = DIRECTION ( 'NONE',  ( 1.000000000000000000, 0.000000000000000000, 0.000000000000000000 ) ) ;
#32759 = ORIENTED_EDGE ( 'NONE', *, *, #25053, .F. ) ;
#32760 = FILL_AREA_STYLE_COLOUR ( '', #12827 ) ;
#32761 = CARTESIAN_POINT ( 'NONE',  ( 20.70971545910534672, 31.00000000000000355, 15.87948211774388518 ) ) ;
#32762 = CIRCLE ( 'NONE', #38346, 14.99999999999999822 ) ;
#32763 = ORIENTED_EDGE ( 'NONE', *, *, #23264, .F. ) ;
#32764 = CARTESIAN_POINT ( 'NONE',  ( 17.99999999999999645, -16.77727049691128869, 27.19001440037539297 ) ) ;
#32765 = CIRCLE ( 'NONE', #16774, 13.59999999999999964 ) ;
#32766 = CIRCLE ( 'NONE', #33456, 47.49900000000000233 ) ;
#32767 = CARTESIAN_POINT ( 'NONE',  ( 0.000000000000000000, 31.80866420683995699, -2.997093558040963224 ) ) ;
#32768 = ORIENTED_EDGE ( 'NONE', *, *, #17361, .T. ) ;
#32769 = EDGE_CURVE ( 'NONE', #33431, #36528, #1956, .T. ) ;
#32770 = ADVANCED_FACE ( 'NONE', ( #31639 ), #2160, .T. ) ;
#32771 = CIRCLE ( 'NONE', #13992, 31.49899999999999878 ) ;
#32772 = CARTESIAN_POINT ( 'NONE',  ( 0.000000000000000000, 0.000000000000000000, 0.000000000000000000 ) ) ;
#32773 = CARTESIAN_POINT ( 'NONE',  ( -2.781618486875174767, 40.00000000000000000, -42.39583333490362804 ) ) ;
#32774 = CARTESIAN_POINT ( 'NONE',  ( -12.95950413119146205, 40.00000000000000000, 37.95406330258916938 ) ) ;
#32775 = ADVANCED_FACE ( 'NONE', ( #41877 ), #25559, .T. ) ;
#32776 = VERTEX_POINT ( 'NONE', #12026 ) ;
#32777 = ORIENTED_EDGE ( 'NONE', *, *, #15852, .T. ) ;
#32778 = DIRECTION ( 'NONE',  ( -3.614007241618348771E-16, 1.000000000000000000, 0.000000000000000000 ) ) ;
#32779 = CYLINDRICAL_SURFACE ( 'NONE', #33906, 116.0000000000000000 ) ;
#32780 = DIRECTION ( 'NONE',  ( 1.000000000000000000, 0.000000000000000000, 0.000000000000000000 ) ) ;
#32781 = FACE_OUTER_BOUND ( 'NONE', #6769, .T. ) ;
#32782 = CYLINDRICAL_SURFACE ( 'NONE', #6972, 116.0000000000000000 ) ;
#32783 = ORIENTED_EDGE ( 'NONE', *, *, #34748, .F. ) ;
#32784 = CARTESIAN_POINT ( 'NONE',  ( -8.749793197483592522, 117.9447454555042754, 2.972870684497274762 ) ) ;
#32785 = VERTEX_POINT ( 'NONE', #9147 ) ;
#32786 = DIRECTION ( 'NONE',  ( 0.000000000000000000, 0.4999999999999990008, -0.8660254037844391517 ) ) ;
#32787 = DIRECTION ( 'NONE',  ( -1.000000000000000000, 0.000000000000000000, 0.000000000000000000 ) ) ;
#32788 = EDGE_CURVE ( 'NONE', #27036, #11189, #2485, .T. ) ;
#32789 = CIRCLE ( 'NONE', #24493, 116.0000000000000000 ) ;
#32790 = FACE_OUTER_BOUND ( 'NONE', #4647, .T. ) ;
#32791 = DIRECTION ( 'NONE',  ( 0.000000000000000000, -0.9407002666710296834, -0.3392388661180399945 ) ) ;
#32792 = VERTEX_POINT ( 'NONE', #8299 ) ;
#32793 = CYLINDRICAL_SURFACE ( 'NONE', #6153, 51.99999999999999289 ) ;
#32794 = VERTEX_POINT ( 'NONE', #25345 ) ;
#32795 = CIRCLE ( 'NONE', #3493, 13.60000000000000320 ) ;
#32796 = CARTESIAN_POINT ( 'NONE',  ( 0.000000000000000000, -46.21320724403641123, -10.97699764142002010 ) ) ;
#32797 = ORIENTED_EDGE ( 'NONE', *, *, #7869, .F. ) ;
#32799 = ORIENTED_EDGE ( 'NONE', *, *, #32876, .T. ) ;
#32798 = FACE_OUTER_BOUND ( 'NONE', #16771, .T. ) ;
#32800 = VECTOR ( 'NONE', #11206, 1000.000000000000000 ) ;
#32801 = CARTESIAN_POINT ( 'NONE',  ( -30.89738163651153258, 31.00000000000000355, 40.13100860029957317 ) ) ;
#32803 = ORIENTED_EDGE ( 'NONE', *, *, #39165, .T. ) ;
#32802 = CIRCLE ( 'NONE', #31425, 10.99999999999999645 ) ;
#32804 = FACE_OUTER_BOUND ( 'NONE', #8213, .T. ) ;
#32805 = VECTOR ( 'NONE', #14361, 1000.000000000000000 ) ;
#32806 = VERTEX_POINT ( 'NONE', #8946 ) ;
#32807 = DIRECTION ( 'NONE',  ( -1.000000000000000000, 0.000000000000000000, 0.000000000000000000 ) ) ;
#32808 = ORIENTED_EDGE ( 'NONE', *, *, #12443, .F. ) ;
#32809 = CARTESIAN_POINT ( 'NONE',  ( 27.50146173784981229, 40.00000000000000000, -80.63904244945182143 ) ) ;
#32810 = AXIS2_PLACEMENT_3D ( 'NONE', #6301, #32917, #23785 ) ;
#32812 = DIRECTION ( 'NONE',  ( 0.000000000000000000, -0.5076658003388467844, 0.8615540813938020737 ) ) ;
#32811 = CYLINDRICAL_SURFACE ( 'NONE', #1506, 120.5010000000000190 ) ;
#32813 = DIRECTION ( 'NONE',  ( 1.000000000000000000, 0.000000000000000000, 0.000000000000000000 ) ) ;
#32814 = EDGE_LOOP ( 'NONE', ( #25782, #22689, #9029, #5912 ) ) ;
#32815 = CARTESIAN_POINT ( 'NONE',  ( 17.99999999999999645, 120.4984140710909344, -0.7894348306988416830 ) ) ;
#32816 = VERTEX_POINT ( 'NONE', #22291 ) ;
#32817 = CARTESIAN_POINT ( 'NONE',  ( 17.99999999999999645, 0.000000000000000000, 0.000000000000000000 ) ) ;
#32818 = LINE ( 'NONE', #9482, #39318 ) ;
#32819 = CARTESIAN_POINT ( 'NONE',  ( 75.10416666583130052, 31.00000000000000000, 4.908738512847474311 ) ) ;
#32821 = CARTESIAN_POINT ( 'NONE',  ( 17.99999999999999645, -30.74337109795225942, 8.695908345466005329 ) ) ;
#32820 = CYLINDRICAL_SURFACE ( 'NONE', #35140, 120.5010000000000190 ) ;
#32822 = ORIENTED_EDGE ( 'NONE', *, *, #21843, .T. ) ;
#32823 = EDGE_CURVE ( 'NONE', #3211, #35058, #19269, .T. ) ;
#32824 = VECTOR ( 'NONE', #38930, 1000.000000000000000 ) ;
#32825 = DIRECTION ( 'NONE',  ( 1.000000000000000000, -0.000000000000000000, -0.000000000000000000 ) ) ;
#32826 = VECTOR ( 'NONE', #41106, 1000.000000000000000 ) ;
#32827 = APPLICATION_CONTEXT ( 'automotive_design' ) ;
#32828 = AXIS2_PLACEMENT_3D ( 'NONE', #23829, #34413, #36224 ) ;
#32829 = ORIENTED_EDGE ( 'NONE', *, *, #20420, .T. ) ;
#32830 = CARTESIAN_POINT ( 'NONE',  ( 18.00000000000000355, -32.32520163883607722, 34.09746168776025854 ) ) ;
#32831 = DIRECTION ( 'NONE',  ( 1.000000000000000000, 0.000000000000000000, 0.000000000000000000 ) ) ;
#32832 = CARTESIAN_POINT ( 'NONE',  ( 59.96221986557396377, 31.00000000000000355, 78.35452998770438171 ) ) ;
#32833 = CARTESIAN_POINT ( 'NONE',  ( 63.29164158768324455, 39.99999999999999289, -71.97807289018581400 ) ) ;
#32834 = EDGE_CURVE ( 'NONE', #12461, #17650, #3887, .T. ) ;
#32835 = AXIS2_PLACEMENT_3D ( 'NONE', #11462, #21100, #4900 ) ;
#32836 = CARTESIAN_POINT ( 'NONE',  ( 17.99999999999999645, 0.000000000000000000, 0.000000000000000000 ) ) ;
#32837 = EDGE_CURVE ( 'NONE', #33425, #21541, #29029, .T. ) ;
#32838 = DIRECTION ( 'NONE',  ( -1.000000000000000000, 0.000000000000000000, -0.000000000000000000 ) ) ;
#32839 = ORIENTED_EDGE ( 'NONE', *, *, #33708, .T. ) ;
#32840 = DIRECTION ( 'NONE',  ( 0.000000000000000000, 0.000000000000000000, 1.000000000000000000 ) ) ;
#32841 = EDGE_LOOP ( 'NONE', ( #4408, #28441, #31570, #3554 ) ) ;
#32842 = VECTOR ( 'NONE', #37588, 1000.000000000000000 ) ;
#32843 = DIRECTION ( 'NONE',  ( 0.000000000000000000, -0.1590634960190596414, -0.9872683547213465527 ) ) ;
#32844 = EDGE_CURVE ( 'NONE', #14699, #35634, #9791, .T. ) ;
#32845 = CARTESIAN_POINT ( 'NONE',  ( 17.99999999999999645, 105.7179949885867956, -37.57629584241721687 ) ) ;
#32846 = CARTESIAN_POINT ( 'NONE',  ( -8.749793197483596074, -2.055254544495723312, 2.972870684497275207 ) ) ;
#32847 = ORIENTED_EDGE ( 'NONE', *, *, #35108, .F. ) ;
#32848 = DIRECTION ( 'NONE',  ( 1.000000000000000000, -0.000000000000000000, -0.000000000000000000 ) ) ;
#32849 = FACE_OUTER_BOUND ( 'NONE', #13022, .T. ) ;
#32850 = CARTESIAN_POINT ( 'NONE',  ( 17.99999999999999645, -41.33768078145432412, -104.3046912715545318 ) ) ;
#32852 = ORIENTED_EDGE ( 'NONE', *, *, #16579, .F. ) ;
#32851 = DIRECTION ( 'NONE',  ( -0.3806385939525924744, 0.000000000000000000, 0.9247238835424298475 ) ) ;
#32853 = CARTESIAN_POINT ( 'NONE',  ( 20.65150112226810819, 31.00000000000000355, -15.81946110361252522 ) ) ;
#32854 = CARTESIAN_POINT ( 'NONE',  ( -31.75000000000000000, 0.000000000000000000, 0.000000000000000000 ) ) ;
#32856 = ORIENTED_EDGE ( 'NONE', *, *, #28220, .F. ) ;
#32855 = DIRECTION ( 'NONE',  ( 0.000000000000000000, 0.000000000000000000, 1.000000000000000000 ) ) ;
#32857 = ORIENTED_EDGE ( 'NONE', *, *, #34966, .F. ) ;
#32858 = DIRECTION ( 'NONE',  ( 1.000000000000000000, 0.000000000000000000, 0.000000000000000000 ) ) ;
#32860 = EDGE_CURVE ( 'NONE', #35004, #43080, #25538, .T. ) ;
#32859 = AXIS2_PLACEMENT_3D ( 'NONE', #42, #13410, #39972 ) ;
#32861 = LINE ( 'NONE', #32436, #22475 ) ;
#32862 = CARTESIAN_POINT ( 'NONE',  ( -17.88900094062007184, 40.00000000000000000, 36.12696699726038219 ) ) ;
#32863 = LINE ( 'NONE', #3384, #11844 ) ;
#32864 = AXIS2_PLACEMENT_3D ( 'NONE', #11970, #28760, #27907 ) ;
#32865 = DIRECTION ( 'NONE',  ( -1.000000000000000000, 0.000000000000000000, -0.000000000000000000 ) ) ;
#32866 = AXIS2_PLACEMENT_3D ( 'NONE', #40658, #953, #37405 ) ;
#32867 = FACE_OUTER_BOUND ( 'NONE', #34, .T. ) ;
#32868 = EDGE_LOOP ( 'NONE', ( #26213, #26930, #27255, #21801 ) ) ;
#32869 = DIRECTION ( 'NONE',  ( -1.000000000000000000, 0.000000000000000000, -0.000000000000000000 ) ) ;
#32870 = VERTEX_POINT ( 'NONE', #152 ) ;
#32871 = DIRECTION ( 'NONE',  ( 1.000000000000000000, 0.000000000000000000, 0.000000000000000000 ) ) ;
#32872 = CARTESIAN_POINT ( 'NONE',  ( -10.00000000000000000, 0.000000000000000000, 0.000000000000000000 ) ) ;
#32873 = CARTESIAN_POINT ( 'NONE',  ( -13.51098712749246467, 31.00000000000000355, -50.41620372279128048 ) ) ;
#32874 = CARTESIAN_POINT ( 'NONE',  ( 0.000000000000000000, 0.000000000000000000, 0.000000000000000000 ) ) ;
#32875 = ORIENTED_EDGE ( 'NONE', *, *, #32220, .T. ) ;
#32876 = EDGE_CURVE ( 'NONE', #14639, #28956, #622, .T. ) ;
#32877 = CARTESIAN_POINT ( 'NONE',  ( 0.000000000000000000, 74.56001736500736854, -88.86396238368961065 ) ) ;
#32878 = CARTESIAN_POINT ( 'NONE',  ( -80.23695839127151430, 31.00000000000000711, 39.56677620416681407 ) ) ;
#32879 = B_SPLINE_CURVE_WITH_KNOTS ( 'NONE', 3,
 ( #28015, #11212, #15151, #34961, #5288, #37796 ),
 .UNSPECIFIED., .F., .F.,
 ( 4, 2, 4 ),
 ( 0.002452478801916376308, 0.003676905084148007850, 0.004901331366379639391 ),
 .UNSPECIFIED. ) ;
#32880 = DIRECTION ( 'NONE',  ( 0.000000000000000000, -1.246648735278247733E-14, -1.000000000000000000 ) ) ;
#32881 = ORIENTED_EDGE ( 'NONE', *, *, #6924, .T. ) ;
#32882 = CARTESIAN_POINT ( 'NONE',  ( -4.660665814385270167, 31.00000000000000355, 69.59371722956201722 ) ) ;
#32883 = CARTESIAN_POINT ( 'NONE',  ( 54.03410584561684971, 40.00000000000000000, 41.58544482236945328 ) ) ;
#32884 = CARTESIAN_POINT ( 'NONE',  ( -43.52407497442469264, 40.00000000000000000, 88.29422169633753015 ) ) ;
#32885 = ADVANCED_FACE ( 'NONE', ( #10221 ), #2993, .T. ) ;
#32886 = VECTOR ( 'NONE', #16820, 1000.000000000000000 ) ;
#32887 = ORIENTED_EDGE ( 'NONE', *, *, #10832, .T. ) ;
#32888 = AXIS2_PLACEMENT_3D ( 'NONE', #40573, #29940, #10708 ) ;
#32889 = DIRECTION ( 'NONE',  ( -1.000000000000000000, 0.000000000000000000, 0.000000000000000000 ) ) ;
#32890 = VECTOR ( 'NONE', #6167, 1000.000000000000000 ) ;
#32891 = CARTESIAN_POINT ( 'NONE',  ( 5.200000000000002842, 0.000000000000000000, -2.700000000000000622 ) ) ;
#32892 = LINE ( 'NONE', #16332, #32416 ) ;
#32893 = CIRCLE ( 'NONE', #38462, 116.0000000000000000 ) ;
#32895 = ORIENTED_EDGE ( 'NONE', *, *, #10611, .T. ) ;
#32894 = CARTESIAN_POINT ( 'NONE',  ( 4.024499207728657879, 2.323545700935571556, -3.572172305156506411 ) ) ;
#32896 = EDGE_CURVE ( 'NONE', #7662, #29305, #13313, .T. ) ;
#32897 = CARTESIAN_POINT ( 'NONE',  ( -10.00000000000000000, 0.000000000000000000, 0.000000000000000000 ) ) ;
#32898 = ORIENTED_EDGE ( 'NONE', *, *, #14298, .T. ) ;
#32899 = DIRECTION ( 'NONE',  ( 0.000000000000000000, 0.000000000000000000, 1.000000000000000000 ) ) ;
#32900 = CARTESIAN_POINT ( 'NONE',  ( -56.48955861152074220, 40.00000000000000711, -43.32902275383659685 ) ) ;
#32901 = DIRECTION ( 'NONE',  ( -1.000000000000000000, 0.000000000000000000, 0.000000000000000000 ) ) ;
#32902 = AXIS2_PLACEMENT_3D ( 'NONE', #24938, #37963, #31443 ) ;
#32903 = ORIENTED_EDGE ( 'NONE', *, *, #14931, .T. ) ;
#32904 = CARTESIAN_POINT ( 'NONE',  ( 17.99999999999999645, -73.51007459736368332, -89.73443560133438268 ) ) ;
#32905 = CARTESIAN_POINT ( 'NONE',  ( 6.600000000000001421, 7.044548050363292547E-15, 0.000000000000000000 ) ) ;
#32906 = ORIENTED_EDGE ( 'NONE', *, *, #25722, .T. ) ;
#32907 = ORIENTED_EDGE ( 'NONE', *, *, #27841, .F. ) ;
#32908 = CARTESIAN_POINT ( 'NONE',  ( 18.00000000000000355, -47.00885577955416039, 6.806061952192135500 ) ) ;
#32910 = ORIENTED_EDGE ( 'NONE', *, *, #30013, .F. ) ;
#32909 = EDGE_CURVE ( 'NONE', #38864, #25476, #36836, .T. ) ;
#32911 = DIRECTION ( 'NONE',  ( 0.000000000000000000, 0.000000000000000000, 1.000000000000000000 ) ) ;
#32912 = DIRECTION ( 'NONE',  ( 0.000000000000000000, -0.6382441836448108363, -0.7698339834299139373 ) ) ;
#32913 = EDGE_CURVE ( 'NONE', #35004, #30836, #7396, .T. ) ;
#32914 = CARTESIAN_POINT ( 'NONE',  ( 17.99999999999999645, 111.9370513079669394, 44.61600100275212100 ) ) ;
#32915 = FACE_OUTER_BOUND ( 'NONE', #30874, .T. ) ;
#32916 = ORIENTED_EDGE ( 'NONE', *, *, #22730, .T. ) ;
#32917 = DIRECTION ( 'NONE',  ( 3.009274222672345096E-17, 1.000000000000000000, -2.455023325076455345E-18 ) ) ;
#32918 = UNCERTAINTY_MEASURE_WITH_UNIT (LENGTH_MEASURE( 1.000000000000000082E-05 ), #29043, 'distance_accuracy_value', 'NONE');
#32919 = ORIENTED_EDGE ( 'NONE', *, *, #16974, .T. ) ;
#32920 = CIRCLE ( 'NONE', #32244, 20.00000000000000711 ) ;
#32921 = AXIS2_PLACEMENT_3D ( 'NONE', #14898, #28837, #38624 ) ;
#32922 = DIRECTION ( 'NONE',  ( 0.000000000000000000, 0.000000000000000000, 1.000000000000000000 ) ) ;
#32923 = ORIENTED_EDGE ( 'NONE', *, *, #18243, .F. ) ;
#32924 = CARTESIAN_POINT ( 'NONE',  ( 0.000000000000000000, 111.9370513079669394, 44.61600100275212100 ) ) ;
#32925 = CIRCLE ( 'NONE', #861, 99.99999999999994316 ) ;
#32926 = DIRECTION ( 'NONE',  ( 1.000000000000000000, 0.000000000000000000, 0.000000000000000000 ) ) ;
#32927 = PRODUCT_CONTEXT ( 'NONE', #5251, 'mechanical' ) ;
#32928 = CARTESIAN_POINT ( 'NONE',  ( -0.5999999999999996447, -12.75000000000000000, -1.199999999999999956 ) ) ;
#32929 = CARTESIAN_POINT ( 'NONE',  ( -51.34291522965900612, 31.00000000000000355, 29.65708359768123970 ) ) ;
#32930 = AXIS2_PLACEMENT_3D ( 'NONE', #41396, #35077, #8469 ) ;
#32931 = EDGE_LOOP ( 'NONE', ( #25383, #12394, #20334, #31151 ) ) ;
#32932 = CARTESIAN_POINT ( 'NONE',  ( 31.41502175087182991, 31.00000000000000355, -18.07270130326418922 ) ) ;
#32933 = CARTESIAN_POINT ( 'NONE',  ( -66.92166868300088822, 40.00000000000000711, -22.71661802240650019 ) ) ;
#32934 = EDGE_CURVE ( 'NONE', #22441, #10216, #30402, .T. ) ;
#32935 = DIRECTION ( 'NONE',  ( -1.000000000000000000, -0.000000000000000000, -0.000000000000000000 ) ) ;
#32936 = DIRECTION ( 'NONE',  ( 0.02040816326530612776, -0.9997917317482359900, 0.000000000000000000 ) ) ;
#32937 = ADVANCED_FACE ( 'NONE', ( #29667 ), #33564, .T. ) ;
#32938 = ADVANCED_FACE ( 'NONE', ( #32915 ), #6299, .F. ) ;
#32939 = DIRECTION ( 'NONE',  ( 1.000000000000000000, 0.000000000000000000, -3.273063162220416457E-16 ) ) ;
#32940 = DIRECTION ( 'NONE',  ( 1.000000000000000000, 0.000000000000000000, 0.000000000000000000 ) ) ;
#32941 = AXIS2_PLACEMENT_3D ( 'NONE', #6681, #40685, #16544 ) ;
#32942 = ORIENTED_EDGE ( 'NONE', *, *, #30969, .F. ) ;
#32943 = CARTESIAN_POINT ( 'NONE',  ( -15.46676570949300000, 40.00000000000000000, 45.57083133015776610 ) ) ;
#32944 = CYLINDRICAL_SURFACE ( 'NONE', #10333, 120.5010000000000190 ) ;
#32945 = LINE ( 'NONE', #32524, #31224 ) ;
#32946 = ORIENTED_EDGE ( 'NONE', *, *, #3285, .T. ) ;
#32947 = CARTESIAN_POINT ( 'NONE',  ( 0.000000000000000000, 16.86122981692056655, -27.13802899033274940 ) ) ;
#32948 = CARTESIAN_POINT ( 'NONE',  ( -2.797566391619251075E-15, 1.860994515641065082E-14, 7.000000000000002665 ) ) ;
#32949 = ORIENTED_EDGE ( 'NONE', *, *, #40981, .F. ) ;
#32950 = DIRECTION ( 'NONE',  ( 1.000000000000000000, 0.000000000000000000, 0.000000000000000000 ) ) ;
#32951 = ORIENTED_EDGE ( 'NONE', *, *, #42840, .F. ) ;
#32952 = CIRCLE ( 'NONE', #21153, 47.49900000000001654 ) ;
#32953 = ORIENTED_EDGE ( 'NONE', *, *, #42963, .T. ) ;
#32954 = LINE ( 'NONE', #33394, #16745 ) ;
#32955 = EDGE_CURVE ( 'NONE', #34051, #13299, #15770, .T. ) ;
#32956 = CARTESIAN_POINT ( 'NONE',  ( -5.980347265640405752, 31.00000000000000355, 89.59238221257746204 ) ) ;
#32957 = ORIENTED_EDGE ( 'NONE', *, *, #17519, .F. ) ;
#32958 = DIRECTION ( 'NONE',  ( 0.000000000000000000, 9.408669700213189617E-16, -1.000000000000000000 ) ) ;
#32959 = ADVANCED_FACE ( 'NONE', ( #39873 ), #19441, .T. ) ;
#32960 = EDGE_CURVE ( 'NONE', #29952, #12461, #33875, .T. ) ;
#32961 = EDGE_CURVE ( 'NONE', #39267, #37232, #23348, .T. ) ;
#32962 = CYLINDRICAL_SURFACE ( 'NONE', #9413, 51.99999999999999289 ) ;
#32963 = LINE ( 'NONE', #30355, #12251 ) ;
#32964 = VERTEX_POINT ( 'NONE', #16149 ) ;
#32965 = CARTESIAN_POINT ( 'NONE',  ( 17.99999999999999645, 0.000000000000000000, 0.000000000000000000 ) ) ;
#32966 = LINE ( 'NONE', #3045, #3175 ) ;
#32968 = CARTESIAN_POINT ( 'NONE',  ( 17.99999999999999645, 57.40245293794799153, -96.40140491896575270 ) ) ;
#32967 = DIRECTION ( 'NONE',  ( 1.000000000000000000, 0.000000000000000000, 0.000000000000000000 ) ) ;
#32969 = VECTOR ( 'NONE', #14451, 1000.000000000000000 ) ;
#32970 = CYLINDRICAL_SURFACE ( 'NONE', #6804, 59.00000000000000000 ) ;
#32971 = VERTEX_POINT ( 'NONE', #36609 ) ;
#32972 = VECTOR ( 'NONE', #8108, 1000.000000000000000 ) ;
#32973 = CARTESIAN_POINT ( 'NONE',  ( -29.44516979616424024, 31.00000000000000355, -7.879824757621473275 ) ) ;
#32974 = VERTEX_POINT ( 'NONE', #19648 ) ;
#32975 = FACE_OUTER_BOUND ( 'NONE', #15073, .T. ) ;
#32976 = CARTESIAN_POINT ( 'NONE',  ( 0.000000000000000000, -35.11945359308136716, 38.34871548466002622 ) ) ;
#32977 = VERTEX_POINT ( 'NONE', #42712 ) ;
#32978 = FACE_OUTER_BOUND ( 'NONE', #41542, .T. ) ;
#32979 = CARTESIAN_POINT ( 'NONE',  ( -37.46020281470095625, 40.00000000000000000, 12.72710441276525017 ) ) ;
#32980 = MECHANICAL_DESIGN_GEOMETRIC_PRESENTATION_REPRESENTATION (  '', ( #28161 ), #921 ) ;
#32981 = CARTESIAN_POINT ( 'NONE',  ( -2.829072032612394594, 40.00000000000000000, -44.39959014221900446 ) ) ;
#32982 = EDGE_CURVE ( 'NONE', #33745, #6849, #4586, .T. ) ;
#32983 = CIRCLE ( 'NONE', #16291, 116.0000000000000000 ) ;
#32984 = ORIENTED_EDGE ( 'NONE', *, *, #29179, .T. ) ;
#32985 = ORIENTED_EDGE ( 'NONE', *, *, #18394, .T. ) ;
#32986 = FACE_OUTER_BOUND ( 'NONE', #31868, .T. ) ;
#32987 = FACE_OUTER_BOUND ( 'NONE', #10136, .T. ) ;
#32988 = LINE ( 'NONE', #25842, #19689 ) ;
#32989 = CARTESIAN_POINT ( 'NONE',  ( 0.000000000000000000, 110.3490479609632615, 38.71798610214565173 ) ) ;
#32990 = VERTEX_POINT ( 'NONE', #9586 ) ;
#32991 = DIRECTION ( 'NONE',  ( -1.000000000000000000, 0.000000000000000000, -0.000000000000000000 ) ) ;
#32992 = ORIENTED_EDGE ( 'NONE', *, *, #17308, .F. ) ;
#32993 = DIRECTION ( 'NONE',  ( 0.000000000000000000, 0.000000000000000000, 1.000000000000000000 ) ) ;
#32994 = DIRECTION ( 'NONE',  ( 1.000000000000000000, -0.000000000000000000, 0.000000000000000000 ) ) ;
#32995 = VERTEX_POINT ( 'NONE', #22942 ) ;
#32996 = DIRECTION ( 'NONE',  ( -1.000000000000000000, -0.000000000000000000, -0.000000000000000000 ) ) ;
#32997 = CIRCLE ( 'NONE', #11450, 12.59999999999999964 ) ;
#32998 = FACE_BOUND ( 'NONE', #21525, .T. ) ;
#32999 = ORIENTED_EDGE ( 'NONE', *, *, #1749, .F. ) ;
#33000 = PLANE ( 'NONE',  #11775 ) ;
#33001 = ORIENTED_EDGE ( 'NONE', *, *, #37137, .T. ) ;
#33002 = CYLINDRICAL_SURFACE ( 'NONE', #11441, 59.00000000000000000 ) ;
#33003 = VECTOR ( 'NONE', #16624, 1000.000000000000000 ) ;
#33004 = ORIENTED_EDGE ( 'NONE', *, *, #2717, .T. ) ;
#33006 = EDGE_LOOP ( 'NONE', ( #40383, #38488 ) ) ;
#33005 = CARTESIAN_POINT ( 'NONE',  ( 17.99999999999999645, 97.89532456239497549, 54.81585448086229917 ) ) ;
#33007 = CARTESIAN_POINT ( 'NONE',  ( -30.31917247938466176, 31.00000000000000355, 52.30862930534038924 ) ) ;
#33008 = ORIENTED_EDGE ( 'NONE', *, *, #31932, .F. ) ;
#33009 = CYLINDRICAL_SURFACE ( 'NONE', #27247, 10.99999999999998934 ) ;
#33010 = EDGE_CURVE ( 'NONE', #42002, #40772, #5284, .T. ) ;
#33011 = EDGE_CURVE ( 'NONE', #15772, #17775, #15103, .T. ) ;
#33012 = EDGE_CURVE ( 'NONE', #39874, #31256, #39430, .T. ) ;
#33013 = AXIS2_PLACEMENT_3D ( 'NONE', #20801, #34064, #871 ) ;
#33014 = ORIENTED_EDGE ( 'NONE', *, *, #14686, .F. ) ;
#33015 = CARTESIAN_POINT ( 'NONE',  ( 17.99999999999999645, -5.919241748379815427, 31.39643714728454427 ) ) ;
#33016 = EDGE_CURVE ( 'NONE', #17987, #11580, #42200, .T. ) ;
#33017 = EDGE_LOOP ( 'NONE', ( #34182, #7930, #34901, #39064 ) ) ;
#33018 = CARTESIAN_POINT ( 'NONE',  ( 84.58694138809387653, 39.99999999999999289, 22.77597867319729374 ) ) ;
#33020 = CARTESIAN_POINT ( 'NONE',  ( 0.000000000000000000, -29.60891106212762125, -37.14118181634796656 ) ) ;
#33019 = CARTESIAN_POINT ( 'NONE',  ( 0.000000000000000000, 51.27532863109503580, -99.79535634195073612 ) ) ;
#33021 = CYLINDRICAL_SURFACE ( 'NONE', #15740, 59.00000000000001421 ) ;
#33022 = ORIENTED_EDGE ( 'NONE', *, *, #23504, .T. ) ;
#33023 = DIRECTION ( 'NONE',  ( 0.000000000000000000, 0.1590634960190655256, 0.9872683547213456645 ) ) ;
#33024 = VECTOR ( 'NONE', #15940, 1000.000000000000000 ) ;
#33025 = ORIENTED_EDGE ( 'NONE', *, *, #20230, .F. ) ;
#33026 = CIRCLE ( 'NONE', #41399, 36.00000000000000000 ) ;
#33027 = DIRECTION ( 'NONE',  ( -1.000000000000000000, -0.000000000000000000, -0.000000000000000000 ) ) ;
#33028 = DIRECTION ( 'NONE',  ( -1.000000000000000000, 1.373900992973641868E-15, 4.405646923115722869E-16 ) ) ;
#33029 = EDGE_CURVE ( 'NONE', #34279, #37209, #12965, .T. ) ;
#33030 = CARTESIAN_POINT ( 'NONE',  ( 68.07048008643859305, 31.00000000000000000, 33.55317283102968418 ) ) ;
#33032 = DIRECTION ( 'NONE',  ( 1.000000000000000000, -0.000000000000000000, -0.000000000000000000 ) ) ;
#33031 = DIRECTION ( 'NONE',  ( -1.000000000000000000, -0.000000000000000000, -0.000000000000000000 ) ) ;
#33033 = VERTEX_POINT ( 'NONE', #11110 ) ;
#33034 = VECTOR ( 'NONE', #22673, 1000.000000000000000 ) ;
#33035 = DIRECTION ( 'NONE',  ( -1.836909530733573776E-16, 1.000000000000000000, 0.000000000000000000 ) ) ;
#33036 = AXIS2_PLACEMENT_3D ( 'NONE', #32419, #5794, #38524 ) ;
#33037 = ORIENTED_EDGE ( 'NONE', *, *, #18394, .F. ) ;
#33038 = CARTESIAN_POINT ( 'NONE',  ( 0.000000000000000000, -31.80866420683992857, 2.997093558041182160 ) ) ;
#33039 = CYLINDRICAL_SURFACE ( 'NONE', #39432, 13.60000000000000142 ) ;
#33040 = CARTESIAN_POINT ( 'NONE',  ( 72.29027477042623673, 31.00000000000000000, -63.25088587033864229 ) ) ;
#33041 = CARTESIAN_POINT ( 'NONE',  ( 18.00000000000000355, 0.000000000000000000, 0.000000000000000000 ) ) ;
#33042 = EDGE_CURVE ( 'NONE', #27124, #6594, #8086, .T. ) ;
#33043 = CARTESIAN_POINT ( 'NONE',  ( 18.00000000000000355, -38.92705108641711576, -27.21837053747839263 ) ) ;
#33044 = EDGE_LOOP ( 'NONE', ( #31473, #1527, #40406, #30949 ) ) ;
#33045 = CARTESIAN_POINT ( 'NONE',  ( 42.80287614962790599, -14.05525454449571932, 69.29271901957253021 ) ) ;
#33046 = ORIENTED_EDGE ( 'NONE', *, *, #21055, .F. ) ;
#33047 = CIRCLE ( 'NONE', #14267, 116.0000000000000000 ) ;
#33048 = DIRECTION ( 'NONE',  ( -1.000000000000000000, -0.000000000000000000, -0.000000000000000000 ) ) ;
#33049 = FACE_OUTER_BOUND ( 'NONE', #38404, .T. ) ;
#33050 = DIRECTION ( 'NONE',  ( -1.000000000000000000, 0.000000000000000000, -0.000000000000000000 ) ) ;
#33051 = VERTEX_POINT ( 'NONE', #27460 ) ;
#33052 = DIRECTION ( 'NONE',  ( -3.996523416598930318E-16, 2.658563593772947863E-15, 1.000000000000000000 ) ) ;
#33053 = CIRCLE ( 'NONE', #13593, 58.99999999999999289 ) ;
#33054 = DIRECTION ( 'NONE',  ( -1.000000000000000000, -0.000000000000000000, -0.000000000000000000 ) ) ;
#33055 = VECTOR ( 'NONE', #10887, 1000.000000000000000 ) ;
#33056 = DIRECTION ( 'NONE',  ( 1.000000000000000000, 0.000000000000000000, 0.000000000000000000 ) ) ;
#33057 = AXIS2_PLACEMENT_3D ( 'NONE', #42380, #12099, #25420 ) ;
#33059 = ORIENTED_EDGE ( 'NONE', *, *, #41352, .F. ) ;
#33058 = DIRECTION ( 'NONE',  ( 0.000000000000000000, 0.000000000000000000, 1.000000000000000000 ) ) ;
#33060 = EDGE_CURVE ( 'NONE', #27794, #34636, #7596, .T. ) ;
#33061 = CARTESIAN_POINT ( 'NONE',  ( 36.20216622922067273, 31.00000000000000355, 9.761693653842600682 ) ) ;
#33062 = CYLINDRICAL_SURFACE ( 'NONE', #9256, 19.99999999999999645 ) ;
#33063 = CIRCLE ( 'NONE', #24073, 59.00000000000000711 ) ;
#33064 = EDGE_CURVE ( 'NONE', #14258, #25432, #10877, .T. ) ;
#33066 = ORIENTED_EDGE ( 'NONE', *, *, #16747, .T. ) ;
#33065 = DIRECTION ( 'NONE',  ( -1.000000000000000000, -0.000000000000000000, -0.000000000000000000 ) ) ;
#33067 = CIRCLE ( 'NONE', #13602, 58.99999999999999289 ) ;
#33068 = ORIENTED_EDGE ( 'NONE', *, *, #15831, .F. ) ;
#33069 = CARTESIAN_POINT ( 'NONE',  ( 0.000000000000000000, 46.11014828289844303, -9.022736828080878624 ) ) ;
#33070 = CARTESIAN_POINT ( 'NONE',  ( 6.600000000000004974, -19.99999999999998579, 2.449293598294705724E-15 ) ) ;
#33071 = CARTESIAN_POINT ( 'NONE',  ( -51.89982240185989326, 40.00000000000000000, 3.308651922604956219 ) ) ;
#33072 = DIRECTION ( 'NONE',  ( 0.000000000000000000, 0.000000000000000000, 1.000000000000000000 ) ) ;
#33073 = DIRECTION ( 'NONE',  ( -1.000000000000000000, 0.000000000000000000, 0.000000000000000000 ) ) ;
#33074 = DIRECTION ( 'NONE',  ( 0.000000000000000000, 0.000000000000000000, 1.000000000000000000 ) ) ;
#33075 = VERTEX_POINT ( 'NONE', #3865 ) ;
#33076 = DIRECTION ( 'NONE',  ( -0.5000000000000051070, 0.000000000000000000, 0.8660254037844355990 ) ) ;
#33077 = ADVANCED_FACE ( 'NONE', ( #37261 ), #17247, .F. ) ;
#33078 = AXIS2_PLACEMENT_3D ( 'NONE', #38449, #8569, #21928 ) ;
#33079 = ORIENTED_EDGE ( 'NONE', *, *, #9372, .F. ) ;
#33080 = DIRECTION ( 'NONE',  ( -1.000000000000000000, -0.000000000000000000, -0.000000000000000000 ) ) ;
#33081 = DIRECTION ( 'NONE',  ( 0.000000000000000000, 0.000000000000000000, 1.000000000000000000 ) ) ;
#33082 = ADVANCED_FACE ( 'NONE', ( #20736 ), #3163, .T. ) ;
#33083 = CARTESIAN_POINT ( 'NONE',  ( -36.80126402429788612, 31.00000000000000355, 32.28896105221774349 ) ) ;
#33084 = CYLINDRICAL_SURFACE ( 'NONE', #42013, 116.0000000000000000 ) ;
#33085 = ORIENTED_EDGE ( 'NONE', *, *, #42527, .F. ) ;
#33086 = CIRCLE ( 'NONE', #38655, 142.5000000000000284 ) ;
#33087 = EDGE_CURVE ( 'NONE', #38633, #19127, #24647, .T. ) ;
#33088 = VECTOR ( 'NONE', #34958, 1000.000000000000000 ) ;
#33089 = DIRECTION ( 'NONE',  ( 1.000000000000000000, 0.000000000000000000, 0.000000000000000000 ) ) ;
#33090 = ORIENTED_EDGE ( 'NONE', *, *, #956, .F. ) ;
#33091 = CARTESIAN_POINT ( 'NONE',  ( 92.36625196220676060, 31.00000000000000000, 24.73319171124347093 ) ) ;
#33092 = AXIS2_PLACEMENT_3D ( 'NONE', #9975, #19837, #23323 ) ;
#33093 = DIRECTION ( 'NONE',  ( -0.2140725878556641593, -0.9768177553304296934, 0.000000000000000000 ) ) ;
#33094 = VERTEX_POINT ( 'NONE', #24220 ) ;
#33095 = CARTESIAN_POINT ( 'NONE',  ( 4.329677741076777053, 31.00000000000000355, -64.59417075179258916 ) ) ;
#33097 = AXIS2_PLACEMENT_3D ( 'NONE', #12144, #5576, #32195 ) ;
#33096 = CARTESIAN_POINT ( 'NONE',  ( 43.45541166192411708, 40.00000000000000000, -49.38773770141698805 ) ) ;
#33098 = CARTESIAN_POINT ( 'NONE',  ( 48.45023387855729879, 40.00000000000000000, 83.88660019351674180 ) ) ;
#33099 = AXIS2_PLACEMENT_3D ( 'NONE', #29758, #10321, #29536 ) ;
#33100 = ORIENTED_EDGE ( 'NONE', *, *, #23365, .F. ) ;
#33101 = ORIENTED_EDGE ( 'NONE', *, *, #31376, .F. ) ;
#33102 = SURFACE_STYLE_USAGE ( .BOTH. , #35717 ) ;
#33103 = DIRECTION ( 'NONE',  ( 0.000000000000000000, 0.000000000000000000, 1.000000000000000000 ) ) ;
#33104 = FACE_OUTER_BOUND ( 'NONE', #5688, .T. ) ;
#33106 = ORIENTED_EDGE ( 'NONE', *, *, #33439, .F. ) ;
#33105 = CARTESIAN_POINT ( 'NONE',  ( 17.99999999999999645, -21.48775762007842260, -23.64423737150161031 ) ) ;
#33107 = CARTESIAN_POINT ( 'NONE',  ( 17.99999999999999645, 0.000000000000000000, 0.000000000000000000 ) ) ;
#33108 = ORIENTED_EDGE ( 'NONE', *, *, #26730, .F. ) ;
#33109 = CYLINDRICAL_SURFACE ( 'NONE', #36970, 51.99999999999999289 ) ;
#33110 = CARTESIAN_POINT ( 'NONE',  ( -31.81163009274181519, 40.00000000000000000, -64.50738158386226928 ) ) ;
#33111 = DIRECTION ( 'NONE',  ( -1.000000000000000000, -0.000000000000000000, 0.000000000000000000 ) ) ;
#33112 = AXIS2_PLACEMENT_3D ( 'NONE', #36029, #6155, #19500 ) ;
#33113 = VERTEX_POINT ( 'NONE', #30737 ) ;
#33114 = DIRECTION ( 'NONE',  ( 0.000000000000000000, 0.000000000000000000, 1.000000000000000000 ) ) ;
#33115 = DIRECTION ( 'NONE',  ( 0.000000000000000000, 0.9714298932647090767, 0.2373266998711184850 ) ) ;
#33116 = CIRCLE ( 'NONE', #12247, 142.5000000000000284 ) ;
#33117 = AXIS2_PLACEMENT_3D ( 'NONE', #17301, #14001, #30354 ) ;
#33118 = EDGE_CURVE ( 'NONE', #31429, #32974, #28368, .T. ) ;
#33119 = ORIENTED_EDGE ( 'NONE', *, *, #19171, .F. ) ;
#33120 = VECTOR ( 'NONE', #37314, 1000.000000000000000 ) ;
#33121 = EDGE_CURVE ( 'NONE', #17019, #28172, #38753, .T. ) ;
#33122 = AXIS2_PLACEMENT_3D ( 'NONE', #24295, #20577, #33850 ) ;
#33123 = ORIENTED_EDGE ( 'NONE', *, *, #14303, .T. ) ;
#33124 = FACE_BOUND ( 'NONE', #23311, .T. ) ;
#33125 = ORIENTED_EDGE ( 'NONE', *, *, #5374, .F. ) ;
#33126 = DIRECTION ( 'NONE',  ( -0.5000000000000019984, -0.8660254037844375974, 0.000000000000000000 ) ) ;
#33127 = COLOUR_RGB ( '', 0.66274510, 0.83137255, 0.94901961) ;
#33128 = LINE ( 'NONE', #6293, #37936 ) ;
#33129 = CARTESIAN_POINT ( 'NONE',  ( -91.96080130434580724, -40.05525454449572464, 14.45886780445738218 ) ) ;
#33130 = AXIS2_PLACEMENT_3D ( 'NONE', #10170, #32448, #16545 ) ;
#33131 = AXIS2_PLACEMENT_3D ( 'NONE', #11132, #24458, #21418 ) ;
#33132 = CARTESIAN_POINT ( 'NONE',  ( -150.5000000000000284, -5.254679414958916394E-13, 6.999999999999998224 ) ) ;
#33133 = DIRECTION ( 'NONE',  ( 0.000000000000000000, -0.9574220383620080099, 0.2886919473396124536 ) ) ;
#33134 = ORIENTED_EDGE ( 'NONE', *, *, #10225, .T. ) ;
#33135 = CYLINDRICAL_SURFACE ( 'NONE', #32810, 10.99999999999999645 ) ;
#33136 = ADVANCED_FACE ( 'NONE', ( #37691 ), #7810, .T. ) ;
#33138 = ORIENTED_EDGE ( 'NONE', *, *, #9224, .T. ) ;
#33137 = AXIS2_PLACEMENT_3D ( 'NONE', #26905, #19736, #33647 ) ;
#33139 = DIRECTION ( 'NONE',  ( 1.000000000000000000, 0.000000000000000000, 0.000000000000000000 ) ) ;
#33140 = EDGE_CURVE ( 'NONE', #11159, #1957, #7154, .T. ) ;
#33141 = CARTESIAN_POINT ( 'NONE',  ( 2.965790448435745574, 31.00000000000000355, -22.56328348808469997 ) ) ;
#33142 = ORIENTED_EDGE ( 'NONE', *, *, #24227, .F. ) ;
#33143 = DIRECTION ( 'NONE',  ( -1.000000000000000000, 0.000000000000000000, -0.000000000000000000 ) ) ;
#33144 = EDGE_CURVE ( 'NONE', #26640, #18784, #13720, .T. ) ;
#33145 = CARTESIAN_POINT ( 'NONE',  ( 0.000000000000000000, 0.7408941433508176022, -1.199999999999999956 ) ) ;
#33146 = APPLICATION_PROTOCOL_DEFINITION ( 'draft international standard', 'automotive_design', 1998, #5251 ) ;
#33147 = DIRECTION ( 'NONE',  ( 1.000000000000000000, 0.000000000000000000, 0.000000000000000000 ) ) ;
#33148 = CARTESIAN_POINT ( 'NONE',  ( 44.56294422764113250, 31.00000000000000355, 34.17917587534974189 ) ) ;
#33150 = EDGE_LOOP ( 'NONE', ( #31934, #6290, #28598, #41268 ) ) ;
#33149 = AXIS2_PLACEMENT_3D ( 'NONE', #29780, #48, #36290 ) ;
#33151 = CARTESIAN_POINT ( 'NONE',  ( 23.40755275317545880, 31.00000000000000355, 30.61714766194360138 ) ) ;
#33152 = CIRCLE ( 'NONE', #14368, 64.99999999999997158 ) ;
#33153 = CARTESIAN_POINT ( 'NONE',  ( -18.69663849766352826, 40.00000000000000000, -69.77653669617104981 ) ) ;
#33154 = VECTOR ( 'NONE', #39449, 1000.000000000000000 ) ;
#33155 = VECTOR ( 'NONE', #15003, 1000.000000000000000 ) ;
#33156 = EDGE_CURVE ( 'NONE', #35643, #13412, #6028, .T. ) ;
#33157 = DIRECTION ( 'NONE',  ( 0.000000000000000000, 0.000000000000000000, 1.000000000000000000 ) ) ;
#33158 = EDGE_CURVE ( 'NONE', #14447, #4027, #37049, .T. ) ;
#33159 = VECTOR ( 'NONE', #4784, 1000.000000000000000 ) ;
#33160 = AXIS2_PLACEMENT_3D ( 'NONE', #7435, #41013, #20797 ) ;
#33161 = CARTESIAN_POINT ( 'NONE',  ( -107.9608013043457930, -12.05525454449571043, 14.45886780445738395 ) ) ;
#33162 = CARTESIAN_POINT ( 'NONE',  ( 18.00000000000000355, 0.000000000000000000, 0.000000000000000000 ) ) ;
#33163 = AXIS2_PLACEMENT_3D ( 'NONE', #22697, #6077, #15136 ) ;
#33164 = VERTEX_POINT ( 'NONE', #1904 ) ;
#33165 = CARTESIAN_POINT ( 'NONE',  ( 43.96541952717798551, 40.00000000000000000, 11.76906328551413239 ) ) ;
#33166 = LINE ( 'NONE', #29922, #23692 ) ;
#33167 = DIRECTION ( 'NONE',  ( -1.000000000000000000, 0.000000000000000000, -0.000000000000000000 ) ) ;
#33168 = EDGE_LOOP ( 'NONE', ( #15641, #24759, #30611, #12579 ) ) ;
#33169 = CARTESIAN_POINT ( 'NONE',  ( 17.99999999999999645, 101.1249659627855806, -48.60055280209454054 ) ) ;
#33170 = CARTESIAN_POINT ( 'NONE',  ( 17.99999999999999645, 0.6819280456829140968, 115.9979955608738749 ) ) ;
#33171 = ORIENTED_EDGE ( 'NONE', *, *, #26290, .T. ) ;
#33172 = PLANE ( 'NONE',  #17261 ) ;
#33173 = ORIENTED_EDGE ( 'NONE', *, *, #14321, .F. ) ;
#33174 = ADVANCED_FACE ( 'NONE', ( #12183 ), #25506, .T. ) ;
#33175 = VERTEX_POINT ( 'NONE', #1686 ) ;
#33176 = DIRECTION ( 'NONE',  ( -1.000000000000000000, -0.000000000000000000, -0.000000000000000000 ) ) ;
#33177 = CARTESIAN_POINT ( 'NONE',  ( 11.57239447661056353, 31.00000000000000355, 88.72710294830137912 ) ) ;
#33178 = ORIENTED_EDGE ( 'NONE', *, *, #22818, .F. ) ;
#33179 = CARTESIAN_POINT ( 'NONE',  ( 5.200000000000002842, 0.000000000000000000, 0.000000000000000000 ) ) ;
#33180 = AXIS2_PLACEMENT_3D ( 'NONE', #21282, #31496, #28664 ) ;
#33181 = CARTESIAN_POINT ( 'NONE',  ( 18.00000000000000355, 41.20225022064669673, -23.63323037071358357 ) ) ;
#33182 = CIRCLE ( 'NONE', #17919, 20.00000000000000355 ) ;
#33183 = EDGE_CURVE ( 'NONE', #9004, #5428, #38130, .T. ) ;
#33185 = CYLINDRICAL_SURFACE ( 'NONE', #21345, 59.00000000000000000 ) ;
#33184 = CIRCLE ( 'NONE', #9521, 120.5010000000000474 ) ;
#33186 = ORIENTED_EDGE ( 'NONE', *, *, #25334, .T. ) ;
#33187 = AXIS2_PLACEMENT_3D ( 'NONE', #25687, #5783, #38945 ) ;
#33188 = FACE_OUTER_BOUND ( 'NONE', #20180, .T. ) ;
#33189 = EDGE_CURVE ( 'NONE', #37254, #26682, #25299, .T. ) ;
#33190 = CIRCLE ( 'NONE', #16496, 116.0000000000000000 ) ;
#33191 = CARTESIAN_POINT ( 'NONE',  ( 0.000000000000000000, 0.000000000000000000, 0.000000000000000000 ) ) ;
#33192 = CIRCLE ( 'NONE', #40840, 22.99999999999987921 ) ;
#33193 = ADVANCED_FACE ( 'NONE', ( #15673 ), #12401, .F. ) ;
#33195 = DIRECTION ( 'NONE',  ( 0.000000000000000000, 0.000000000000000000, 1.000000000000000000 ) ) ;
#33194 = CARTESIAN_POINT ( 'NONE',  ( 17.99999999999999645, 0.000000000000000000, 0.000000000000000000 ) ) ;
#33196 = CIRCLE ( 'NONE', #3206, 116.0000000000000000 ) ;
#33197 = EDGE_CURVE ( 'NONE', #10324, #41990, #30432, .T. ) ;
#33198 = CARTESIAN_POINT ( 'NONE',  ( 0.000000000000000000, 0.000000000000000000, 0.000000000000000000 ) ) ;
#33199 = ORIENTED_EDGE ( 'NONE', *, *, #16565, .F. ) ;
#33200 = CIRCLE ( 'NONE', #2497, 58.99999999999999289 ) ;
#33201 = CARTESIAN_POINT ( 'NONE',  ( -20.72449291656876369, 31.00000000000000355, -23.61699481730619610 ) ) ;
#33202 = ORIENTED_EDGE ( 'NONE', *, *, #12637, .F. ) ;
#33203 = CARTESIAN_POINT ( 'NONE',  ( 0.000000000000000000, -101.1403355683150096, 56.80345518653453496 ) ) ;
#33204 = CARTESIAN_POINT ( 'NONE',  ( -2.000000000000007550, -3.464101615137749945, 0.000000000000000000 ) ) ;
#33205 = ORIENTED_EDGE ( 'NONE', *, *, #41138, .T. ) ;
#33206 = CARTESIAN_POINT ( 'NONE',  ( 2.500000000000000000, 2.357898499370431722, -2.818925648462311528E-15 ) ) ;
#33207 = CARTESIAN_POINT ( 'NONE',  ( 28.83751338862256119, 40.00000000000000000, -32.88701605462710376 ) ) ;
#33208 = CARTESIAN_POINT ( 'NONE',  ( -33.53193138075045709, 40.00000000000000000, 38.09769221459629307 ) ) ;
#33209 = VERTEX_POINT ( 'NONE', #31819 ) ;
#33210 = ORIENTED_EDGE ( 'NONE', *, *, #42606, .T. ) ;
#33211 = FACE_OUTER_BOUND ( 'NONE', #1356, .T. ) ;
#33212 = CARTESIAN_POINT ( 'NONE',  ( -10.00000000000000000, 0.000000000000000000, 0.000000000000000000 ) ) ;
#33213 = EDGE_CURVE ( 'NONE', #8627, #2881, #28563, .T. ) ;
#33214 = CIRCLE ( 'NONE', #18640, 58.99999999999999289 ) ;
#33215 = EDGE_CURVE ( 'NONE', #14276, #38773, #26255, .T. ) ;
#33216 = ADVANCED_FACE ( 'NONE', ( #38544 ), #32230, .F. ) ;
#33217 = LINE ( 'NONE', #14188, #23353 ) ;
#33218 = CARTESIAN_POINT ( 'NONE',  ( -10.00000000000000000, 0.000000000000000000, 0.000000000000000000 ) ) ;
#33219 = CIRCLE ( 'NONE', #6061, 59.00000000000000711 ) ;
#33220 = CARTESIAN_POINT ( 'NONE',  ( 17.99999999999999645, 22.66088087769180603, 21.87856208362564914 ) ) ;
#33221 = VERTEX_POINT ( 'NONE', #11769 ) ;
#33222 = CARTESIAN_POINT ( 'NONE',  ( 18.00000000000000355, 0.000000000000000000, 0.000000000000000000 ) ) ;
#33223 = EDGE_LOOP ( 'NONE', ( #42598, #24814, #18165, #39210, #23507 ) ) ;
#33224 = CARTESIAN_POINT ( 'NONE',  ( 0.000000000000000000, 58.30069736313667050, 100.2847380560568951 ) ) ;
#33225 = CARTESIAN_POINT ( 'NONE',  ( 0.3198814748697593746, 4.434118497892183264, -0.3507732604232499107 ) ) ;
#33226 = VECTOR ( 'NONE', #1001, 1000.000000000000000 ) ;
#33227 = ORIENTED_EDGE ( 'NONE', *, *, #8374, .F. ) ;
#33228 =( GEOMETRIC_REPRESENTATION_CONTEXT ( 3 ) GLOBAL_UNCERTAINTY_ASSIGNED_CONTEXT ( ( #309 ) ) GLOBAL_UNIT_ASSIGNED_CONTEXT ( ( #5379, #4731, #21996 ) ) REPRESENTATION_CONTEXT ( 'NONE', 'WORKASPACE' ) );
#33229 = CARTESIAN_POINT ( 'NONE',  ( 17.99999999999999645, 112.1427988504408404, -3.502162136922268409 ) ) ;
#33230 = DIRECTION ( 'NONE',  ( 0.000000000000000000, 0.000000000000000000, 1.000000000000000000 ) ) ;
#33231 = VERTEX_POINT ( 'NONE', #41384 ) ;
#33232 = DIRECTION ( 'NONE',  ( 0.000000000000000000, 0.000000000000000000, 1.000000000000000000 ) ) ;
#33233 = ORIENTED_EDGE ( 'NONE', *, *, #7623, .F. ) ;
#33234 = LINE ( 'NONE', #13189, #19796 ) ;
#33235 = AXIS2_PLACEMENT_3D ( 'NONE', #19860, #42710, #36833 ) ;
#33236 = EDGE_LOOP ( 'NONE', ( #765, #8762, #35022, #5753 ) ) ;
#33238 = EDGE_LOOP ( 'NONE', ( #26045, #17889, #786, #25302 ) ) ;
#33237 = LINE ( 'NONE', #27142, #27855 ) ;
#33239 = AXIS2_PLACEMENT_3D ( 'NONE', #31758, #1852, #9896 ) ;
#33240 = CARTESIAN_POINT ( 'NONE',  ( -53.12901929300349479, 31.00000000000000355, 30.56653509229933618 ) ) ;
#33241 = ORIENTED_EDGE ( 'NONE', *, *, #12641, .T. ) ;
#33242 = DIRECTION ( 'NONE',  ( -1.000000000000000000, -0.000000000000000000, 0.000000000000000000 ) ) ;
#33243 = ORIENTED_EDGE ( 'NONE', *, *, #16393, .T. ) ;
#33244 = DIRECTION ( 'NONE',  ( 0.000000000000000000, 0.000000000000000000, 1.000000000000000000 ) ) ;
#33245 = PRODUCT ( 'Planetary Gear Carrier Assembly', 'Planetary Gear Carrier Assembly', '', ( #22722 ) ) ;
#33246 = EDGE_CURVE ( 'NONE', #9615, #40347, #27635, .T. ) ;
#33247 = VERTEX_POINT ( 'NONE', #35493 ) ;
#33248 = CARTESIAN_POINT ( 'NONE',  ( -78.26717753304431824, 40.00000000000000711, -26.69481836930730978 ) ) ;
#33249 = ADVANCED_FACE ( 'NONE', ( #9095 ), #7429, .T. ) ;
#33251 = DIRECTION ( 'NONE',  ( 0.000000000000000000, 0.000000000000000000, -1.000000000000000000 ) ) ;
#33250 = CARTESIAN_POINT ( 'NONE',  ( -3.413765605486552168, -14.29811891091961407, 0.000000000000000000 ) ) ;
#33252 = DIRECTION ( 'NONE',  ( -1.000000000000000000, -0.000000000000000000, 0.000000000000000000 ) ) ;
#33253 = ORIENTED_EDGE ( 'NONE', *, *, #24111, .T. ) ;
#33254 = CARTESIAN_POINT ( 'NONE',  ( 18.00000000000000355, 30.93515269692114344, 36.04401931830261674 ) ) ;
#33255 = VECTOR ( 'NONE', #29263, 1000.000000000000000 ) ;
#33256 = ORIENTED_EDGE ( 'NONE', *, *, #5044, .T. ) ;
#33257 = VECTOR ( 'NONE', #19053, 1000.000000000000000 ) ;
#33258 = DIRECTION ( 'NONE',  ( 0.000000000000000000, 0.000000000000000000, 1.000000000000000000 ) ) ;
#33259 = CIRCLE ( 'NONE', #4696, 13.60000000000000142 ) ;
#33260 = CARTESIAN_POINT ( 'NONE',  ( 36.74538074116732389, 31.00000000000000355, -63.64477163140654170 ) ) ;
#33262 = DIRECTION ( 'NONE',  ( 0.000000000000000000, 0.000000000000000000, 1.000000000000000000 ) ) ;
#33261 = DIRECTION ( 'NONE',  ( 0.000000000000000000, 0.000000000000000000, 1.000000000000000000 ) ) ;
#33264 = VERTEX_POINT ( 'NONE', #42247 ) ;
#33263 = AXIS2_PLACEMENT_3D ( 'NONE', #26735, #30023, #20881 ) ;
#33265 = AXIS2_PLACEMENT_3D ( 'NONE', #34278, #14231, #24509 ) ;
#33266 = CARTESIAN_POINT ( 'NONE',  ( 22.90854556226710415, -40.05525454449572464, -74.83297477053821467 ) ) ;
#33267 = EDGE_CURVE ( 'NONE', #31975, #2667, #35974, .T. ) ;
#33268 = VERTEX_POINT ( 'NONE', #25096 ) ;
#33269 = DIRECTION ( 'NONE',  ( 1.000000000000000000, 0.000000000000000000, 0.000000000000000000 ) ) ;
#33270 = CARTESIAN_POINT ( 'NONE',  ( 17.99999999999999645, 110.0562500189205224, -49.07252625220001363 ) ) ;
#33271 = EDGE_CURVE ( 'NONE', #15863, #18333, #15471, .T. ) ;
#33272 = CARTESIAN_POINT ( 'NONE',  ( -80.34276469477588023, 31.00000000000000711, 61.48650092630385444 ) ) ;
#33273 = ADVANCED_FACE ( 'NONE', ( #18975 ), #28769, .F. ) ;
#33274 = EDGE_CURVE ( 'NONE', #26169, #34763, #22793, .T. ) ;
#33275 = FACE_OUTER_BOUND ( 'NONE', #317, .T. ) ;
#33276 = ORIENTED_EDGE ( 'NONE', *, *, #34982, .F. ) ;
#33277 = LINE ( 'NONE', #26733, #28467 ) ;
#33278 = ORIENTED_EDGE ( 'NONE', *, *, #10348, .T. ) ;
#33279 = CARTESIAN_POINT ( 'NONE',  ( 9.000000000000001776, 40.47821179127714686, 32.64221760512772619 ) ) ;
#33280 = AXIS2_PLACEMENT_3D ( 'NONE', #24, #7239, #236 ) ;
#33281 = CARTESIAN_POINT ( 'NONE',  ( 0.000000000000000000, -24.70533337038204635, -26.18485254986720179 ) ) ;
#33282 = EDGE_CURVE ( 'NONE', #29453, #821, #33184, .T. ) ;
#33283 = DIRECTION ( 'NONE',  ( 3.009274222672345096E-17, 1.000000000000000000, -2.455023325076454960E-18 ) ) ;
#33284 = ORIENTED_EDGE ( 'NONE', *, *, #36643, .T. ) ;
#33285 = ORIENTED_EDGE ( 'NONE', *, *, #13054, .F. ) ;
#33286 = LINE ( 'NONE', #9726, #30057 ) ;
#33287 = AXIS2_PLACEMENT_3D ( 'NONE', #37713, #27939, #837 ) ;
#33288 = CARTESIAN_POINT ( 'NONE',  ( 12.50000000000000000, 0.000000000000000000, -20.00000000000000000 ) ) ;
#33289 = DIRECTION ( 'NONE',  ( 0.000000000000000000, -1.000000000000000000, 0.000000000000000000 ) ) ;
#33290 = AXIS2_PLACEMENT_3D ( 'NONE', #21945, #28688, #21739 ) ;
#33292 = ORIENTED_EDGE ( 'NONE', *, *, #12084, .F. ) ;
#33291 = DIRECTION ( 'NONE',  ( 0.000000000000000000, -0.8993121301712143634, -0.4373073204588656115 ) ) ;
#33293 = CARTESIAN_POINT ( 'NONE',  ( 9.304442065603227618, 31.00000000000000355, 27.50946418541002458 ) ) ;
#33294 = CARTESIAN_POINT ( 'NONE',  ( 0.000000000000000000, 23.10276247328255650, -118.2656051737067600 ) ) ;
#33295 = AXIS2_PLACEMENT_3D ( 'NONE', #41257, #18414, #14691 ) ;
#33297 = ORIENTED_EDGE ( 'NONE', *, *, #19349, .F. ) ;
#33296 = DIRECTION ( 'NONE',  ( 0.000000000000000000, 0.6382441836448160544, 0.7698339834299096074 ) ) ;
#33298 = ORIENTED_EDGE ( 'NONE', *, *, #11977, .F. ) ;
#33299 = DIRECTION ( 'NONE',  ( 0.000000000000000000, 0.000000000000000000, 1.000000000000000000 ) ) ;
#33300 = DIRECTION ( 'NONE',  ( 3.996523416598930318E-16, -2.658563593772947863E-15, -1.000000000000000000 ) ) ;
#33301 = CARTESIAN_POINT ( 'NONE',  ( 56.89991739620084843, 40.00000000000000000, -3.630084216720919521 ) ) ;
#33302 = DIRECTION ( 'NONE',  ( 0.000000000000000000, 0.000000000000000000, -1.000000000000000000 ) ) ;
#33303 = DIRECTION ( 'NONE',  ( 0.000000000000000000, 1.000000000000000000, 0.000000000000000000 ) ) ;
#33304 = CARTESIAN_POINT ( 'NONE',  ( 8.999999999999998224, -74.56001736500675747, 88.86396238369010803 ) ) ;
#33305 = VERTEX_POINT ( 'NONE', #36132 ) ;
#33306 = DIRECTION ( 'NONE',  ( 1.000000000000000000, 0.000000000000000000, 0.000000000000000000 ) ) ;
#33307 = ORIENTED_EDGE ( 'NONE', *, *, #2354, .T. ) ;
#33308 = CARTESIAN_POINT ( 'NONE',  ( -8.920000000000003482, 0.000000000000000000, 0.000000000000000000 ) ) ;
#33309 = FACE_OUTER_BOUND ( 'NONE', #40398, .T. ) ;
#33310 = CARTESIAN_POINT ( 'NONE',  ( -12.41726970680908515, 31.00000000000000355, 46.38546114896210071 ) ) ;
#33311 = AXIS2_PLACEMENT_3D ( 'NONE', #31680, #1124, #31474 ) ;
#33312 = CARTESIAN_POINT ( 'NONE',  ( -10.00000000000000000, 0.000000000000000000, 0.000000000000000000 ) ) ;
#33313 = ORIENTED_EDGE ( 'NONE', *, *, #2707, .F. ) ;
#33314 = CIRCLE ( 'NONE', #32630, 116.0000000000000000 ) ;
#33315 = CIRCLE ( 'NONE', #1266, 13.59999999999999964 ) ;
#33316 = CARTESIAN_POINT ( 'NONE',  ( 18.00000000000000355, -47.00885577955406802, -6.806061952192774989 ) ) ;
#33317 = VERTEX_POINT ( 'NONE', #26127 ) ;
#33318 = CARTESIAN_POINT ( 'NONE',  ( 83.17098260925966713, 31.00000000000000000, 48.02127090943169208 ) ) ;
#33319 = CIRCLE ( 'NONE', #14538, 120.5010000000000190 ) ;
#33320 = VECTOR ( 'NONE', #19306, 1000.000000000000000 ) ;
#33321 = VERTEX_POINT ( 'NONE', #6251 ) ;
#33322 = DIRECTION ( 'NONE',  ( 0.000000000000000000, 0.000000000000000000, 1.000000000000000000 ) ) ;
#33324 = CARTESIAN_POINT ( 'NONE',  ( 77.09314031436156256, 31.00000000000000000, 5.156213784760050878 ) ) ;
#33323 = AXIS2_PLACEMENT_3D ( 'NONE', #29478, #6332, #29063 ) ;
#33325 = CARTESIAN_POINT ( 'NONE',  ( 10.26812810425290579, 40.00000000000000000, 78.79123036454033979 ) ) ;
#33326 = EDGE_CURVE ( 'NONE', #25300, #25826, #6890, .T. ) ;
#33327 = EDGE_CURVE ( 'NONE', #1510, #2217, #38074, .T. ) ;
#33328 = DIRECTION ( 'NONE',  ( -1.000000000000000000, -0.000000000000000000, -0.000000000000000000 ) ) ;
#33329 = EDGE_CURVE ( 'NONE', #26923, #36284, #23094, .T. ) ;
#33330 = ORIENTED_EDGE ( 'NONE', *, *, #21702, .F. ) ;
#33331 = VERTEX_POINT ( 'NONE', #23515 ) ;
#33332 = DIRECTION ( 'NONE',  ( -1.000000000000000000, 0.000000000000000000, 0.000000000000000000 ) ) ;
#33333 = CARTESIAN_POINT ( 'NONE',  ( 17.99999999999999645, -84.77518783075045405, -73.49448960231443095 ) ) ;
#33334 = DIRECTION ( 'NONE',  ( 0.000000000000000000, 0.000000000000000000, 1.000000000000000000 ) ) ;
#33336 = VERTEX_POINT ( 'NONE', #16307 ) ;
#33335 = DIRECTION ( 'NONE',  ( 0.000000000000000000, 0.000000000000000000, -1.000000000000000000 ) ) ;
#33337 = DIRECTION ( 'NONE',  ( -1.000000000000000000, -0.000000000000000000, -0.000000000000000000 ) ) ;
#33338 = EDGE_LOOP ( 'NONE', ( #7853, #42503, #29933, #34955 ) ) ;
#33339 = CARTESIAN_POINT ( 'NONE',  ( 17.99999999999999645, 40.37724737310070111, 104.6802291180868565 ) ) ;
#33340 = ADVANCED_FACE ( 'NONE', ( #32867 ), #9947, .T. ) ;
#33341 = CARTESIAN_POINT ( 'NONE',  ( 52.74436945453300041, 40.00000000000000000, 68.73989242669851762 ) ) ;
#33342 = CARTESIAN_POINT ( 'NONE',  ( -7.000000000000002665, 18.77999999999999758, 0.000000000000000000 ) ) ;
#33343 = ORIENTED_EDGE ( 'NONE', *, *, #31055, .F. ) ;
#33344 = ADVANCED_FACE ( 'NONE', ( #20039 ), #40031, .F. ) ;
#33345 = DIRECTION ( 'NONE',  ( -0.000000000000000000, -0.000000000000000000, -1.000000000000000000 ) ) ;
#33346 = AXIS2_PLACEMENT_3D ( 'NONE', #34456, #37300, #27501 ) ;
#33347 = CARTESIAN_POINT ( 'NONE',  ( 0.000000000000000000, 41.62036691425530677, 113.0850832732715787 ) ) ;
#33348 = VECTOR ( 'NONE', #20078, 1000.000000000000000 ) ;
#33349 = ORIENTED_EDGE ( 'NONE', *, *, #5504, .F. ) ;
#33350 = ORIENTED_EDGE ( 'NONE', *, *, #32004, .F. ) ;
#33351 = PLANE ( 'NONE',  #26780 ) ;
#33352 = VERTEX_POINT ( 'NONE', #39394 ) ;
#33353 = CARTESIAN_POINT ( 'NONE',  ( 26.89767027507547326, 40.00000000000000000, -1.736414864505229305 ) ) ;
#33354 = CARTESIAN_POINT ( 'NONE',  ( 18.00000000000000355, -46.19362259308839214, 8.585149169758333088 ) ) ;
#33355 = CYLINDRICAL_SURFACE ( 'NONE', #33235, 20.00000000000000355 ) ;
#33356 = CARTESIAN_POINT ( 'NONE',  ( 17.99999999999999645, 3.996885678773026029, 120.4346956066682424 ) ) ;
#33357 = CARTESIAN_POINT ( 'NONE',  ( 0.000000000000000000, 97.89532456239568603, -54.81585448086097045 ) ) ;
#33358 = ORIENTED_EDGE ( 'NONE', *, *, #8265, .T. ) ;
#33359 = DIRECTION ( 'NONE',  ( 0.000000000000000000, 1.000000000000000000, 0.000000000000000000 ) ) ;
#33360 = EDGE_LOOP ( 'NONE', ( #20111, #24059, #15059, #15196, #21440 ) ) ;
#33361 = LINE ( 'NONE', #819, #32886 ) ;
#33362 = DIRECTION ( 'NONE',  ( 0.000000000000000000, -0.9510565162951565288, 0.3090169943749382919 ) ) ;
#33363 = EDGE_LOOP ( 'NONE', ( #21027, #7010, #38587, #32485 ) ) ;
#33364 = DIRECTION ( 'NONE',  ( 3.009274222672345096E-17, 1.000000000000000000, -2.455023325076455345E-18 ) ) ;
#33365 = DIRECTION ( 'NONE',  ( 0.000000000000000000, 0.7525707698561396874, -0.6585113790650372056 ) ) ;
#33366 = SHAPE_DEFINITION_REPRESENTATION ( #12683, #19391 ) ;
#33367 = DIRECTION ( 'NONE',  ( 1.000000000000000000, 0.000000000000000000, 0.000000000000000000 ) ) ;
#33368 = CARTESIAN_POINT ( 'NONE',  ( 58.80104710710317306, 31.00000000000000000, -45.11949705600698479 ) ) ;
#33369 = AXIS2_PLACEMENT_3D ( 'NONE', #19321, #26058, #26275 ) ;
#33370 = EDGE_LOOP ( 'NONE', ( #6610, #29557, #20084, #4278, #28044, #13833, #31714, #14023, #32374, #17502, #10684, #24200, #33626, #15420, #31179 ) ) ;
#33371 = CARTESIAN_POINT ( 'NONE',  ( 21.72498709342646706, 31.00000000000000355, -28.22316639787266013 ) ) ;
#33372 = EDGE_CURVE ( 'NONE', #5717, #17009, #24159, .T. ) ;
#33373 = CARTESIAN_POINT ( 'NONE',  ( 64.89583333437747115, 39.99999999999999289, -4.254240043327834009 ) ) ;
#33374 = CIRCLE ( 'NONE', #40332, 120.5010000000000190 ) ;
#33375 = DIRECTION ( 'NONE',  ( 0.000000000000000000, -0.9822872507286903865, 0.1873813145857150808 ) ) ;
#33376 = DIRECTION ( 'NONE',  ( -1.000000000000000000, -0.000000000000000000, -0.000000000000000000 ) ) ;
#33377 = EDGE_CURVE ( 'NONE', #10881, #42317, #10909, .T. ) ;
#33378 = ORIENTED_EDGE ( 'NONE', *, *, #28640, .F. ) ;
#33379 = FACE_OUTER_BOUND ( 'NONE', #24684, .T. ) ;
#33380 = LINE ( 'NONE', #7179, #35540 ) ;
#33381 = EDGE_CURVE ( 'NONE', #2582, #29580, #16493, .T. ) ;
#33382 = ORIENTED_EDGE ( 'NONE', *, *, #23463, .F. ) ;
#33383 = CARTESIAN_POINT ( 'NONE',  ( -33.94102792873697183, 40.00000000000000000, -38.68473105385043453 ) ) ;
#33384 = CARTESIAN_POINT ( 'NONE',  ( 2.500000000000000000, 2.357898499370431722, -2.818925648462311528E-15 ) ) ;
#33385 = CARTESIAN_POINT ( 'NONE',  ( 42.80287614962790599, -35.35525454449572180, 69.29271901957253021 ) ) ;
#33386 = ORIENTED_EDGE ( 'NONE', *, *, #6837, .F. ) ;
#33387 = EDGE_CURVE ( 'NONE', #29060, #24778, #14404, .T. ) ;
#33388 = DIRECTION ( 'NONE',  ( -0.000000000000000000, -0.000000000000000000, 1.000000000000000000 ) ) ;
#33389 = DIRECTION ( 'NONE',  ( -3.996523416598930318E-16, 2.658563593772947863E-15, 1.000000000000000000 ) ) ;
#33390 = ORIENTED_EDGE ( 'NONE', *, *, #9536, .F. ) ;
#33391 = DIRECTION ( 'NONE',  ( 1.000000000000000000, -0.000000000000000000, -0.000000000000000000 ) ) ;
#33392 = ORIENTED_EDGE ( 'NONE', *, *, #7080, .T. ) ;
#33393 = ORIENTED_EDGE ( 'NONE', *, *, #24596, .F. ) ;
#33394 = CARTESIAN_POINT ( 'NONE',  ( 8.999999999999998224, -64.69195966009822030, -96.28577441832322847 ) ) ;
#33395 = CARTESIAN_POINT ( 'NONE',  ( -29.11455967534192979, 31.00000000000000355, 85.38284731564058916 ) ) ;
#33396 = VERTEX_POINT ( 'NONE', #9537 ) ;
#33397 = DIRECTION ( 'NONE',  ( 0.000000000000000000, 0.000000000000000000, 1.000000000000000000 ) ) ;
#33398 = AXIS2_PLACEMENT_3D ( 'NONE', #12334, #41969, #39124 ) ;
#33399 = CIRCLE ( 'NONE', #26436, 116.0000000000000000 ) ;
#33400 = DIRECTION ( 'NONE',  ( -1.000000000000000000, -0.000000000000000000, 0.000000000000000000 ) ) ;
#33401 = DIRECTION ( 'NONE',  ( 1.000000000000000000, -1.058513553088275437E-16, 0.000000000000000000 ) ) ;
#33402 = CIRCLE ( 'NONE', #3424, 47.49900000000000944 ) ;
#33403 = VERTEX_POINT ( 'NONE', #22889 ) ;
#33404 = CARTESIAN_POINT ( 'NONE',  ( 22.90854556226722138, -2.055254544495723756, -74.83297477053847047 ) ) ;
#33405 = EDGE_CURVE ( 'NONE', #22707, #14639, #17764, .T. ) ;
#33406 = APPLICATION_CONTEXT ( 'automotive_design' ) ;
#33407 = CARTESIAN_POINT ( 'NONE',  ( -103.7695705685742240, -106.4195705685773135, 6.999999999999753975 ) ) ;
#33408 = EDGE_CURVE ( 'NONE', #25656, #26054, #19995, .T. ) ;
#33410 = DIRECTION ( 'NONE',  ( 0.000000000000000000, -0.8183027759081622499, -0.5747874102144165942 ) ) ;
#33409 = CARTESIAN_POINT ( 'NONE',  ( 47.55521504368574881, -12.05525454449572464, -70.64469547305695585 ) ) ;
#33411 = DIRECTION ( 'NONE',  ( -1.000000000000000000, -0.000000000000000000, 0.000000000000000000 ) ) ;
#33412 = ORIENTED_EDGE ( 'NONE', *, *, #33533, .F. ) ;
#33413 = SURFACE_STYLE_FILL_AREA ( #3496 ) ;
#33414 = CARTESIAN_POINT ( 'NONE',  ( -10.91816144241376563, 31.00000000000000355, -40.73603723627661566 ) ) ;
#33415 = ORIENTED_EDGE ( 'NONE', *, *, #361, .T. ) ;
#33416 = CARTESIAN_POINT ( 'NONE',  ( 17.99999999999999645, 111.1352304691229733, -15.40237066878481720 ) ) ;
#33417 = DIRECTION ( 'NONE',  ( -1.000000000000000000, 0.000000000000000000, 0.000000000000000000 ) ) ;
#33418 = ORIENTED_EDGE ( 'NONE', *, *, #20319, .F. ) ;
#33419 = DIRECTION ( 'NONE',  ( -1.000000000000000000, -0.000000000000000000, -0.000000000000000000 ) ) ;
#33420 = CARTESIAN_POINT ( 'NONE',  ( 5.583751958424166162, 40.00000000000000000, -42.43436172917101601 ) ) ;
#33421 = EDGE_CURVE ( 'NONE', #7262, #8485, #13470, .T. ) ;
#33422 = CARTESIAN_POINT ( 'NONE',  ( -46.12092335263332643, 40.00000000000000000, 22.64177125690310177 ) ) ;
#33423 = ORIENTED_EDGE ( 'NONE', *, *, #27416, .F. ) ;
#33424 = VECTOR ( 'NONE', #2077, 1000.000000000000000 ) ;
#33425 = VERTEX_POINT ( 'NONE', #39616 ) ;
#33426 = CYLINDRICAL_SURFACE ( 'NONE', #26228, 59.00000000000000000 ) ;
#33427 = DIRECTION ( 'NONE',  ( -1.000000000000000000, -0.000000000000000000, -0.000000000000000000 ) ) ;
#33428 = AXIS2_PLACEMENT_3D ( 'NONE', #36876, #39914, #36650 ) ;
#33429 = DIRECTION ( 'NONE',  ( -1.000000000000000000, 0.000000000000000000, -0.000000000000000000 ) ) ;
#33430 = EDGE_CURVE ( 'NONE', #20273, #36979, #15801, .T. ) ;
#33431 = VERTEX_POINT ( 'NONE', #16539 ) ;
#33432 = DIRECTION ( 'NONE',  ( 0.000000000000000000, 0.000000000000000000, 1.000000000000000000 ) ) ;
#33433 = ORIENTED_EDGE ( 'NONE', *, *, #36048, .F. ) ;
#33434 = CARTESIAN_POINT ( 'NONE',  ( -10.00000000000000000, 1.592040838891559450E-14, -130.0000000000000000 ) ) ;
#33435 = CARTESIAN_POINT ( 'NONE',  ( 17.99999999999999645, 11.41303419185120482, -111.6154788735834700 ) ) ;
#33436 = ORIENTED_EDGE ( 'NONE', *, *, #37792, .T. ) ;
#33437 = CARTESIAN_POINT ( 'NONE',  ( 17.99999999999999645, -17.77780072541623113, -114.6296200873377842 ) ) ;
#33438 = CARTESIAN_POINT ( 'NONE',  ( 0.000000000000000000, 35.54274411428215075, -115.1399337407602701 ) ) ;
#33439 = EDGE_CURVE ( 'NONE', #19109, #5464, #42232, .T. ) ;
#33440 = ORIENTED_EDGE ( 'NONE', *, *, #40638, .T. ) ;
#33441 = CARTESIAN_POINT ( 'NONE',  ( 17.99999999999999645, 82.63181128086733906, 81.41243003647002752 ) ) ;
#33442 = ORIENTED_EDGE ( 'NONE', *, *, #12173, .T. ) ;
#33443 = CARTESIAN_POINT ( 'NONE',  ( -2.107686228591307694E-13, 150.5000000000013642, 10.00000000000041744 ) ) ;
#33444 = ORIENTED_EDGE ( 'NONE', *, *, #14062, .T. ) ;
#33446 = VERTEX_POINT ( 'NONE', #39183 ) ;
#33445 = CARTESIAN_POINT ( 'NONE',  ( 18.00000000000000355, 0.000000000000000000, 0.000000000000000000 ) ) ;
#33447 = CARTESIAN_POINT ( 'NONE',  ( 60.82800096162477388, 31.00000000000000000, 30.10617641798563682 ) ) ;
#33448 = ORIENTED_EDGE ( 'NONE', *, *, #10489, .F. ) ;
#33449 = DIRECTION ( 'NONE',  ( -1.000000000000000000, -0.000000000000000000, -0.000000000000000000 ) ) ;
#33450 = ORIENTED_EDGE ( 'NONE', *, *, #40099, .T. ) ;
#33451 = CARTESIAN_POINT ( 'NONE',  ( 150.4999999999986926, 1.388241670201576064E-12, 6.999999999999959144 ) ) ;
#33452 = ORIENTED_EDGE ( 'NONE', *, *, #15658, .T. ) ;
#33453 = CARTESIAN_POINT ( 'NONE',  ( 83.84057477258951963, 39.99999999999999289, -22.33845567676512900 ) ) ;
#33455 = EDGE_CURVE ( 'NONE', #27141, #21142, #43109, .T. ) ;
#33454 = AXIS2_PLACEMENT_3D ( 'NONE', #19726, #40761, #16445 ) ;
#33457 = EDGE_CURVE ( 'NONE', #16830, #12278, #13256, .T. ) ;
#33456 = AXIS2_PLACEMENT_3D ( 'NONE', #25764, #5656, #19218 ) ;
#33459 = DIRECTION ( 'NONE',  ( -1.000000000000000000, -0.000000000000000000, 0.000000000000000000 ) ) ;
#33458 = CARTESIAN_POINT ( 'NONE',  ( 17.99999999999999645, 0.000000000000000000, 0.000000000000000000 ) ) ;
#33460 = AXIS2_PLACEMENT_3D ( 'NONE', #41417, #2138, #18360 ) ;
#33461 = DIRECTION ( 'NONE',  ( 0.000000000000000000, 0.000000000000000000, 1.000000000000000000 ) ) ;
#33462 = ORIENTED_EDGE ( 'NONE', *, *, #4641, .T. ) ;
#33463 = DIRECTION ( 'NONE',  ( 0.000000000000000000, -0.9826841245925228563, 0.1852887240871046171 ) ) ;
#33464 = ORIENTED_EDGE ( 'NONE', *, *, #23628, .T. ) ;
#33465 = VERTEX_POINT ( 'NONE', #40469 ) ;
#33466 = CARTESIAN_POINT ( 'NONE',  ( 18.00000000000000355, 0.000000000000000000, 0.000000000000000000 ) ) ;
#33467 = CARTESIAN_POINT ( 'NONE',  ( -21.28946418274055929, 31.00000000000000355, -79.45670318283352174 ) ) ;
#33468 = DIRECTION ( 'NONE',  ( 0.000000000000000000, 0.000000000000000000, -1.000000000000000000 ) ) ;
#33469 = EDGE_CURVE ( 'NONE', #2698, #16003, #10197, .T. ) ;
#33470 = ORIENTED_EDGE ( 'NONE', *, *, #20460, .F. ) ;
#33471 = ADVANCED_FACE ( 'NONE', ( #27408 ), #24384, .F. ) ;
#33472 = DIRECTION ( 'NONE',  ( -1.000000000000000000, 0.000000000000000000, 0.000000000000000000 ) ) ;
#33473 = CIRCLE ( 'NONE', #2801, 47.49900000000000233 ) ;
#33474 = ORIENTED_EDGE ( 'NONE', *, *, #35610, .T. ) ;
#33475 = CARTESIAN_POINT ( 'NONE',  ( 17.99999999999999645, -103.1672962317648512, -44.09967643725973119 ) ) ;
#33476 = CARTESIAN_POINT ( 'NONE',  ( 0.000000000000000000, -29.36437154452078246, 116.8684075565134890 ) ) ;
#33477 = CARTESIAN_POINT ( 'NONE',  ( 17.99999999999999645, 0.000000000000000000, 0.000000000000000000 ) ) ;
#33478 = CIRCLE ( 'NONE', #37647, 5.560781378645573980 ) ;
#33479 = EDGE_CURVE ( 'NONE', #4089, #16799, #5252, .T. ) ;
#33480 = ORIENTED_EDGE ( 'NONE', *, *, #10182, .T. ) ;
#33481 = LINE ( 'NONE', #39795, #17992 ) ;
#33482 = EDGE_LOOP ( 'NONE', ( #32664, #1208, #34387, #4467 ) ) ;
#33483 = AXIS2_PLACEMENT_3D ( 'NONE', #15883, #19585, #19163 ) ;
#33484 = CARTESIAN_POINT ( 'NONE',  ( 17.99999999999999645, -97.89532456239460601, -54.81585448086294576 ) ) ;
#33485 = CIRCLE ( 'NONE', #16836, 47.49900000000000233 ) ;
#33486 = ADVANCED_FACE ( 'NONE', ( #20457 ), #7313, .T. ) ;
#33487 = CIRCLE ( 'NONE', #23686, 20.00000000000000000 ) ;
#33488 = CYLINDRICAL_SURFACE ( 'NONE', #7453, 116.0000000000000000 ) ;
#33489 = CIRCLE ( 'NONE', #14718, 120.5010000000000190 ) ;
#33490 = DIRECTION ( 'NONE',  ( 0.000000000000000000, 0.000000000000000000, 1.000000000000000000 ) ) ;
#33491 = ORIENTED_EDGE ( 'NONE', *, *, #10678, .T. ) ;
#33492 = ORIENTED_EDGE ( 'NONE', *, *, #37666, .T. ) ;
#33493 = CARTESIAN_POINT ( 'NONE',  ( 17.99999999999999645, -5.492704054967489924, 115.8698847939556202 ) ) ;
#33494 = CARTESIAN_POINT ( 'NONE',  ( -2.499999999999999556, 3.061616997868382648E-16, 3.469446951953614189E-15 ) ) ;
#33495 = DIRECTION ( 'NONE',  ( 1.000000000000000000, -0.000000000000000000, 0.000000000000000000 ) ) ;
#33497 = ORIENTED_EDGE ( 'NONE', *, *, #33274, .F. ) ;
#33496 = CARTESIAN_POINT ( 'NONE',  ( 17.99999999999999645, 0.000000000000000000, 0.000000000000000000 ) ) ;
#33498 = CARTESIAN_POINT ( 'NONE',  ( -26.24023198663968515, 31.00000000000000355, -20.19409642360271917 ) ) ;
#33499 = DIRECTION ( 'NONE',  ( 1.000000000000000000, 0.000000000000000000, -3.273063162220425331E-16 ) ) ;
#33501 = ORIENTED_EDGE ( 'NONE', *, *, #26286, .T. ) ;
#33500 = LINE ( 'NONE', #3585, #14051 ) ;
#33502 = ORIENTED_EDGE ( 'NONE', *, *, #19618, .T. ) ;
#33503 = CARTESIAN_POINT ( 'NONE',  ( 0.000000000000000000, 46.83041522348636931, -101.9567785075596618 ) ) ;
#33504 = LINE ( 'NONE', #23932, #39110 ) ;
#33505 = CARTESIAN_POINT ( 'NONE',  ( 15.70068437845367093, 40.00000000000000000, 46.50252577712053892 ) ) ;
#33506 = EDGE_CURVE ( 'NONE', #41947, #7746, #10604, .T. ) ;
#33507 = EDGE_CURVE ( 'NONE', #25878, #6181, #7106, .T. ) ;
#33508 = LINE ( 'NONE', #20245, #21494 ) ;
#33509 = ADVANCED_FACE ( 'NONE', ( #36992 ), #13682, .T. ) ;
#33510 = ADVANCED_FACE ( 'NONE', ( #761 ), #21118, .T. ) ;
#33511 = CARTESIAN_POINT ( 'NONE',  ( 8.999999999999998224, 28.35267316522783432, 22.18391138608718549 ) ) ;
#33512 = CIRCLE ( 'NONE', #17515, 10.49999999999999467 ) ;
#33513 = EDGE_LOOP ( 'NONE', ( #21400, #12688, #1153, #2616, #35344 ) ) ;
#33514 = DIRECTION ( 'NONE',  ( -1.000000000000000000, 0.000000000000000000, 0.000000000000000000 ) ) ;
#33515 = VERTEX_POINT ( 'NONE', #40680 ) ;
#33516 = VECTOR ( 'NONE', #27628, 1000.000000000000000 ) ;
#33517 = DIRECTION ( 'NONE',  ( 0.000000000000000000, 0.8951632913550603421, 0.4457383557765422499 ) ) ;
#33518 = CARTESIAN_POINT ( 'NONE',  ( 18.00000000000000355, 29.60891106212788415, 37.14118181634774629 ) ) ;
#33519 = AXIS2_PLACEMENT_3D ( 'NONE', #7805, #6344, #32958 ) ;
#33520 = CARTESIAN_POINT ( 'NONE',  ( 11.12085686420672381, 31.00000000000000355, -41.54537790535560760 ) ) ;
#33521 = DIRECTION ( 'NONE',  ( 0.000000000000000000, -0.9911528310040084166, 0.1327255272837126743 ) ) ;
#33522 = ORIENTED_EDGE ( 'NONE', *, *, #30582, .F. ) ;
#33523 = AXIS2_PLACEMENT_3D ( 'NONE', #30454, #40011, #33700 ) ;
#33524 = DIRECTION ( 'NONE',  ( -1.000000000000000000, 3.035766082959412415E-17, 0.000000000000000000 ) ) ;
#33525 = VERTEX_POINT ( 'NONE', #13905 ) ;
#33526 = CARTESIAN_POINT ( 'NONE',  ( -49.27414759474276451, 31.00000000000000711, 85.34056160678568403 ) ) ;
#33527 = CIRCLE ( 'NONE', #30062, 13.60000000000000142 ) ;
#33528 = ORIENTED_EDGE ( 'NONE', *, *, #39856, .F. ) ;
#33529 = CARTESIAN_POINT ( 'NONE',  ( 9.000000000000001776, -23.85344185397275041, 113.5209818126990200 ) ) ;
#33530 = CARTESIAN_POINT ( 'NONE',  ( -10.54315780145427617, 31.00000000000000355, 79.17709703063970039 ) ) ;
#33531 = CARTESIAN_POINT ( 'NONE',  ( -53.37462671635322664, 40.00000000000000711, 60.68184199298008252 ) ) ;
#33532 = FACE_OUTER_BOUND ( 'NONE', #7444, .T. ) ;
#33533 = EDGE_CURVE ( 'NONE', #11136, #14824, #9410, .T. ) ;
#33534 = AXIS2_PLACEMENT_3D ( 'NONE', #27981, #37759, #41025 ) ;
#33535 = VERTEX_POINT ( 'NONE', #26986 ) ;
#33536 = ORIENTED_EDGE ( 'NONE', *, *, #1853, .F. ) ;
#33537 = CARTESIAN_POINT ( 'NONE',  ( 17.99999999999999645, -2.007101075700182591, 31.43498920425968279 ) ) ;
#33538 = DIRECTION ( 'NONE',  ( -1.000000000000000000, 0.000000000000000000, 0.000000000000000000 ) ) ;
#33539 = EDGE_CURVE ( 'NONE', #33396, #40845, #30686, .T. ) ;
#33541 = ORIENTED_EDGE ( 'NONE', *, *, #17154, .F. ) ;
#33540 = DIRECTION ( 'NONE',  ( -1.000000000000000000, 0.000000000000000000, 0.000000000000000000 ) ) ;
#33542 = CARTESIAN_POINT ( 'NONE',  ( 17.99999999999999645, 0.000000000000000000, 0.000000000000000000 ) ) ;
#33543 = ORIENTED_EDGE ( 'NONE', *, *, #15812, .F. ) ;
#33544 = DIRECTION ( 'NONE',  ( 0.000000000000000000, 0.000000000000000000, 1.000000000000000000 ) ) ;
#33545 = CARTESIAN_POINT ( 'NONE',  ( -70.72766149062127283, 40.00000000000000711, 54.26934393422349956 ) ) ;
#33546 = FACE_OUTER_BOUND ( 'NONE', #14074, .T. ) ;
#33547 = AXIS2_PLACEMENT_3D ( 'NONE', #41058, #4860, #24986 ) ;
#33548 = VECTOR ( 'NONE', #23725, 1000.000000000000000 ) ;
#33549 = ORIENTED_EDGE ( 'NONE', *, *, #23835, .F. ) ;
#33550 = CARTESIAN_POINT ( 'NONE',  ( 17.99999999999999645, -11.49545354908957862, 29.80986809967256335 ) ) ;
#33551 = CARTESIAN_POINT ( 'NONE',  ( -6.075999999999997847, 0.000000000000000000, 19.11697999999999809 ) ) ;
#33552 = CIRCLE ( 'NONE', #10575, 116.0000000000000000 ) ;
#33553 = VERTEX_POINT ( 'NONE', #37846 ) ;
#33554 = CARTESIAN_POINT ( 'NONE',  ( -1.420922472151883646E-13, 9.833206111663764869E-13, 369.6955262170047831 ) ) ;
#33555 = EDGE_LOOP ( 'NONE', ( #1982, #28814, #12697, #38775 ) ) ;
#33556 = FACE_OUTER_BOUND ( 'NONE', #7145, .T. ) ;
#33557 = VERTEX_POINT ( 'NONE', #23728 ) ;
#33558 = CARTESIAN_POINT ( 'NONE',  ( 24.14050371820133023, 40.00000000000000000, 13.97356841391088444 ) ) ;
#33559 = DIRECTION ( 'NONE',  ( 0.000000000000000000, 0.5877852522924686962, 0.8090169943749506709 ) ) ;
#33560 = DIRECTION ( 'NONE',  ( -1.000000000000000000, 3.336006684570783348E-17, 0.000000000000000000 ) ) ;
#33561 = DIRECTION ( 'NONE',  ( -1.000000000000000000, -0.000000000000000000, -0.000000000000000000 ) ) ;
#33562 = EDGE_CURVE ( 'NONE', #8378, #27124, #34369, .T. ) ;
#33563 = EDGE_CURVE ( 'NONE', #27630, #27814, #33718, .T. ) ;
#33564 = CYLINDRICAL_SURFACE ( 'NONE', #14369, 20.00000000000000711 ) ;
#33565 = ORIENTED_EDGE ( 'NONE', *, *, #30551, .F. ) ;
#33567 = DIRECTION ( 'NONE',  ( -1.000000000000000000, 0.000000000000000000, -0.000000000000000000 ) ) ;
#33566 = DIRECTION ( 'NONE',  ( 1.000000000000000000, 0.000000000000000000, -0.000000000000000000 ) ) ;
#33568 = EDGE_CURVE ( 'NONE', #40564, #719, #12922, .T. ) ;
#33569 = ORIENTED_EDGE ( 'NONE', *, *, #2813, .F. ) ;
#33570 = CARTESIAN_POINT ( 'NONE',  ( 17.99999999999999645, -75.03166794516737070, -94.29071961951585479 ) ) ;
#33571 = DIRECTION ( 'NONE',  ( 1.000000000000000000, 0.000000000000000000, 0.000000000000000000 ) ) ;
#33572 = VERTEX_POINT ( 'NONE', #4253 ) ;
#33573 = DIRECTION ( 'NONE',  ( 0.000000000000000000, 0.000000000000000000, 1.000000000000000000 ) ) ;
#33574 = LINE ( 'NONE', #17030, #27938 ) ;
#33575 = DIRECTION ( 'NONE',  ( 1.000000000000000000, 0.000000000000000000, -6.546126324440850663E-16 ) ) ;
#33576 = CARTESIAN_POINT ( 'NONE',  ( 8.815036365794538753, 31.00000000000000355, 66.85656860134390911 ) ) ;
#33577 = AXIS2_PLACEMENT_3D ( 'NONE', #13827, #40819, #24519 ) ;
#33578 = EDGE_CURVE ( 'NONE', #11001, #32412, #16526, .T. ) ;
#33579 = ORIENTED_EDGE ( 'NONE', *, *, #21007, .T. ) ;
#33580 = CARTESIAN_POINT ( 'NONE',  ( -41.52979953746218911, 31.00000000000000355, 5.398177843165337109 ) ) ;
#33581 = CIRCLE ( 'NONE', #4322, 47.49899999999999523 ) ;
#33582 = CARTESIAN_POINT ( 'NONE',  ( -80.10416666582359824, 40.00000000000000711, -5.235987747607834031 ) ) ;
#33583 = AXIS2_PLACEMENT_3D ( 'NONE', #1367, #41279, #11428 ) ;
#33584 = CARTESIAN_POINT ( 'NONE',  ( 17.99999999999999645, 111.8797445107943531, 8.437727291344614855 ) ) ;
#33585 = DIRECTION ( 'NONE',  ( -1.000000000000000000, -0.000000000000000000, -0.000000000000000000 ) ) ;
#33586 = ORIENTED_EDGE ( 'NONE', *, *, #26869, .T. ) ;
#33587 = DIRECTION ( 'NONE',  ( -1.000000000000000000, -0.000000000000000000, 0.000000000000000000 ) ) ;
#33588 = ADVANCED_FACE ( 'NONE', ( #973 ), #14327, .F. ) ;
#33589 = CARTESIAN_POINT ( 'NONE',  ( 0.000000000000000000, -10.40101730206447961, 120.0512800434970728 ) ) ;
#33590 = PRODUCT_DEFINITION_SHAPE ( 'NONE', 'NONE',  #43187 ) ;
#33591 = ORIENTED_EDGE ( 'NONE', *, *, #6606, .T. ) ;
#33592 = CARTESIAN_POINT ( 'NONE',  ( -44.33513214241411760, 40.00000000000000000, 38.89722855811361768 ) ) ;
#33593 = DIRECTION ( 'NONE',  ( -1.000000000000000000, 0.000000000000000000, -0.000000000000000000 ) ) ;
#33594 = CARTESIAN_POINT ( 'NONE',  ( 17.99999999999999645, 0.000000000000000000, 0.000000000000000000 ) ) ;
#33595 = ORIENTED_EDGE ( 'NONE', *, *, #14398, .T. ) ;
#33596 = CARTESIAN_POINT ( 'NONE',  ( 17.99999999999999645, 0.000000000000000000, 0.000000000000000000 ) ) ;
#33597 = LINE ( 'NONE', #9825, #22953 ) ;
#33598 = VERTEX_POINT ( 'NONE', #17836 ) ;
#33599 = LINE ( 'NONE', #17058, #5418 ) ;
#33600 = ORIENTED_EDGE ( 'NONE', *, *, #33405, .T. ) ;
#33601 = AXIS2_PLACEMENT_3D ( 'NONE', #18821, #38186, #1526 ) ;
#33602 = ORIENTED_EDGE ( 'NONE', *, *, #40938, .F. ) ;
#33603 = LINE ( 'NONE', #16857, #22325 ) ;
#33604 = CIRCLE ( 'NONE', #11333, 58.99999999999998579 ) ;
#33605 = CARTESIAN_POINT ( 'NONE',  ( -88.68107738130200346, 31.00000000000000711, 23.63280646692842524 ) ) ;
#33606 = VERTEX_POINT ( 'NONE', #35021 ) ;
#33607 = CIRCLE ( 'NONE', #22509, 116.0000000000000000 ) ;
#33608 = DIRECTION ( 'NONE',  ( 0.000000000000000000, 0.000000000000000000, 1.000000000000000000 ) ) ;
#33609 = EDGE_CURVE ( 'NONE', #34488, #19682, #31978, .T. ) ;
#33610 = FACE_OUTER_BOUND ( 'NONE', #1896, .T. ) ;
#33611 = ORIENTED_EDGE ( 'NONE', *, *, #9253, .F. ) ;
#33612 = CYLINDRICAL_SURFACE ( 'NONE', #32182, 2.649999999999971934 ) ;
#33613 = CIRCLE ( 'NONE', #6421, 116.0000000000000000 ) ;
#33614 = FACE_OUTER_BOUND ( 'NONE', #5106, .T. ) ;
#33616 = DIRECTION ( 'NONE',  ( 0.000000000000000000, 0.000000000000000000, 1.000000000000000000 ) ) ;
#33615 = FACE_OUTER_BOUND ( 'NONE', #1137, .T. ) ;
#33617 = CARTESIAN_POINT ( 'NONE',  ( 9.999999999999998224, 0.000000000000000000, -12.59999999999999964 ) ) ;
#33618 = ORIENTED_EDGE ( 'NONE', *, *, #10619, .T. ) ;
#33619 = EDGE_CURVE ( 'NONE', #26002, #20435, #2447, .T. ) ;
#33620 = DIRECTION ( 'NONE',  ( 0.7071067811865487940, 0.000000000000000000, 0.7071067811865463515 ) ) ;
#33621 = CARTESIAN_POINT ( 'NONE',  ( 11.92156526682413720, 31.00000000000000355, 35.08788755311113761 ) ) ;
#33622 = VERTEX_POINT ( 'NONE', #5126 ) ;
#33623 = DIRECTION ( 'NONE',  ( -1.000000000000000000, 0.000000000000000000, 0.000000000000000000 ) ) ;
#33624 = EDGE_CURVE ( 'NONE', #21317, #2151, #40863, .T. ) ;
#33625 = CARTESIAN_POINT ( 'NONE',  ( 0.000000000000000000, 0.7408941433508176022, -1.199999999999999956 ) ) ;
#33626 = ORIENTED_EDGE ( 'NONE', *, *, #24244, .F. ) ;
#33627 = EDGE_CURVE ( 'NONE', #37085, #4630, #8736, .T. ) ;
#33628 = DIRECTION ( 'NONE',  ( -1.000000000000000000, -0.000000000000000000, -0.000000000000000000 ) ) ;
#33629 = CARTESIAN_POINT ( 'NONE',  ( -3.436116956419240864, 40.00000000000000000, -52.39583333462812931 ) ) ;
#33630 = CARTESIAN_POINT ( 'NONE',  ( -26.44890248586417414, 40.00000000000000000, -34.59877114778964113 ) ) ;
#33631 = CIRCLE ( 'NONE', #41287, 116.0000000000000000 ) ;
#33632 = ORIENTED_EDGE ( 'NONE', *, *, #24927, .T. ) ;
#33633 = DIRECTION ( 'NONE',  ( 0.000000000000000000, -7.709882115452474222E-16, -1.000000000000000000 ) ) ;
#33634 = DIRECTION ( 'NONE',  ( 0.000000000000000000, 0.000000000000000000, 1.000000000000000000 ) ) ;
#33635 = VECTOR ( 'NONE', #6239, 1000.000000000000000 ) ;
#33637 = EDGE_CURVE ( 'NONE', #41108, #6459, #24199, .T. ) ;
#33636 = CARTESIAN_POINT ( 'NONE',  ( 17.99999999999999645, -83.58328028049713510, 80.43528614701295965 ) ) ;
#33638 = ORIENTED_EDGE ( 'NONE', *, *, #9084, .F. ) ;
#33639 = CARTESIAN_POINT ( 'NONE',  ( -1.799870782497340782, 40.00000000000000000, 27.60416666422008802 ) ) ;
#33640 = ORIENTED_EDGE ( 'NONE', *, *, #12353, .F. ) ;
#33641 = DIRECTION ( 'NONE',  ( -1.000000000000000000, 0.000000000000000000, -0.000000000000000000 ) ) ;
#33642 = EDGE_CURVE ( 'NONE', #37671, #20999, #31047, .T. ) ;
#33643 = AXIS2_PLACEMENT_3D ( 'NONE', #36845, #30954, #24230 ) ;
#33644 = CARTESIAN_POINT ( 'NONE',  ( 1.144235203016666258, 3.958177651039090250, -0.09382832055445661235 ) ) ;
#33645 = ORIENTED_EDGE ( 'NONE', *, *, #34572, .F. ) ;
#33646 = DIRECTION ( 'NONE',  ( 0.000000000000000000, 0.000000000000000000, -1.000000000000000000 ) ) ;
#33647 = DIRECTION ( 'NONE',  ( 0.000000000000000000, 0.000000000000000000, 1.000000000000000000 ) ) ;
#33648 = ORIENTED_EDGE ( 'NONE', *, *, #25037, .F. ) ;
#33649 = LINE ( 'NONE', #37353, #24301 ) ;
#33650 = ORIENTED_EDGE ( 'NONE', *, *, #24190, .F. ) ;
#33651 = CARTESIAN_POINT ( 'NONE',  ( -93.98204972788910538, -12.05525454449572109, 39.37702493556011518 ) ) ;
#33652 = ORIENTED_EDGE ( 'NONE', *, *, #40, .F. ) ;
#33654 = ORIENTED_EDGE ( 'NONE', *, *, #10484, .T. ) ;
#33653 = DIRECTION ( 'NONE',  ( 1.000000000000000000, -1.373900992973642263E-15, -3.996523416598957436E-16 ) ) ;
#33655 = CARTESIAN_POINT ( 'NONE',  ( -56.33579487689731735, 31.00000000000000355, -27.88694065509425002 ) ) ;
#33656 = VERTEX_POINT ( 'NONE', #41778 ) ;
#33657 = CARTESIAN_POINT ( 'NONE',  ( -6.259644161404860030E-16, -4.618802153517027165, -3.433295621305388234 ) ) ;
#33658 = EDGE_CURVE ( 'NONE', #12767, #13702, #6636, .T. ) ;
#33659 = ORIENTED_EDGE ( 'NONE', *, *, #36093, .F. ) ;
#33660 = DIRECTION ( 'NONE',  ( 0.000000000000000000, -0.6382441836448109473, -0.7698339834299138262 ) ) ;
#33661 = EDGE_LOOP ( 'NONE', ( #29167, #34962, #2680, #19526 ) ) ;
#33662 = CIRCLE ( 'NONE', #31595, 52.00000000000000000 ) ;
#33663 = CARTESIAN_POINT ( 'NONE',  ( -71.82650799747224823, 40.00000000000000711, -41.60779115366585756 ) ) ;
#33665 = CARTESIAN_POINT ( 'NONE',  ( 18.00000000000000355, -5.667686777402029641, 46.64153600743603789 ) ) ;
#33664 = DIRECTION ( 'NONE',  ( -1.000000000000000000, -0.000000000000000000, -0.000000000000000000 ) ) ;
#33666 = CARTESIAN_POINT ( 'NONE',  ( -4.000000000000000000, 2.309401076758498483, -3.433295621305379353 ) ) ;
#33667 = ORIENTED_EDGE ( 'NONE', *, *, #28226, .F. ) ;
#33668 = CARTESIAN_POINT ( 'NONE',  ( 9.000000000000001776, 5.492704054968225336, -115.8698847939555776 ) ) ;
#33669 = MECHANICAL_DESIGN_GEOMETRIC_PRESENTATION_REPRESENTATION (  '', ( #26029 ), #19759 ) ;
#33670 = ORIENTED_EDGE ( 'NONE', *, *, #29109, .T. ) ;
#33671 = EDGE_CURVE ( 'NONE', #8463, #31266, #38005, .T. ) ;
#33672 =( NAMED_UNIT ( * ) SI_UNIT ( $, .STERADIAN. ) SOLID_ANGLE_UNIT ( ) );
#33673 = CARTESIAN_POINT ( 'NONE',  ( 0.000000000000000000, 0.000000000000000000, 0.000000000000000000 ) ) ;
#33674 = ORIENTED_EDGE ( 'NONE', *, *, #27471, .F. ) ;
#33675 = CARTESIAN_POINT ( 'NONE',  ( 0.000000000000000000, -27.43636312076348815, 38.14186064215142835 ) ) ;
#33676 = EDGE_CURVE ( 'NONE', #28259, #36486, #42162, .T. ) ;
#33677 = CARTESIAN_POINT ( 'NONE',  ( -84.90650804512098659, 31.00000000000000711, 28.83788733109305014 ) ) ;
#33678 = CARTESIAN_POINT ( 'NONE',  ( 2.756197834950227410, 3.027510591568626896, -3.223146290109805356 ) ) ;
#33679 = ORIENTED_EDGE ( 'NONE', *, *, #21121, .F. ) ;
#33680 = AXIS2_PLACEMENT_3D ( 'NONE', #23666, #26694, #10092 ) ;
#33681 = LINE ( 'NONE', #24119, #34497 ) ;
#33682 = EDGE_LOOP ( 'NONE', ( #24962, #36667, #18752, #39921 ) ) ;
#33683 = CARTESIAN_POINT ( 'NONE',  ( 8.999999999999998224, -90.81729652456212420, 72.16798910853589177 ) ) ;
#33684 = AXIS2_PLACEMENT_3D ( 'NONE', #39290, #31938, #9424 ) ;
#33685 = DIRECTION ( 'NONE',  ( 1.000000000000000000, -0.000000000000000000, -0.000000000000000000 ) ) ;
#33686 = PRESENTATION_STYLE_ASSIGNMENT (( #521 ) ) ;
#33687 = VECTOR ( 'NONE', #18926, 1000.000000000000000 ) ;
#33688 = DIRECTION ( 'NONE',  ( 0.000000000000000000, 0.000000000000000000, 1.000000000000000000 ) ) ;
#33689 = AXIS2_PLACEMENT_3D ( 'NONE', #8969, #25790, #39050 ) ;
#33690 = VERTEX_POINT ( 'NONE', #24818 ) ;
#33691 = CARTESIAN_POINT ( 'NONE',  ( 20.00000000000000000, 2.449293598294706513E-15, -6.000000000000000000 ) ) ;
#33692 = ORIENTED_EDGE ( 'NONE', *, *, #19091, .F. ) ;
#33693 = EDGE_CURVE ( 'NONE', #28268, #28450, #33116, .T. ) ;
#33694 = DIRECTION ( 'NONE',  ( -1.000000000000000000, 0.000000000000000000, 0.000000000000000000 ) ) ;
#33695 = ADVANCED_FACE ( 'NONE', ( #4918 ), #25451, .T. ) ;
#33696 = CARTESIAN_POINT ( 'NONE',  ( 109.0695705685734254, 106.4195705685780524, 10.00000000000025047 ) ) ;
#33697 = CYLINDRICAL_SURFACE ( 'NONE', #12911, 59.00000000000000000 ) ;
#33698 = ORIENTED_EDGE ( 'NONE', *, *, #32301, .F. ) ;
#33699 = ORIENTED_EDGE ( 'NONE', *, *, #1684, .T. ) ;
#33700 = DIRECTION ( 'NONE',  ( 0.000000000000000000, 1.881733940042638318E-15, -1.000000000000000000 ) ) ;
#33701 =( GEOMETRIC_REPRESENTATION_CONTEXT ( 3 ) GLOBAL_UNCERTAINTY_ASSIGNED_CONTEXT ( ( #17835 ) ) GLOBAL_UNIT_ASSIGNED_CONTEXT ( ( #25202, #41935, #15573 ) ) REPRESENTATION_CONTEXT ( 'NONE', 'WORKASPACE' ) );
#33702 = DIRECTION ( 'NONE',  ( 0.000000000000000000, 0.000000000000000000, 1.000000000000000000 ) ) ;
#33703 = CARTESIAN_POINT ( 'NONE',  ( 17.99999999999999645, 0.000000000000000000, 0.000000000000000000 ) ) ;
#33705 = ORIENTED_EDGE ( 'NONE', *, *, #33988, .F. ) ;
#33704 = DIRECTION ( 'NONE',  ( 0.000000000000000000, 0.000000000000000000, 1.000000000000000000 ) ) ;
#33706 = CARTESIAN_POINT ( 'NONE',  ( 25.29542371717656835, 31.00000000000000355, 28.93716311998947788 ) ) ;
#33707 = VECTOR ( 'NONE', #20506, 1000.000000000000000 ) ;
#33708 = EDGE_CURVE ( 'NONE', #3331, #31747, #8835, .T. ) ;
#33710 = VERTEX_POINT ( 'NONE', #25671 ) ;
#33709 = LINE ( 'NONE', #14110, #13304 ) ;
#33711 = ORIENTED_EDGE ( 'NONE', *, *, #4324, .F. ) ;
#33712 = DIRECTION ( 'NONE',  ( -1.000000000000000000, 0.000000000000000000, 0.000000000000000000 ) ) ;
#33713 = DIRECTION ( 'NONE',  ( 1.000000000000000000, 0.000000000000000000, 0.000000000000000000 ) ) ;
#33714 = CARTESIAN_POINT ( 'NONE',  ( 24.55685208795062380, 40.00000000000000000, -49.59815698162134368 ) ) ;
#33715 = VECTOR ( 'NONE', #25896, 1000.000000000000000 ) ;
#33716 = DIRECTION ( 'NONE',  ( -1.000000000000000000, 0.000000000000000000, 0.000000000000000000 ) ) ;
#33717 = AXIS2_PLACEMENT_3D ( 'NONE', #25149, #12041, #28615 ) ;
#33718 = LINE ( 'NONE', #33511, #26871 ) ;
#33719 = ORIENTED_EDGE ( 'NONE', *, *, #9407, .F. ) ;
#33720 = CARTESIAN_POINT ( 'NONE',  ( 17.99999999999999645, 23.21237537461889389, -109.7700237000589709 ) ) ;
#33721 = ORIENTED_EDGE ( 'NONE', *, *, #10671, .F. ) ;
#33722 = EDGE_CURVE ( 'NONE', #29560, #15632, #33798, .T. ) ;
#33723 = CIRCLE ( 'NONE', #32327, 59.00000000000000711 ) ;
#33724 = CARTESIAN_POINT ( 'NONE',  ( 0.000000000000000000, 92.10690493017060021, 64.06707842432207656 ) ) ;
#33725 = FACE_OUTER_BOUND ( 'NONE', #30722, .T. ) ;
#33726 = EDGE_CURVE ( 'NONE', #6952, #26365, #19920, .T. ) ;
#33727 = CARTESIAN_POINT ( 'NONE',  ( -59.89583333444493718, 31.00000000000000711, 3.926990808566372060 ) ) ;
#33728 = CARTESIAN_POINT ( 'NONE',  ( 17.99999999999999645, -108.8684555192045025, -27.12806418649726936 ) ) ;
#33729 = EDGE_LOOP ( 'NONE', ( #28794, #20182, #13880, #22009 ) ) ;
#33730 = ADVANCED_FACE ( 'NONE', ( #21971 ), #34585, .T. ) ;
#33731 = AXIS2_PLACEMENT_3D ( 'NONE', #656, #17081, #14014 ) ;
#33732 = CARTESIAN_POINT ( 'NONE',  ( 0.000000000000000000, -27.79676263918163315, -37.88001506494799031 ) ) ;
#33733 = ORIENTED_EDGE ( 'NONE', *, *, #9429, .T. ) ;
#33734 = CARTESIAN_POINT ( 'NONE',  ( 20.96880926229634312, 40.00000000000000000, -12.11681000168150213 ) ) ;
#33735 = VECTOR ( 'NONE', #10437, 1000.000000000000000 ) ;
#33736 = ORIENTED_EDGE ( 'NONE', *, *, #12622, .F. ) ;
#33737 = CARTESIAN_POINT ( 'NONE',  ( 0.000000000000000000, 46.12538073176499154, -111.3235835452206715 ) ) ;
#33738 = CARTESIAN_POINT ( 'NONE',  ( 0.000000000000000000, 0.000000000000000000, 9.999999999999998224 ) ) ;
#33739 = CARTESIAN_POINT ( 'NONE',  ( -71.33925323112771366, 31.00000000000000711, 9.290813765106920030 ) ) ;
#33740 = CARTESIAN_POINT ( 'NONE',  ( 69.81317433577432041, 39.99999999999999289, 34.54326205988235188 ) ) ;
#33741 = CARTESIAN_POINT ( 'NONE',  ( 17.99999999999999645, 80.74349901498408144, 77.90224541347306797 ) ) ;
#33742 = CIRCLE ( 'NONE', #14978, 13.59999999999999964 ) ;
#33743 = ORIENTED_EDGE ( 'NONE', *, *, #7405, .F. ) ;
#33744 = DIRECTION ( 'NONE',  ( 0.000000000000000000, 0.000000000000000000, -1.000000000000000000 ) ) ;
#33745 = VERTEX_POINT ( 'NONE', #31333 ) ;
#33746 = CARTESIAN_POINT ( 'NONE',  ( 0.000000000000000000, -31.08872492059927595, -41.68322423723131465 ) ) ;
#33747 = CIRCLE ( 'NONE', #20555, 59.00000000000001421 ) ;
#33748 = ADVANCED_FACE ( 'NONE', ( #1417 ), #41331, .T. ) ;
#33749 = CARTESIAN_POINT ( 'NONE',  ( 1.567478505476134606E-15, 4.618802153517012066, -5.000000000000000000 ) ) ;
#33750 = EDGE_CURVE ( 'NONE', #26640, #19094, #5353, .T. ) ;
#33751 = EDGE_CURVE ( 'NONE', #21496, #32501, #25046, .T. ) ;
#33752 = ADVANCED_FACE ( 'NONE', ( #29143 ), #33021, .F. ) ;
#33753 = CIRCLE ( 'NONE', #7275, 116.0000000000000000 ) ;
#33755 = ORIENTED_EDGE ( 'NONE', *, *, #20258, .T. ) ;
#33754 = CARTESIAN_POINT ( 'NONE',  ( 33.90854556226734218, -40.05525454449572464, -74.83297477053821467 ) ) ;
#33756 = DIRECTION ( 'NONE',  ( 0.000000000000000000, -0.6736956436465479925, -0.7390089172206675272 ) ) ;
#33757 = ORIENTED_EDGE ( 'NONE', *, *, #243, .T. ) ;
#33758 = CARTESIAN_POINT ( 'NONE',  ( 2.855764796983346177, -2.970025579236428737, -0.09382832055446485575 ) ) ;
#33759 = CARTESIAN_POINT ( 'NONE',  ( -54.00384411202717416, 40.00000000000000711, 70.40394205935166383 ) ) ;
#33760 = CARTESIAN_POINT ( 'NONE',  ( -10.00000000000000000, 0.000000000000000000, 0.000000000000000000 ) ) ;
#33761 = ORIENTED_EDGE ( 'NONE', *, *, #30559, .T. ) ;
#33762 = DIRECTION ( 'NONE',  ( -1.000000000000000000, 0.000000000000000000, -0.000000000000000000 ) ) ;
#33763 = FACE_OUTER_BOUND ( 'NONE', #26084, .T. ) ;
#33764 = ORIENTED_EDGE ( 'NONE', *, *, #18108, .T. ) ;
#33765 = CARTESIAN_POINT ( 'NONE',  ( 17.99999999999999645, 0.000000000000000000, 0.000000000000000000 ) ) ;
#33766 =( LENGTH_UNIT ( ) NAMED_UNIT ( * ) SI_UNIT ( .MILLI., .METRE. ) );
#33767 = VERTEX_POINT ( 'NONE', #5980 ) ;
#33768 = CARTESIAN_POINT ( 'NONE',  ( 0.000000000000000000, 0.000000000000000000, 0.000000000000000000 ) ) ;
#33769 = ORIENTED_EDGE ( 'NONE', *, *, #21673, .F. ) ;
#33770 = CARTESIAN_POINT ( 'NONE',  ( 21.18498618631003438, 40.00000000000000000, 18.62224443192851098 ) ) ;
#33771 = DIRECTION ( 'NONE',  ( -1.000000000000000000, 0.000000000000000000, 0.000000000000000000 ) ) ;
#33772 = CARTESIAN_POINT ( 'NONE',  ( 18.00000000000000355, -46.87740477351715640, -3.172455868805708956 ) ) ;
#33773 = DIRECTION ( 'NONE',  ( 1.000000000000000000, 0.000000000000000000, 0.000000000000000000 ) ) ;
#33774 = CARTESIAN_POINT ( 'NONE',  ( 1.598609366639573350E-14, -1.063425437509180407E-13, -40.00000000000000000 ) ) ;
#33776 = EDGE_LOOP ( 'NONE', ( #15221, #18853, #43045, #7895 ) ) ;
#33775 = AXIS2_PLACEMENT_3D ( 'NONE', #14813, #11527, #8246 ) ;
#33778 = CYLINDRICAL_SURFACE ( 'NONE', #35269, 116.0000000000000000 ) ;
#33777 = DIRECTION ( 'NONE',  ( 1.000000000000000000, 0.000000000000000000, 0.000000000000000000 ) ) ;
#33779 = VERTEX_POINT ( 'NONE', #42411 ) ;
#33780 = ADVANCED_FACE ( 'NONE', ( #26291 ), #26499, .F. ) ;
#33781 = CIRCLE ( 'NONE', #21321, 120.5010000000000474 ) ;
#33782 = CARTESIAN_POINT ( 'NONE',  ( 5.657435538624008755E-15, 4.615443851143735910E-16, -20.00000000000000000 ) ) ;
#33783 = VECTOR ( 'NONE', #20353, 1000.000000000000114 ) ;
#33784 = EDGE_CURVE ( 'NONE', #5213, #20054, #40071, .T. ) ;
#33785 = CARTESIAN_POINT ( 'NONE',  ( 103.7695705685763556, -106.4195705685744855, 9.999999999999998224 ) ) ;
#33786 = EDGE_LOOP ( 'NONE', ( #12856, #17559, #21723, #16243 ) ) ;
#33787 = DIRECTION ( 'NONE',  ( -1.000000000000000000, -0.000000000000000000, -0.000000000000000000 ) ) ;
#33788 = STYLED_ITEM ( 'NONE', ( #21784 ), #27502 ) ;
#33789 = DIRECTION ( 'NONE',  ( -1.000000000000000000, -0.000000000000000000, -0.000000000000000000 ) ) ;
#33790 = DIRECTION ( 'NONE',  ( -1.000000000000000000, -0.000000000000000000, -0.000000000000000000 ) ) ;
#33791 = CARTESIAN_POINT ( 'NONE',  ( -4.745113895469965648, 31.00000000000000355, -72.39583333427917466 ) ) ;
#33792 = ORIENTED_EDGE ( 'NONE', *, *, #6192, .F. ) ;
#33793 = CARTESIAN_POINT ( 'NONE',  ( 6.367266499441480043, 31.00000000000000355, 48.98256792610027333 ) ) ;
#33794 = CARTESIAN_POINT ( 'NONE',  ( 60.46509673945340779, 39.99999999999999289, 46.37897171328766888 ) ) ;
#33795 = CARTESIAN_POINT ( 'NONE',  ( 153.1499999999986414, 1.384600832570195860E-12, 6.999999999999958256 ) ) ;
#33796 = DIRECTION ( 'NONE',  ( 0.000000000000000000, -0.9826841245925227453, 0.1852887240871045060 ) ) ;
#33797 = EDGE_CURVE ( 'NONE', #16140, #39372, #31732, .T. ) ;
#33798 = CIRCLE ( 'NONE', #1056, 59.00000000000000000 ) ;
#33799 = EDGE_CURVE ( 'NONE', #28297, #23414, #2686, .T. ) ;
#33800 = EDGE_CURVE ( 'NONE', #36979, #30306, #9476, .T. ) ;
#33801 = AXIS2_PLACEMENT_3D ( 'NONE', #30146, #23622, #22756 ) ;
#33802 = ORIENTED_EDGE ( 'NONE', *, *, #24719, .F. ) ;
#33803 = AXIS2_PLACEMENT_3D ( 'NONE', #31451, #41024, #11170 ) ;
#33804 = CARTESIAN_POINT ( 'NONE',  ( 18.00000000000000000, 0.000000000000000000, -116.0000000000000000 ) ) ;
#33805 = FACE_OUTER_BOUND ( 'NONE', #21813, .T. ) ;
#33806 = CIRCLE ( 'NONE', #34524, 120.5010000000000332 ) ;
#33807 = EDGE_CURVE ( 'NONE', #26460, #16104, #42616, .T. ) ;
#33808 = EDGE_LOOP ( 'NONE', ( #42749, #17994, #5931, #11662 ) ) ;
#33809 = CARTESIAN_POINT ( 'NONE',  ( -7.547223091130065953, 40.00000000000000000, 57.33767041057931380 ) ) ;
#33810 = CYLINDRICAL_SURFACE ( 'NONE', #9640, 13.60000000000000142 ) ;
#33811 = FACE_OUTER_BOUND ( 'NONE', #27636, .T. ) ;
#33812 = VECTOR ( 'NONE', #27587, 1000.000000000000000 ) ;
#33813 = VERTEX_POINT ( 'NONE', #12766 ) ;
#33814 = VECTOR ( 'NONE', #31598, 1000.000000000000000 ) ;
#33815 = LINE ( 'NONE', #21203, #7105 ) ;
#33816 = DIRECTION ( 'NONE',  ( -1.000000000000000000, -0.000000000000000000, -0.000000000000000000 ) ) ;
#33817 = ORIENTED_EDGE ( 'NONE', *, *, #34670, .T. ) ;
#33818 = DIRECTION ( 'NONE',  ( -1.000000000000000000, 0.000000000000000000, 0.000000000000000000 ) ) ;
#33819 = EDGE_CURVE ( 'NONE', #12201, #24796, #38721, .T. ) ;
#33820 = ORIENTED_EDGE ( 'NONE', *, *, #14774, .T. ) ;
#33821 = CIRCLE ( 'NONE', #38672, 36.00000000000000000 ) ;
#33822 = DIRECTION ( 'NONE',  ( 0.000000000000000000, 0.000000000000000000, 1.000000000000000000 ) ) ;
#33823 = EDGE_LOOP ( 'NONE', ( #11908, #28536, #23884, #13670 ) ) ;
#33824 = DIRECTION ( 'NONE',  ( 0.000000000000000000, 0.000000000000000000, 1.000000000000000000 ) ) ;
#33825 = CARTESIAN_POINT ( 'NONE',  ( 17.99999999999999645, 0.000000000000000000, 0.000000000000000000 ) ) ;
#33826 = EDGE_LOOP ( 'NONE', ( #28392, #14970, #36790, #34045 ) ) ;
#33827 = DIRECTION ( 'NONE',  ( -3.009274222672345096E-17, -1.000000000000000000, 2.455023325076454960E-18 ) ) ;
#33828 = CARTESIAN_POINT ( 'NONE',  ( 17.99999999999999645, 0.000000000000000000, 0.000000000000000000 ) ) ;
#33829 = EDGE_LOOP ( 'NONE', ( #17605, #17215 ) ) ;
#33830 = DIRECTION ( 'NONE',  ( 1.000000000000000000, 0.000000000000000000, 0.000000000000000000 ) ) ;
#33831 = FACE_BOUND ( 'NONE', #32577, .T. ) ;
#33832 = CYLINDRICAL_SURFACE ( 'NONE', #16932, 59.00000000000000000 ) ;
#33833 = AXIS2_PLACEMENT_3D ( 'NONE', #34633, #8658, #4513 ) ;
#33834 = CARTESIAN_POINT ( 'NONE',  ( 17.99999999999999645, 111.9370513079675789, -44.61600100275060043 ) ) ;
#33835 = AXIS2_PLACEMENT_3D ( 'NONE', #40143, #10278, #7200 ) ;
#33836 = ADVANCED_FACE ( 'NONE', ( #39337 ), #12558, .F. ) ;
#33837 = ORIENTED_EDGE ( 'NONE', *, *, #5779, .T. ) ;
#33838 = AXIS2_PLACEMENT_3D ( 'NONE', #11077, #30907, #28086 ) ;
#33839 = CARTESIAN_POINT ( 'NONE',  ( 150.5000000000000284, 1.999999999999996669, -1.578654112981108009E-12 ) ) ;
#33840 = CARTESIAN_POINT ( 'NONE',  ( 17.99999999999999645, 25.18647942089742031, 113.2326863338528824 ) ) ;
#33841 = CARTESIAN_POINT ( 'NONE',  ( -18.51709390187839688, 31.00000000000000355, -37.54239277154294996 ) ) ;
#33842 = ORIENTED_EDGE ( 'NONE', *, *, #36026, .F. ) ;
#33843 = CIRCLE ( 'NONE', #10168, 19.11697999999999809 ) ;
#33844 = LINE ( 'NONE', #27532, #20537 ) ;
#33845 = CIRCLE ( 'NONE', #25545, 116.0000000000000000 ) ;
#33846 = CARTESIAN_POINT ( 'NONE',  ( 18.00000000000000355, 0.000000000000000000, 0.000000000000000000 ) ) ;
#33847 = ORIENTED_EDGE ( 'NONE', *, *, #31907, .T. ) ;
#33848 = CONICAL_SURFACE ( 'NONE', #8748, 2.055000000000000160, 0.7853981633974639331 ) ;
#33849 = AXIS2_PLACEMENT_3D ( 'NONE', #9502, #42854, #34285 ) ;
#33850 = DIRECTION ( 'NONE',  ( 0.000000000000000000, 0.000000000000000000, 1.000000000000000000 ) ) ;
#33851 = CARTESIAN_POINT ( 'NONE',  ( -6.238242335983215092, 40.00000000000000000, 47.40213128959678102 ) ) ;
#33852 = CARTESIAN_POINT ( 'NONE',  ( 36.58905133581346547, 40.00000000000000000, -27.97030060560320308 ) ) ;
#33853 = VECTOR ( 'NONE', #7360, 1000.000000000000114 ) ;
#33854 = ORIENTED_EDGE ( 'NONE', *, *, #34945, .T. ) ;
#33855 = CARTESIAN_POINT ( 'NONE',  ( 0.000000000000000000, -48.55277268144259040, -105.3500273609084843 ) ) ;
#33856 = CARTESIAN_POINT ( 'NONE',  ( 9.000000000000001776, 51.19683565102456413, -9.104066087302932431 ) ) ;
#33857 = ADVANCED_FACE ( 'NONE', ( #6199 ), #35854, .F. ) ;
#33858 = EDGE_CURVE ( 'NONE', #25656, #32464, #16480, .T. ) ;
#33859 = DIRECTION ( 'NONE',  ( -1.000000000000000000, 0.000000000000000000, -0.000000000000000000 ) ) ;
#33860 = FACE_OUTER_BOUND ( 'NONE', #20936, .T. ) ;
#33861 = EDGE_CURVE ( 'NONE', #40947, #41484, #15769, .T. ) ;
#33862 = VERTEX_POINT ( 'NONE', #16260 ) ;
#33863 = CARTESIAN_POINT ( 'NONE',  ( -7.231618336280544845, 40.00000000000000000, 27.02512817425793656 ) ) ;
#33864 = ORIENTED_EDGE ( 'NONE', *, *, #27769, .F. ) ;
#33865 = CARTESIAN_POINT ( 'NONE',  ( 5.991980000000000750, 0.000000000000000000, 15.08402000000000065 ) ) ;
#33866 = DIRECTION ( 'NONE',  ( -1.000000000000000000, 0.000000000000000000, 0.000000000000000000 ) ) ;
#33867 = ORIENTED_EDGE ( 'NONE', *, *, #34512, .T. ) ;
#33868 = AXIS2_PLACEMENT_3D ( 'NONE', #22917, #37025, #20276 ) ;
#33869 = DIRECTION ( 'NONE',  ( 0.000000000000000000, 0.7705132427757861446, 0.6374239897486935202 ) ) ;
#33870 = DIRECTION ( 'NONE',  ( 1.000000000000000000, 0.000000000000000000, 0.000000000000000000 ) ) ;
#33871 = ORIENTED_EDGE ( 'NONE', *, *, #18946, .F. ) ;
#33872 = DIRECTION ( 'NONE',  ( 0.000000000000000000, 0.5528000653611945259, -0.8333139190825141762 ) ) ;
#33873 = CIRCLE ( 'NONE', #29039, 120.5010000000000190 ) ;
#33874 = ORIENTED_EDGE ( 'NONE', *, *, #7321, .F. ) ;
#33875 = CIRCLE ( 'NONE', #7364, 13.59999999999999964 ) ;
#33876 = DIRECTION ( 'NONE',  ( 1.000000000000000000, 0.000000000000000000, 0.000000000000000000 ) ) ;
#33877 = EDGE_CURVE ( 'NONE', #41807, #26478, #40102, .T. ) ;
#33878 = CIRCLE ( 'NONE', #1822, 59.00000000000000711 ) ;
#33879 = ORIENTED_EDGE ( 'NONE', *, *, #38876, .T. ) ;
#33881 = ORIENTED_EDGE ( 'NONE', *, *, #21611, .F. ) ;
#33880 = DIRECTION ( 'NONE',  ( 0.000000000000000000, -0.1062934856473723155, 0.9943348002101364269 ) ) ;
#33882 = EDGE_CURVE ( 'NONE', #3612, #6418, #6407, .T. ) ;
#33883 = CARTESIAN_POINT ( 'NONE',  ( -58.00742674159663892, 31.00000000000000711, -44.63796826975934096 ) ) ;
#33884 = ORIENTED_EDGE ( 'NONE', *, *, #13909, .T. ) ;
#33885 = DIRECTION ( 'NONE',  ( 1.000000000000000000, 0.000000000000000000, 0.000000000000000000 ) ) ;
#33886 = CIRCLE ( 'NONE', #38052, 116.0000000000000000 ) ;
#33887 = ORIENTED_EDGE ( 'NONE', *, *, #8266, .F. ) ;
#33888 = DIRECTION ( 'NONE',  ( -1.000000000000000000, 0.000000000000000000, 0.000000000000000000 ) ) ;
#33889 = VECTOR ( 'NONE', #4745, 1000.000000000000000 ) ;
#33890 = VERTEX_POINT ( 'NONE', #23247 ) ;
#33891 = CARTESIAN_POINT ( 'NONE',  ( 83.51212062389942048, 39.99999999999999289, -48.08891344038907079 ) ) ;
#33893 = CARTESIAN_POINT ( 'NONE',  ( -105.9879088449591933, 31.00000000000000355, -0.3807199291576673361 ) ) ;
#33892 = DIRECTION ( 'NONE',  ( -1.000000000000000000, 0.000000000000000000, 0.000000000000000000 ) ) ;
#33894 = CIRCLE ( 'NONE', #6728, 120.5010000000000190 ) ;
#33895 = DIRECTION ( 'NONE',  ( -1.000000000000000000, -0.000000000000000000, -0.000000000000000000 ) ) ;
#33896 = ORIENTED_EDGE ( 'NONE', *, *, #16930, .F. ) ;
#33897 = LINE ( 'NONE', #37155, #30537 ) ;
#33898 = ORIENTED_EDGE ( 'NONE', *, *, #29295, .T. ) ;
#33899 =( NAMED_UNIT ( * ) SI_UNIT ( $, .STERADIAN. ) SOLID_ANGLE_UNIT ( ) );
#33900 = ORIENTED_EDGE ( 'NONE', *, *, #41893, .F. ) ;
#33901 = DIRECTION ( 'NONE',  ( 0.000000000000000000, -6.586068790149233915E-15, 1.000000000000000000 ) ) ;
#33902 = CARTESIAN_POINT ( 'NONE',  ( 80.16187752211510542, 31.00000000000000000, -27.22680903928618434 ) ) ;
#33903 = DIRECTION ( 'NONE',  ( 0.000000000000000000, 0.000000000000000000, 1.000000000000000000 ) ) ;
#33904 = ORIENTED_EDGE ( 'NONE', *, *, #1550, .T. ) ;
#33905 = AXIS2_PLACEMENT_3D ( 'NONE', #27694, #40958, #14168 ) ;
#33906 = AXIS2_PLACEMENT_3D ( 'NONE', #29963, #13171, #9661 ) ;
#33907 = DIRECTION ( 'NONE',  ( 0.000000000000000000, 0.9826841245925215240, -0.1852887240871114727 ) ) ;
#33908 = AXIS2_PLACEMENT_3D ( 'NONE', #42787, #26251, #39098 ) ;
#33909 = ORIENTED_EDGE ( 'NONE', *, *, #2057, .F. ) ;
#33910 = ORIENTED_EDGE ( 'NONE', *, *, #16069, .F. ) ;
#33911 = DIRECTION ( 'NONE',  ( -1.000000000000000000, 0.000000000000000000, -0.000000000000000000 ) ) ;
#33912 = CARTESIAN_POINT ( 'NONE',  ( -98.36195137685432144, 31.00000000000000711, 26.22212808231157055 ) ) ;
#33913 = VECTOR ( 'NONE', #7346, 1000.000000000000000 ) ;
#33914 = EDGE_CURVE ( 'NONE', #29860, #41658, #36498, .T. ) ;
#33915 = DIRECTION ( 'NONE',  ( 0.000000000000000000, 0.000000000000000000, 1.000000000000000000 ) ) ;
#33916 = EDGE_CURVE ( 'NONE', #42499, #40120, #14367, .T. ) ;
#33917 = AXIS2_PLACEMENT_3D ( 'NONE', #32273, #8716, #8943 ) ;
#33918 = VERTEX_POINT ( 'NONE', #9257 ) ;
#33919 = CARTESIAN_POINT ( 'NONE',  ( 0.000000000000000000, 22.66088087769180603, 21.87856208362564914 ) ) ;
#33920 = ORIENTED_EDGE ( 'NONE', *, *, #24174, .T. ) ;
#33921 = CARTESIAN_POINT ( 'NONE',  ( 0.000000000000000000, -120.3696465864705800, -5.624871700597306123 ) ) ;
#33922 = AXIS2_PLACEMENT_3D ( 'NONE', #13631, #30640, #918 ) ;
#33923 = CARTESIAN_POINT ( 'NONE',  ( 17.99999999999999645, -94.83915810436441518, 59.94836581341558457 ) ) ;
#33924 = FACE_OUTER_BOUND ( 'NONE', #1245, .T. ) ;
#33925 = ORIENTED_EDGE ( 'NONE', *, *, #33916, .T. ) ;
#33926 = ORIENTED_EDGE ( 'NONE', *, *, #18292, .F. ) ;
#33927 = DIRECTION ( 'NONE',  ( 0.000000000000000000, 0.000000000000000000, 1.000000000000000000 ) ) ;
#33928 = DIRECTION ( 'NONE',  ( 0.000000000000000000, -7.709882115452471264E-16, -1.000000000000000000 ) ) ;
#33929 = ADVANCED_FACE ( 'NONE', ( #36942 ), #14273, .T. ) ;
#33930 = DIRECTION ( 'NONE',  ( -1.000000000000000000, 0.000000000000000000, 0.000000000000000000 ) ) ;
#33932 = ORIENTED_EDGE ( 'NONE', *, *, #34848, .T. ) ;
#33931 = CARTESIAN_POINT ( 'NONE',  ( 17.99999999999999645, 0.6168405712486720871, 35.99471499692226928 ) ) ;
#33933 = EDGE_CURVE ( 'NONE', #8384, #4825, #34109, .T. ) ;
#33934 = CARTESIAN_POINT ( 'NONE',  ( -30.58448433907586761, 31.00000000000000355, 8.146263651248247584 ) ) ;
#33935 = CYLINDRICAL_SURFACE ( 'NONE', #704, 10.99999999999998934 ) ;
#33936 = AXIS2_PLACEMENT_3D ( 'NONE', #31733, #949, #14746 ) ;
#33938 = CARTESIAN_POINT ( 'NONE',  ( 17.99999999999999645, 0.000000000000000000, 0.000000000000000000 ) ) ;
#33937 = CARTESIAN_POINT ( 'NONE',  ( 17.99999999999999645, 31.94619804602787738, -16.59639811537323340 ) ) ;
#33939 = EDGE_LOOP ( 'NONE', ( #29765, #9404, #17617, #32414 ) ) ;
#33940 = DIRECTION ( 'NONE',  ( 0.000000000000000000, 0.000000000000000000, -1.000000000000000000 ) ) ;
#33941 = CARTESIAN_POINT ( 'NONE',  ( -51.46673615999394968, 40.00000000000000000, 6.691140578787329041 ) ) ;
#33942 = AXIS2_PLACEMENT_3D ( 'NONE', #33385, #9821, #3898 ) ;
#33943 = VECTOR ( 'NONE', #40652, 1000.000000000000000 ) ;
#33944 = DIRECTION ( 'NONE',  ( 0.000000000000000000, 0.000000000000000000, 1.000000000000000000 ) ) ;
#33945 = CIRCLE ( 'NONE', #8883, 120.5010000000000332 ) ;
#33946 = DIRECTION ( 'NONE',  ( 0.000000000000000000, 0.000000000000000000, 1.000000000000000000 ) ) ;
#33947 = ORIENTED_EDGE ( 'NONE', *, *, #18819, .T. ) ;
#33948 = CARTESIAN_POINT ( 'NONE',  ( 17.99999999999999645, 0.000000000000000000, 0.000000000000000000 ) ) ;
#33949 = EDGE_CURVE ( 'NONE', #18075, #41485, #27581, .T. ) ;
#33950 = ORIENTED_EDGE ( 'NONE', *, *, #31879, .T. ) ;
#33951 = EDGE_CURVE ( 'NONE', #41712, #21090, #6670, .T. ) ;
#33952 = DIRECTION ( 'NONE',  ( 1.000000000000000000, -0.000000000000000000, -0.000000000000000000 ) ) ;
#33953 = DIRECTION ( 'NONE',  ( 0.000000000000000000, 0.6783118362696173298, -0.7347741508630661889 ) ) ;
#33954 = AXIS2_PLACEMENT_3D ( 'NONE', #8561, #11429, #34759 ) ;
#33956 = EDGE_CURVE ( 'NONE', #17013, #909, #31077, .T. ) ;
#33955 = CARTESIAN_POINT ( 'NONE',  ( 13.71368254939966036, 31.00000000000000355, -51.22554439249349656 ) ) ;
#33957 = CARTESIAN_POINT ( 'NONE',  ( -10.00000000000000000, 0.000000000000000000, 0.000000000000000000 ) ) ;
#33958 = VERTEX_POINT ( 'NONE', #919 ) ;
#33959 = DIRECTION ( 'NONE',  ( -1.000000000000000000, -0.000000000000000000, -0.000000000000000000 ) ) ;
#33960 = ORIENTED_EDGE ( 'NONE', *, *, #19103, .F. ) ;
#33961 = CARTESIAN_POINT ( 'NONE',  ( -96.39699453480135105, 31.00000000000000711, 25.82690913164849889 ) ) ;
#33962 = VERTEX_POINT ( 'NONE', #33666 ) ;
#33963 = DIRECTION ( 'NONE',  ( -1.000000000000000000, -0.000000000000000000, -0.000000000000000000 ) ) ;
#33964 = DIRECTION ( 'NONE',  ( 1.000000000000000000, 0.000000000000000000, 0.000000000000000000 ) ) ;
#33965 = CARTESIAN_POINT ( 'NONE',  ( -56.48168293059611500, 31.00000000000000711, 43.19841958068096233 ) ) ;
#33966 = CARTESIAN_POINT ( 'NONE',  ( 50.06853320189533463, 39.99999999999999289, -56.91684085114077618 ) ) ;
#33967 = DIRECTION ( 'NONE',  ( 0.000000000000000000, 0.000000000000000000, 1.000000000000000000 ) ) ;
#33968 = AXIS2_PLACEMENT_3D ( 'NONE', #4164, #672, #41248 ) ;
#33969 = ORIENTED_EDGE ( 'NONE', *, *, #27028, .T. ) ;
#33970 = LINE ( 'NONE', #23964, #26297 ) ;
#33971 = ORIENTED_EDGE ( 'NONE', *, *, #32335, .F. ) ;
#33972 = AXIS2_PLACEMENT_3D ( 'NONE', #18948, #5377, #22220 ) ;
#33973 = LINE ( 'NONE', #30504, #16537 ) ;
#33974 = LINE ( 'NONE', #7572, #2423 ) ;
#33975 = VECTOR ( 'NONE', #30176, 1000.000000000000000 ) ;
#33977 = ORIENTED_EDGE ( 'NONE', *, *, #27583, .F. ) ;
#33976 = CARTESIAN_POINT ( 'NONE',  ( -2.649999999999789857, -150.5000000000013642, 6.999999999999585221 ) ) ;
#33978 = DIRECTION ( 'NONE',  ( -1.000000000000000000, 0.000000000000000000, -0.000000000000000000 ) ) ;
#33979 = ORIENTED_EDGE ( 'NONE', *, *, #25448, .T. ) ;
#33980 = CARTESIAN_POINT ( 'NONE',  ( 0.000000000000000000, 51.19683565102457834, -9.104066087302939536 ) ) ;
#33981 = EDGE_CURVE ( 'NONE', #41293, #11261, #7706, .T. ) ;
#33982 = CARTESIAN_POINT ( 'NONE',  ( -86.71682804797315214, 40.00000000000000711, 23.23408344657299196 ) ) ;
#33983 = CYLINDRICAL_SURFACE ( 'NONE', #36822, 59.00000000000000000 ) ;
#33984 = APPLICATION_CONTEXT ( 'automotive_design' ) ;
#33985 = AXIS2_PLACEMENT_3D ( 'NONE', #29192, #6455, #29610 ) ;
#33986 = ORIENTED_EDGE ( 'NONE', *, *, #5736, .T. ) ;
#33987 = CARTESIAN_POINT ( 'NONE',  ( 0.000000000000000000, -31.48608500567871005, 0.9019157472703476230 ) ) ;
#33988 = EDGE_CURVE ( 'NONE', #15479, #33535, #37319, .T. ) ;
#33989 = FACE_OUTER_BOUND ( 'NONE', #41750, .T. ) ;
#33990 = ORIENTED_EDGE ( 'NONE', *, *, #13436, .T. ) ;
#33991 = DIRECTION ( 'NONE',  ( 0.000000000000000000, 0.000000000000000000, -1.000000000000000000 ) ) ;
#33992 = EDGE_LOOP ( 'NONE', ( #35230, #22402, #38046, #11846 ) ) ;
#33993 = CARTESIAN_POINT ( 'NONE',  ( 17.99999999999999645, 30.78424799127077804, -6.672111855472861563 ) ) ;
#33994 = EDGE_LOOP ( 'NONE', ( #6379, #12389, #22472, #23758 ) ) ;
#33995 = CARTESIAN_POINT ( 'NONE',  ( -21.37212791037562098, 40.00000000000000000, -7.253704819186252983 ) ) ;
#33996 = DIRECTION ( 'NONE',  ( 1.000000000000000000, 0.000000000000000000, 0.000000000000000000 ) ) ;
#33997 = AXIS2_PLACEMENT_3D ( 'NONE', #12691, #42541, #8540 ) ;
#33998 = DIRECTION ( 'NONE',  ( -0.9979848074931935153, 0.000000000000000000, -0.06345332152672163162 ) ) ;
#33999 = CARTESIAN_POINT ( 'NONE',  ( 17.99999999999999645, -93.26762629039475883, 76.29967815892324268 ) ) ;
#34000 = ORIENTED_EDGE ( 'NONE', *, *, #26728, .F. ) ;
#34001 = CIRCLE ( 'NONE', #11008, 58.99999999999999289 ) ;
#34003 = CARTESIAN_POINT ( 'NONE',  ( 8.999999999999998224, 113.8630351447205697, 22.16324045874448601 ) ) ;
#34002 = DIRECTION ( 'NONE',  ( 0.000000000000000000, 0.1062934856473588541, 0.9943348002101377592 ) ) ;
#34004 = VECTOR ( 'NONE', #17207, 1000.000000000000000 ) ;
#34005 = ORIENTED_EDGE ( 'NONE', *, *, #26538, .F. ) ;
#34006 = AXIS2_PLACEMENT_3D ( 'NONE', #34534, #4646, #1370 ) ;
#34007 = CIRCLE ( 'NONE', #1951, 2.649999999999987477 ) ;
#34008 = DIRECTION ( 'NONE',  ( 0.000000000000000000, 0.000000000000000000, 1.000000000000000000 ) ) ;
#34010 = EDGE_CURVE ( 'NONE', #24871, #14972, #17882, .T. ) ;
#34009 = CARTESIAN_POINT ( 'NONE',  ( 20.96880926229634312, 31.00000000000000355, -12.11681000168150213 ) ) ;
#34011 = ORIENTED_EDGE ( 'NONE', *, *, #43064, .T. ) ;
#34012 = DIRECTION ( 'NONE',  ( 1.000000000000000000, -0.000000000000000000, -0.000000000000000000 ) ) ;
#34013 = CIRCLE ( 'NONE', #28472, 13.60000000000000142 ) ;
#34014 = DIRECTION ( 'NONE',  ( -1.000000000000000000, 0.000000000000000000, 0.000000000000000000 ) ) ;
#34015 = CARTESIAN_POINT ( 'NONE',  ( 17.99999999999999645, 0.000000000000000000, 0.000000000000000000 ) ) ;
#34016 = CARTESIAN_POINT ( 'NONE',  ( -17.60292107714122878, 31.00000000000000355, 65.74579412301164894 ) ) ;
#34017 = EDGE_LOOP ( 'NONE', ( #33014, #31315, #21044, #26332 ) ) ;
#34018 = CARTESIAN_POINT ( 'NONE',  ( -37.13421060599358725, 31.00000000000000355, -21.52932707635455500 ) ) ;
#34019 = CARTESIAN_POINT ( 'NONE',  ( 57.37208743749949491, 40.00000000000000000, 50.31438278193533620 ) ) ;
#34020 = ADVANCED_FACE ( 'NONE', ( #40853 ), #31062, .F. ) ;
#34021 = LINE ( 'NONE', #14186, #4599 ) ;
#34022 = DIRECTION ( 'NONE',  ( -1.000000000000000000, -0.000000000000000000, 0.000000000000000000 ) ) ;
#34023 = CARTESIAN_POINT ( 'NONE',  ( -31.75000000000000000, 0.000000000000000000, 0.000000000000000000 ) ) ;
#34024 = AXIS2_PLACEMENT_3D ( 'NONE', #10694, #37524, #4564 ) ;
#34025 = AXIS2_PLACEMENT_3D ( 'NONE', #8287, #31852, #1937 ) ;
#34027 = ORIENTED_EDGE ( 'NONE', *, *, #40099, .F. ) ;
#34026 = DIRECTION ( 'NONE',  ( 0.000000000000000000, 0.4610925014493267859, -0.8873520750565710991 ) ) ;
#34028 = DIRECTION ( 'NONE',  ( -3.009274222672345096E-17, -1.000000000000000000, 2.455023325076455345E-18 ) ) ;
#34029 = CARTESIAN_POINT ( 'NONE',  ( 17.99999999999999645, -79.94368240339368015, -90.16373242487986772 ) ) ;
#34030 = CIRCLE ( 'NONE', #42360, 116.0000000000000000 ) ;
#34031 = EDGE_CURVE ( 'NONE', #15847, #18339, #38038, .T. ) ;
#34032 = ORIENTED_EDGE ( 'NONE', *, *, #42224, .F. ) ;
#34033 = CARTESIAN_POINT ( 'NONE',  ( 42.30435120181500963, 40.00000000000000000, 37.09784777058769123 ) ) ;
#34034 = DIRECTION ( 'NONE',  ( 0.000000000000000000, 0.000000000000000000, 1.000000000000000000 ) ) ;
#34035 = LINE ( 'NONE', #17282, #4734 ) ;
#34036 = AXIS2_PLACEMENT_3D ( 'NONE', #29114, #9868, #23221 ) ;
#34037 = EDGE_LOOP ( 'NONE', ( #35689, #11519, #8902, #8271 ) ) ;
#34038 = ADVANCED_FACE ( 'NONE', ( #7053 ), #14500, .F. ) ;
#34039 = DIRECTION ( 'NONE',  ( -1.000000000000000000, 0.000000000000000000, -0.000000000000000000 ) ) ;
#34040 = CARTESIAN_POINT ( 'NONE',  ( 0.000000000000000000, -106.5605152861899256, -56.26142179985931335 ) ) ;
#34041 = ORIENTED_EDGE ( 'NONE', *, *, #41457, .F. ) ;
#34042 = CYLINDRICAL_SURFACE ( 'NONE', #3985, 116.0000000000000000 ) ;
#34043 = ORIENTED_EDGE ( 'NONE', *, *, #41227, .F. ) ;
#34044 = CARTESIAN_POINT ( 'NONE',  ( 18.00000000000000355, 46.11014828289831513, 9.022736828081521665 ) ) ;
#34045 = ORIENTED_EDGE ( 'NONE', *, *, #25766, .T. ) ;
#34046 = LINE ( 'NONE', #31434, #12583 ) ;
#34047 = CARTESIAN_POINT ( 'NONE',  ( -61.42214656768812375, 31.00000000000000711, 79.86467493626638259 ) ) ;
#34048 = VERTEX_POINT ( 'NONE', #30421 ) ;
#34049 = DIRECTION ( 'NONE',  ( -3.469446951953614682E-16, 1.000000000000000000, 0.000000000000000000 ) ) ;
#34050 = DIRECTION ( 'NONE',  ( -1.000000000000000000, -0.000000000000000000, -0.000000000000000000 ) ) ;
#34051 = VERTEX_POINT ( 'NONE', #36724 ) ;
#34052 = CYLINDRICAL_SURFACE ( 'NONE', #18313, 116.0000000000000000 ) ;
#34053 = CARTESIAN_POINT ( 'NONE',  ( 9.000000000000001776, -0.6505223195686603566, 51.99593080916757515 ) ) ;
#34054 = EDGE_CURVE ( 'NONE', #29146, #4036, #39978, .T. ) ;
#34056 = ADVANCED_FACE ( 'NONE', ( #10773 ), #10111, .F. ) ;
#34055 = AXIS2_PLACEMENT_3D ( 'NONE', #1509, #4341, #7631 ) ;
#34057 = AXIS2_PLACEMENT_3D ( 'NONE', #24421, #37674, #41151 ) ;
#34058 = DIRECTION ( 'NONE',  ( -1.000000000000000000, -0.000000000000000000, -0.000000000000000000 ) ) ;
#34059 = EDGE_CURVE ( 'NONE', #37862, #36952, #34552, .T. ) ;
#34060 = EDGE_CURVE ( 'NONE', #16003, #10495, #30641, .T. ) ;
#34061 = CYLINDRICAL_SURFACE ( 'NONE', #42332, 59.00000000000000000 ) ;
#34062 = AXIS2_PLACEMENT_3D ( 'NONE', #38469, #32580, #2662 ) ;
#34063 = EDGE_LOOP ( 'NONE', ( #42574, #38078, #2661, #3186, #2079, #28319, #11468, #32999, #10338, #10440, #31981, #21338, #41585, #27505, #25805, #19293, #32919, #36218, #39765, #12058, #27623, #27615, #12820, #28072, #18701, #19833, #43177, #31223, #17768, #29616, #27291, #17837, #7147, #1662, #30211, #16684, #26351, #30855, #26262, #16901, #8347, #1349, #12348, #3109, #26732, #32634, #10249, #39971, #12335, #43161, #37569, #26698, #1301, #17953, #37369, #8171, #26696, #25339, #16337, #648, #26595, #11696, #21236, #28388, #12807, #31686, #3628, #36095, #2819, #18810, #723, #9287, #20724, #10214, #39649, #635, #34940, #13573, #19073, #8760, #455, #36501, #35147, #23790, #29232, #33896, #6163, #5271, #25099, #11432, #6358, #21927, #89, #9362, #37996, #38242, #37895, #16608, #36050, #9198, #31480, #27330, #31501, #27499, #22100, #15018, #2462, #16062, #8067, #4096, #35602, #4611, #27823, #23876, #27949, #29909, #1571, #7658, #32029, #5459, #16150, #7359, #1695, #26633, #26250, #14837, #26564, #27959, #23723, #32875, #16300, #42644, #24365, #15544, #23112, #14591, #9397, #12808, #27310, #14848, #33001 ) ) ;
#34064 = DIRECTION ( 'NONE',  ( -1.110223024625156540E-16, -0.9999999999999997780, 5.551115123125782702E-17 ) ) ;
#34065 = CARTESIAN_POINT ( 'NONE',  ( 0.000000000000000000, 46.11014828289831513, 9.022736828081521665 ) ) ;
#34066 = CARTESIAN_POINT ( 'NONE',  ( 28.83751338862256119, 31.00000000000000355, -32.88701605462710376 ) ) ;
#34067 = ORIENTED_EDGE ( 'NONE', *, *, #662, .T. ) ;
#34069 = CARTESIAN_POINT ( 'NONE',  ( 17.99999999999999645, 21.55123232222629426, -118.5581519187670096 ) ) ;
#34068 = CARTESIAN_POINT ( 'NONE',  ( 17.99999999999999645, 0.000000000000000000, 0.000000000000000000 ) ) ;
#34070 = DIRECTION ( 'NONE',  ( 1.000000000000000000, 0.000000000000000000, 0.000000000000000000 ) ) ;
#34071 = EDGE_LOOP ( 'NONE', ( #16922, #2574, #13156, #18660 ) ) ;
#34072 = DIRECTION ( 'NONE',  ( 0.000000000000000000, 0.7705132427757904745, -0.6374239897486881912 ) ) ;
#34073 = CARTESIAN_POINT ( 'NONE',  ( -38.53741714288415210, 40.00000000000000000, -33.79371401777069650 ) ) ;
#34074 = CARTESIAN_POINT ( 'NONE',  ( 36.84045577241590763, 40.00000000000000000, -41.86038302679909151 ) ) ;
#34075 = DIRECTION ( 'NONE',  ( -1.000000000000000000, -0.000000000000000000, -0.000000000000000000 ) ) ;
#34076 = CYLINDRICAL_SURFACE ( 'NONE', #17985, 116.0000000000000000 ) ;
#34077 = DIRECTION ( 'NONE',  ( 0.000000000000000000, 0.000000000000000000, 1.000000000000000000 ) ) ;
#34078 = DIRECTION ( 'NONE',  ( -1.000000000000000000, 0.000000000000000000, 0.000000000000000000 ) ) ;
#34079 = ORIENTED_EDGE ( 'NONE', *, *, #13074, .F. ) ;
#34080 = CARTESIAN_POINT ( 'NONE',  ( 20.96880926229634312, 40.00000000000000000, -12.11681000168150213 ) ) ;
#34081 = ORIENTED_EDGE ( 'NONE', *, *, #29004, .F. ) ;
#34082 = DIRECTION ( 'NONE',  ( 0.000000000000000000, 0.000000000000000000, -1.000000000000000000 ) ) ;
#34083 = DIRECTION ( 'NONE',  ( -1.000000000000000000, -0.000000000000000000, -0.000000000000000000 ) ) ;
#34084 = EDGE_LOOP ( 'NONE', ( #27494, #23924, #18756, #1813 ) ) ;
#34085 = ADVANCED_FACE ( 'NONE', ( #260 ), #37378, .F. ) ;
#34086 = CIRCLE ( 'NONE', #23658, 20.00000000000000355 ) ;
#34087 = VECTOR ( 'NONE', #29953, 1000.000000000000000 ) ;
#34088 = DIRECTION ( 'NONE',  ( 0.000000000000000000, 0.3140767120219427611, 0.9493976084683832806 ) ) ;
#34089 = CARTESIAN_POINT ( 'NONE',  ( 0.000000000000000000, 0.000000000000000000, 0.000000000000000000 ) ) ;
#34090 = EDGE_LOOP ( 'NONE', ( #43068, #35430, #35504, #34879 ) ) ;
#34091 = DIRECTION ( 'NONE',  ( 0.000000000000000000, 0.000000000000000000, 1.000000000000000000 ) ) ;
#34092 = VERTEX_POINT ( 'NONE', #20406 ) ;
#34093 = CIRCLE ( 'NONE', #35459, 13.60000000000000320 ) ;
#34094 = DIRECTION ( 'NONE',  ( 1.000000000000000000, 0.000000000000000000, -6.546126324440850663E-16 ) ) ;
#34095 = ORIENTED_EDGE ( 'NONE', *, *, #39601, .T. ) ;
#34097 = ORIENTED_EDGE ( 'NONE', *, *, #21796, .F. ) ;
#34096 = CARTESIAN_POINT ( 'NONE',  ( 17.99999999999999645, 13.22719389142019608, -28.58720592780581882 ) ) ;
#34098 = CARTESIAN_POINT ( 'NONE',  ( 69.81317433577432041, 31.00000000000000000, 34.54326205989952570 ) ) ;
#34099 = ORIENTED_EDGE ( 'NONE', *, *, #32598, .T. ) ;
#34100 = CARTESIAN_POINT ( 'NONE',  ( 18.00000000000000355, -43.55304910509425298, 28.41006711799970219 ) ) ;
#34101 = ORIENTED_EDGE ( 'NONE', *, *, #25179, .F. ) ;
#34102 = FACE_OUTER_BOUND ( 'NONE', #30575, .T. ) ;
#34103 = ORIENTED_EDGE ( 'NONE', *, *, #14006, .F. ) ;
#34104 = CARTESIAN_POINT ( 'NONE',  ( 42.30527206516848793, 40.00000000000000000, -85.53883208674149330 ) ) ;
#34106 = DIRECTION ( 'NONE',  ( 1.000000000000000000, 0.000000000000000000, 0.000000000000000000 ) ) ;
#34105 = DIRECTION ( 'NONE',  ( 1.000000000000000000, 1.836909530733573776E-16, 0.000000000000000000 ) ) ;
#34107 = EDGE_CURVE ( 'NONE', #4975, #27337, #19267, .T. ) ;
#34108 = EDGE_CURVE ( 'NONE', #16960, #8432, #11561, .T. ) ;
#34109 = LINE ( 'NONE', #17785, #363 ) ;
#34110 = CARTESIAN_POINT ( 'NONE',  ( 17.99999999999999645, 2.418575551222434949, -120.4767259403368911 ) ) ;
#34111 = EDGE_LOOP ( 'NONE', ( #32056, #28105 ) ) ;
#34112 =( NAMED_UNIT ( * ) SI_UNIT ( $, .STERADIAN. ) SOLID_ANGLE_UNIT ( ) );
#34113 = EDGE_CURVE ( 'NONE', #23617, #14608, #18437, .T. ) ;
#34114 = DIRECTION ( 'NONE',  ( 0.000000000000000000, 0.000000000000000000, 1.000000000000000000 ) ) ;
#34115 = AXIS2_PLACEMENT_3D ( 'NONE', #5945, #16022, #22367 ) ;
#34116 = CARTESIAN_POINT ( 'NONE',  ( 0.000000000000000000, 24.70533337038223110, 26.18485254986702060 ) ) ;
#34117 = CARTESIAN_POINT ( 'NONE',  ( 81.87674480462379734, 31.00000000000000000, -21.93767060400471891 ) ) ;
#34118 = VECTOR ( 'NONE', #9884, 1000.000000000000000 ) ;
#34119 = CARTESIAN_POINT ( 'NONE',  ( -0.1410422978106123659, 4.700232962125094893, -3.687027686973624707 ) ) ;
#34120 = ORIENTED_EDGE ( 'NONE', *, *, #10319, .F. ) ;
#34121 = CARTESIAN_POINT ( 'NONE',  ( -22.06642698273767067, 40.00000000000000000, -2.901557744773887393 ) ) ;
#34122 = ORIENTED_EDGE ( 'NONE', *, *, #23701, .T. ) ;
#34123 = EDGE_CURVE ( 'NONE', #23473, #31625, #3846, .T. ) ;
#34124 = ORIENTED_EDGE ( 'NONE', *, *, #5330, .T. ) ;
#34125 = CARTESIAN_POINT ( 'NONE',  ( 0.000000000000000000, 100.6739960869724655, -49.52796165323157851 ) ) ;
#34126 = CARTESIAN_POINT ( 'NONE',  ( 17.99999999999999645, -78.75547124681308730, -91.20343606297076633 ) ) ;
#34127 = DIRECTION ( 'NONE',  ( -1.000000000000000000, 0.000000000000000000, 0.000000000000000000 ) ) ;
#34128 = EDGE_LOOP ( 'NONE', ( #16349, #38375, #30157, #25144 ) ) ;
#34129 = DIRECTION ( 'NONE',  ( 0.000000000000000000, -0.9407002666710296834, -0.3392388661180399945 ) ) ;
#34130 = ORIENTED_EDGE ( 'NONE', *, *, #36701, .T. ) ;
#34131 = CARTESIAN_POINT ( 'NONE',  ( 9.000000000000001776, 52.88069566989454273, 103.2454939717370905 ) ) ;
#34132 = CARTESIAN_POINT ( 'NONE',  ( 0.000000000000000000, 0.000000000000000000, 0.000000000000000000 ) ) ;
#34133 = CARTESIAN_POINT ( 'NONE',  ( 0.000000000000000000, 0.000000000000000000, 0.000000000000000000 ) ) ;
#34134 = CYLINDRICAL_SURFACE ( 'NONE', #15020, 36.00000000000000000 ) ;
#34135 = VERTEX_POINT ( 'NONE', #14719 ) ;
#34136 = EDGE_CURVE ( 'NONE', #39574, #24001, #5283, .T. ) ;
#34137 = ORIENTED_EDGE ( 'NONE', *, *, #4407, .T. ) ;
#34138 = CARTESIAN_POINT ( 'NONE',  ( 17.99999999999999645, 25.52601536738619714, -19.21447964122670626 ) ) ;
#34139 = DIRECTION ( 'NONE',  ( 0.000000000000000000, 0.000000000000000000, 1.000000000000000000 ) ) ;
#34140 = DIRECTION ( 'NONE',  ( 0.000000000000000000, -0.2113826236296114103, -0.9774033898178695612 ) ) ;
#34141 = ORIENTED_EDGE ( 'NONE', *, *, #3322, .T. ) ;
#34143 = EDGE_LOOP ( 'NONE', ( #9971, #2125, #11689, #34445 ) ) ;
#34142 = CARTESIAN_POINT ( 'NONE',  ( 17.99999999999999645, -57.69704296431255131, 105.7900857083227777 ) ) ;
#34144 = AXIS2_PLACEMENT_3D ( 'NONE', #33741, #3829, #20703 ) ;
#34145 = CARTESIAN_POINT ( 'NONE',  ( -24.78443185005114557, 31.00000000000000355, 32.19086620116432584 ) ) ;
#34146 = DIRECTION ( 'NONE',  ( -1.000000000000000000, -0.000000000000000000, 0.000000000000000000 ) ) ;
#34148 = ORIENTED_EDGE ( 'NONE', *, *, #35560, .T. ) ;
#34147 = CARTESIAN_POINT ( 'NONE',  ( 17.99999999999999645, -28.35267316522800130, 22.18391138608698299 ) ) ;
#34149 = VERTEX_POINT ( 'NONE', #15366 ) ;
#34150 = CARTESIAN_POINT ( 'NONE',  ( 32.82854187708761629, 40.00000000000000000, -56.64543409044760125 ) ) ;
#34151 = DIRECTION ( 'NONE',  ( 0.000000000000000000, -2.928448444191355855E-14, -1.000000000000000000 ) ) ;
#34152 = ADVANCED_FACE ( 'NONE', ( #11219 ), #41931, .T. ) ;
#34153 = DIRECTION ( 'NONE',  ( 0.000000000000000000, 0.9213119778704139673, -0.3888241754733182676 ) ) ;
#34154 = ORIENTED_EDGE ( 'NONE', *, *, #27421, .T. ) ;
#34155 = DIRECTION ( 'NONE',  ( 0.000000000000000000, 0.000000000000000000, 1.000000000000000000 ) ) ;
#34156 = ORIENTED_EDGE ( 'NONE', *, *, #37737, .T. ) ;
#34157 = DIRECTION ( 'NONE',  ( 0.000000000000000000, 0.000000000000000000, -1.000000000000000000 ) ) ;
#34158 = LINE ( 'NONE', #10400, #27610 ) ;
#34159 = AXIS2_PLACEMENT_3D ( 'NONE', #26826, #36846, #36404 ) ;
#34160 = CARTESIAN_POINT ( 'NONE',  ( 14.80739997004469366, 31.00000000000000355, 55.25628696611591550 ) ) ;
#34161 = DIRECTION ( 'NONE',  ( -0.3806385939525924744, 0.000000000000000000, 0.9247238835424298475 ) ) ;
#34162 = EDGE_LOOP ( 'NONE', ( #37823, #41311, #37191, #42514 ) ) ;
#34163 = ADVANCED_FACE ( 'NONE', ( #12081 ), #38240, .F. ) ;
#34164 = CIRCLE ( 'NONE', #23062, 20.00000000000001066 ) ;
#34165 = EDGE_CURVE ( 'NONE', #32706, #33033, #31769, .T. ) ;
#34166 = FACE_OUTER_BOUND ( 'NONE', #23427, .T. ) ;
#34167 = EDGE_LOOP ( 'NONE', ( #5973, #24197, #26939, #19307 ) ) ;
#34168 = CARTESIAN_POINT ( 'NONE',  ( -19.19493090124598922, 40.00000000000000000, -25.00897302100653263 ) ) ;
#34169 = CIRCLE ( 'NONE', #15405, 116.0000000000000000 ) ;
#34170 = AXIS2_PLACEMENT_3D ( 'NONE', #22438, #5806, #2512 ) ;
#34171 = EDGE_CURVE ( 'NONE', #10833, #34610, #12958, .T. ) ;
#34172 = VERTEX_POINT ( 'NONE', #11430 ) ;
#34173 = FACE_OUTER_BOUND ( 'NONE', #7913, .T. ) ;
#34174 = AXIS2_PLACEMENT_3D ( 'NONE', #27040, #3436, #149 ) ;
#34175 = LINE ( 'NONE', #1871, #21381 ) ;
#34176 = CARTESIAN_POINT ( 'NONE',  ( -43.11175393642376008, 31.00000000000000355, 56.02072642018850246 ) ) ;
#34177 = CARTESIAN_POINT ( 'NONE',  ( 24.27443280711675655, 40.00000000000000000, -71.15176282235543681 ) ) ;
#34178 = AXIS2_PLACEMENT_3D ( 'NONE', #10469, #7409, #10919 ) ;
#34179 = CYLINDRICAL_SURFACE ( 'NONE', #39688, 31.49899999999999878 ) ;
#34180 = ORIENTED_EDGE ( 'NONE', *, *, #7020, .T. ) ;
#34181 = DIRECTION ( 'NONE',  ( 0.000000000000000000, -0.6845471059286950544, 0.7289686274214053352 ) ) ;
#34182 = ORIENTED_EDGE ( 'NONE', *, *, #36396, .F. ) ;
#34183 = FACE_OUTER_BOUND ( 'NONE', #32931, .T. ) ;
#34184 = DIRECTION ( 'NONE',  ( 0.000000000000000000, 0.000000000000000000, 1.000000000000000000 ) ) ;
#34186 = VERTEX_POINT ( 'NONE', #2010 ) ;
#34185 = CARTESIAN_POINT ( 'NONE',  ( -10.00000000000000000, 0.000000000000000000, 0.000000000000000000 ) ) ;
#34187 = CARTESIAN_POINT ( 'NONE',  ( 9.000000000000001776, -111.2559044912527355, 32.83479428644638887 ) ) ;
#34188 = ORIENTED_EDGE ( 'NONE', *, *, #35668, .T. ) ;
#34189 = DIRECTION ( 'NONE',  ( -1.000000000000000000, 0.000000000000000000, 0.000000000000000000 ) ) ;
#34190 = CARTESIAN_POINT ( 'NONE',  ( 28.03234818517180216, 40.00000000000000000, 82.53419278363811884 ) ) ;
#34191 = DIRECTION ( 'NONE',  ( 0.000000000000000000, 0.000000000000000000, 1.000000000000000000 ) ) ;
#34192 = EDGE_CURVE ( 'NONE', #27469, #33113, #42881, .T. ) ;
#34193 = ORIENTED_EDGE ( 'NONE', *, *, #33658, .F. ) ;
#34194 = AXIS2_PLACEMENT_3D ( 'NONE', #611, #14619, #823 ) ;
#34195 = CYLINDRICAL_SURFACE ( 'NONE', #24176, 4.250000000000000000 ) ;
#34196 = CARTESIAN_POINT ( 'NONE',  ( -150.5000000000000284, -5.254679414958916394E-13, 6.999999999999998224 ) ) ;
#34197 = ORIENTED_EDGE ( 'NONE', *, *, #4165, .T. ) ;
#34198 = AXIS2_PLACEMENT_3D ( 'NONE', #9478, #22830, #25877 ) ;
#34199 = FACE_OUTER_BOUND ( 'NONE', #31929, .T. ) ;
#34200 = EDGE_LOOP ( 'NONE', ( #25544, #8057, #1048, #37041 ) ) ;
#34201 = CARTESIAN_POINT ( 'NONE',  ( 103.7695705685757019, -106.4195705685758213, 9.999999999999671374 ) ) ;
#34203 = VERTEX_POINT ( 'NONE', #22141 ) ;
#34202 = AXIS2_PLACEMENT_3D ( 'NONE', #9689, #2250, #42609 ) ;
#34204 = CARTESIAN_POINT ( 'NONE',  ( 25.29542371717657545, 40.00000000000000000, 28.93716311999360613 ) ) ;
#34205 = DIRECTION ( 'NONE',  ( -3.996523416598930318E-16, 2.658563593772947863E-15, 1.000000000000000000 ) ) ;
#34206 = VECTOR ( 'NONE', #14920, 1000.000000000000000 ) ;
#34207 = CARTESIAN_POINT ( 'NONE',  ( 9.000000000000001776, 101.8011932243948081, 55.61040422519366189 ) ) ;
#34208 = VECTOR ( 'NONE', #22920, 1000.000000000000000 ) ;
#34209 = CARTESIAN_POINT ( 'NONE',  ( 0.000000000000000000, 111.2721026680460596, -14.38025178762657852 ) ) ;
#34210 = ORIENTED_EDGE ( 'NONE', *, *, #16477, .T. ) ;
#34212 = CARTESIAN_POINT ( 'NONE',  ( 18.00000000000000355, -47.32430374665946715, 21.55018039121508977 ) ) ;
#34211 = CARTESIAN_POINT ( 'NONE',  ( 106.4195705685741302, 106.4195705685767166, 10.00000000000000000 ) ) ;
#34213 = EDGE_CURVE ( 'NONE', #21728, #40564, #35398, .T. ) ;
#34214 = ORIENTED_EDGE ( 'NONE', *, *, #5596, .T. ) ;
#34215 = AXIS2_PLACEMENT_3D ( 'NONE', #30101, #29896, #381 ) ;
#34216 = LINE ( 'NONE', #6736, #19685 ) ;
#34217 = CARTESIAN_POINT ( 'NONE',  ( 15.62097837807030842, 31.00000000000000355, -17.81927981957692353 ) ) ;
#34218 = ORIENTED_EDGE ( 'NONE', *, *, #4301, .F. ) ;
#34219 = DIRECTION ( 'NONE',  ( -1.000000000000000000, -0.000000000000000000, 0.000000000000000000 ) ) ;
#34220 = VECTOR ( 'NONE', #29304, 1000.000000000000000 ) ;
#34221 = DIRECTION ( 'NONE',  ( -1.000000000000000000, -0.000000000000000000, -0.000000000000000000 ) ) ;
#34222 = CONTEXT_DEPENDENT_SHAPE_REPRESENTATION ( #34547, #24987 ) ;
#34223 = EDGE_CURVE ( 'NONE', #19720, #35293, #38443, .T. ) ;
#34224 = CARTESIAN_POINT ( 'NONE',  ( 0.000000000000000000, 72.00556975657821113, -86.04342158279314390 ) ) ;
#34225 = CARTESIAN_POINT ( 'NONE',  ( -67.35649507452052376, 31.00000000000000711, 18.04843207638801772 ) ) ;
#34226 = ORIENTED_EDGE ( 'NONE', *, *, #41178, .F. ) ;
#34227 = CARTESIAN_POINT ( 'NONE',  ( -14.09736097164098823, 31.00000000000000355, -41.75563764759219509 ) ) ;
#34228 = EDGE_CURVE ( 'NONE', #42811, #26205, #32130, .T. ) ;
#34229 = CARTESIAN_POINT ( 'NONE',  ( -77.03666156126601550, 40.00000000000000711, 20.64125776147949409 ) ) ;
#34230 = CARTESIAN_POINT ( 'NONE',  ( 17.99999999999999645, 0.000000000000000000, 0.000000000000000000 ) ) ;
#34231 = CIRCLE ( 'NONE', #23803, 116.0000000000000000 ) ;
#34232 = LINE ( 'NONE', #1054, #24996 ) ;
#34233 = DIRECTION ( 'NONE',  ( -1.000000000000000000, 0.000000000000000000, 0.000000000000000000 ) ) ;
#34234 = AXIS2_PLACEMENT_3D ( 'NONE', #3576, #39802, #33927 ) ;
#34236 = ORIENTED_EDGE ( 'NONE', *, *, #4360, .F. ) ;
#34235 = CARTESIAN_POINT ( 'NONE',  ( 17.99999999999999645, 0.000000000000000000, 0.000000000000000000 ) ) ;
#34237 = LINE ( 'NONE', #38366, #13542 ) ;
#34238 = LINE ( 'NONE', #39899, #15414 ) ;
#34239 = ORIENTED_EDGE ( 'NONE', *, *, #34293, .F. ) ;
#34240 = CARTESIAN_POINT ( 'NONE',  ( 52.83624534446448706, 40.00000000000000000, -14.15919354876300318 ) ) ;
#34241 = DIRECTION ( 'NONE',  ( -1.000000000000000000, -0.000000000000000000, 0.000000000000000000 ) ) ;
#34243 = EDGE_CURVE ( 'NONE', #21049, #24569, #22083, .T. ) ;
#34242 = FACE_OUTER_BOUND ( 'NONE', #33939, .T. ) ;
#34244 = CIRCLE ( 'NONE', #32164, 58.99999999999999289 ) ;
#34245 = EDGE_LOOP ( 'NONE', ( #31726, #40617, #35531, #36727, #21718, #36844, #3718, #5197, #27758, #3283, #22442, #8132, #9646, #15090, #18782, #14209, #33393, #41609, #4234, #21786, #2289, #16795, #2374, #23880, #30100, #19186, #36181, #19745, #31739, #39932, #39860, #395, #10330, #19009, #21202, #10806, #34381, #13772, #3296, #17256, #40737, #29259, #37536, #30267, #14309, #5424, #11349, #1322, #24713, #451, #11563, #7540, #8477, #33085, #38696, #8488, #1117, #31944, #29705, #32021, #22683, #25243, #1296, #18633, #35356, #22542, #851, #28101, #11546, #18817, #38674, #36484, #42694, #19548, #26370, #31215, #31761, #27154, #6986, #3339, #31128, #8232, #39138, #39589, #34991, #14253, #20220, #11478, #38101, #37439, #26, #32389, #22748, #12530, #23912, #25899, #11881, #20635, #1718, #29549, #31031, #15646, #33173, #34103, #25386, #13316, #18702, #39535, #18965, #28354, #33802, #14542, #10101, #16804, #22596, #15040, #19719, #37874, #42106, #35485, #12327, #15408, #7634, #6588, #18208, #35929, #42110, #9151, #22612, #2854, #24541, #27640, #41515, #471, #37675, #22560, #3766, #42350, #4800, #12736, #4155 ) ) ;
#34246 = EDGE_CURVE ( 'NONE', #18842, #10311, #38752, .T. ) ;
#34247 = CARTESIAN_POINT ( 'NONE',  ( 18.00000000000000355, 27.43636312076321104, 38.14186064215159888 ) ) ;
#34248 = CARTESIAN_POINT ( 'NONE',  ( 18.00000000000000355, -27.79676263918163315, -37.88001506494799031 ) ) ;
#34249 = ORIENTED_EDGE ( 'NONE', *, *, #23817, .F. ) ;
#34250 = FACE_OUTER_BOUND ( 'NONE', #13028, .T. ) ;
#34251 = ORIENTED_EDGE ( 'NONE', *, *, #41715, .T. ) ;
#34252 = DIRECTION ( 'NONE',  ( 0.000000000000000000, -0.7164567402983066380, -0.6976315211349934930 ) ) ;
#34253 = EDGE_LOOP ( 'NONE', ( #4524, #38177, #5346, #13230 ) ) ;
#34254 = DIRECTION ( 'NONE',  ( -1.000000000000000000, -0.000000000000000000, 0.000000000000000000 ) ) ;
#34255 = CARTESIAN_POINT ( 'NONE',  ( -87.85203729257557370, 31.00000000000000711, 50.59313708110082786 ) ) ;
#34256 = ORIENTED_EDGE ( 'NONE', *, *, #32169, .T. ) ;
#34257 = DIRECTION ( 'NONE',  ( -1.000000000000000000, 0.000000000000000000, -0.000000000000000000 ) ) ;
#34258 = DIRECTION ( 'NONE',  ( -1.000000000000000000, -0.000000000000000000, 0.000000000000000000 ) ) ;
#34259 = VERTEX_POINT ( 'NONE', #31285 ) ;
#34260 = FACE_OUTER_BOUND ( 'NONE', #33236, .T. ) ;
#34261 = EDGE_CURVE ( 'NONE', #13842, #36952, #21716, .T. ) ;
#34262 = TOROIDAL_SURFACE ( 'NONE', #15492, 19.59999999999999076, 0.4000000000000001887 ) ;
#34263 = AXIS2_PLACEMENT_3D ( 'NONE', #39815, #35900, #15887 ) ;
#34264 = CARTESIAN_POINT ( 'NONE',  ( 106.4195705685734623, 106.4195705685780524, 7.000000000000250466 ) ) ;
#34265 = CARTESIAN_POINT ( 'NONE',  ( 17.99999999999999645, 92.10690493017060021, 64.06707842432207656 ) ) ;
#34266 = VECTOR ( 'NONE', #4340, 1000.000000000000000 ) ;
#34267 = CARTESIAN_POINT ( 'NONE',  ( 17.99999999999999645, -106.5605152861899256, -56.26142179985931335 ) ) ;
#34268 = ORIENTED_EDGE ( 'NONE', *, *, #30745, .F. ) ;
#34269 = CARTESIAN_POINT ( 'NONE',  ( 0.000000000000000000, 0.000000000000000000, 0.000000000000000000 ) ) ;
#34270 = EDGE_CURVE ( 'NONE', #42728, #5490, #13714, .T. ) ;
#34271 = DIRECTION ( 'NONE',  ( -1.000000000000000000, 0.000000000000000000, 0.000000000000000000 ) ) ;
#34272 = CARTESIAN_POINT ( 'NONE',  ( -16.93500259178182432, 31.00000000000000355, 34.36424406943201149 ) ) ;
#34273 = CIRCLE ( 'NONE', #15505, 36.00000000000000000 ) ;
#34274 = ORIENTED_EDGE ( 'NONE', *, *, #8893, .T. ) ;
#34276 = CARTESIAN_POINT ( 'NONE',  ( 0.000000000000000000, 19.69434969228107946, -24.58291258574028504 ) ) ;
#34275 = DIRECTION ( 'NONE',  ( 0.000000000000000000, 0.000000000000000000, 1.000000000000000000 ) ) ;
#34277 = EDGE_CURVE ( 'NONE', #23398, #21330, #7391, .T. ) ;
#34278 = CARTESIAN_POINT ( 'NONE',  ( 17.99999999999999645, 107.2703412112699368, -32.88383143828351507 ) ) ;
#34279 = VERTEX_POINT ( 'NONE', #1582 ) ;
#34280 = DIRECTION ( 'NONE',  ( -1.000000000000000000, 0.000000000000000000, -0.000000000000000000 ) ) ;
#34281 = CARTESIAN_POINT ( 'NONE',  ( 32.65420139560029611, 40.00000000000000000, -42.57517516360295673 ) ) ;
#34282 = CARTESIAN_POINT ( 'NONE',  ( 14.32751628686350287, 40.00000000000000000, -53.13354968558886071 ) ) ;
#34283 = DIRECTION ( 'NONE',  ( 0.000000000000000000, 0.9714298932647090767, 0.2373266998711184850 ) ) ;
#34284 = DIRECTION ( 'NONE',  ( 0.000000000000000000, -0.9714298932647122964, 0.2373266998711056064 ) ) ;
#34285 = DIRECTION ( 'NONE',  ( 0.000000000000000000, -5.351180891996252112E-15, -1.000000000000000000 ) ) ;
#34286 = CARTESIAN_POINT ( 'NONE',  ( 0.000000000000000000, 0.000000000000000000, -4.974599999999998801 ) ) ;
#34287 = VECTOR ( 'NONE', #2790, 1000.000000000000000 ) ;
#34288 = EDGE_LOOP ( 'NONE', ( #22898, #20554, #24931, #18358 ) ) ;
#34289 = CARTESIAN_POINT ( 'NONE',  ( 11.68784703496123711, 40.00000000000000000, -20.25319168173327355 ) ) ;
#34290 = ORIENTED_EDGE ( 'NONE', *, *, #19464, .T. ) ;
#34291 = DIRECTION ( 'NONE',  ( 0.000000000000000000, 0.000000000000000000, 1.000000000000000000 ) ) ;
#34292 = CARTESIAN_POINT ( 'NONE',  ( -1.243802165048909503, 3.900692638707381921, -3.223146290109805800 ) ) ;
#34293 = EDGE_CURVE ( 'NONE', #37232, #30500, #31804, .T. ) ;
#34294 = VERTEX_POINT ( 'NONE', #13749 ) ;
#34295 = EDGE_CURVE ( 'NONE', #37603, #4177, #10193, .T. ) ;
#34296 = CARTESIAN_POINT ( 'NONE',  ( 17.99999999999999645, -76.48293397876315680, 82.08917884620285577 ) ) ;
#34297 = EDGE_CURVE ( 'NONE', #5537, #19539, #14399, .T. ) ;
#34298 = EDGE_CURVE ( 'NONE', #2582, #32160, #3225, .T. ) ;
#34299 = AXIS2_PLACEMENT_3D ( 'NONE', #42930, #9575, #5855 ) ;
#34300 = CARTESIAN_POINT ( 'NONE',  ( 0.000000000000000000, 18.42432724429518487, -30.92804820215982531 ) ) ;
#34301 = ORIENTED_EDGE ( 'NONE', *, *, #40703, .T. ) ;
#34302 = DIRECTION ( 'NONE',  ( -1.000000000000000000, -0.000000000000000000, 0.000000000000000000 ) ) ;
#34303 = ORIENTED_EDGE ( 'NONE', *, *, #33642, .T. ) ;
#34304 = AXIS2_PLACEMENT_3D ( 'NONE', #15953, #12877, #8727 ) ;
#34305 = VERTEX_POINT ( 'NONE', #10229 ) ;
#34307 = ORIENTED_EDGE ( 'NONE', *, *, #38521, .F. ) ;
#34306 = DIRECTION ( 'NONE',  ( 0.000000000000000000, 0.000000000000000000, 1.000000000000000000 ) ) ;
#34308 = CARTESIAN_POINT ( 'NONE',  ( -71.90006454728114704, 31.00000000000000711, 4.599370544632132685 ) ) ;
#34309 = ORIENTED_EDGE ( 'NONE', *, *, #24227, .T. ) ;
#34310 = DIRECTION ( 'NONE',  ( 0.000000000000000000, 0.000000000000000000, 1.000000000000000000 ) ) ;
#34311 = B_SPLINE_CURVE_WITH_KNOTS ( 'NONE', 3,
 ( #37704, #32039, #2123, #7823, #17914, #31189 ),
 .UNSPECIFIED., .F., .F.,
 ( 4, 2, 4 ),
 ( 0.003358874760055551890, 0.004541967308452098118, 0.005725059856848645212 ),
 .UNSPECIFIED. ) ;
#34312 = EDGE_LOOP ( 'NONE', ( #32470, #11537, #7197, #22646 ) ) ;
#34313 = CARTESIAN_POINT ( 'NONE',  ( 17.99999999999999645, 37.07968990261625208, -109.9140418541953750 ) ) ;
#34314 = VERTEX_POINT ( 'NONE', #40320 ) ;
#34315 = CARTESIAN_POINT ( 'NONE',  ( -12.22491041697691294, 40.00000000000000000, -93.69500887688228374 ) ) ;
#34317 = CARTESIAN_POINT ( 'NONE',  ( 0.000000000000000000, 117.9424311864592312, -24.69967462998914698 ) ) ;
#34316 = DIRECTION ( 'NONE',  ( 1.000000000000000000, 0.000000000000000000, 0.000000000000000000 ) ) ;
#34318 = CARTESIAN_POINT ( 'NONE',  ( 17.99999999999999645, 0.000000000000000000, 0.000000000000000000 ) ) ;
#34319 = FACE_OUTER_BOUND ( 'NONE', #2086, .T. ) ;
#34320 = ORIENTED_EDGE ( 'NONE', *, *, #3957, .T. ) ;
#34321 = EDGE_CURVE ( 'NONE', #26486, #10423, #30429, .T. ) ;
#34322 = CIRCLE ( 'NONE', #14862, 2.649999999999957723 ) ;
#34323 = CARTESIAN_POINT ( 'NONE',  ( 17.99999999999999645, -14.84191762912296930, -27.78316904333141224 ) ) ;
#34324 = VERTEX_POINT ( 'NONE', #26611 ) ;
#34325 = CARTESIAN_POINT ( 'NONE',  ( -5.639656061357299244, -10.48075544252182922, 0.000000000000000000 ) ) ;
#34326 = CARTESIAN_POINT ( 'NONE',  ( 64.90595555533579386, 31.00000000000000000, 56.92265028768127166 ) ) ;
#34327 = ADVANCED_FACE ( 'NONE', ( #25616 ), #3448, .F. ) ;
#34328 = DIRECTION ( 'NONE',  ( -1.000000000000000000, 0.000000000000000000, 0.000000000000000000 ) ) ;
#34329 = ORIENTED_EDGE ( 'NONE', *, *, #104, .F. ) ;
#34330 = AXIS2_PLACEMENT_3D ( 'NONE', #591, #23555, #37249 ) ;
#34331 = CARTESIAN_POINT ( 'NONE',  ( -17.43724119492421565, 40.00000000000000000, -15.29674861594511803 ) ) ;
#34332 = CIRCLE ( 'NONE', #2264, 58.99999999999999289 ) ;
#34333 = ORIENTED_EDGE ( 'NONE', *, *, #23524, .F. ) ;
#34334 = ORIENTED_EDGE ( 'NONE', *, *, #6549, .F. ) ;
#34335 = DIRECTION ( 'NONE',  ( 0.000000000000000000, 0.000000000000000000, 1.000000000000000000 ) ) ;
#34336 = DIRECTION ( 'NONE',  ( 0.000000000000000000, 0.000000000000000000, -1.000000000000000000 ) ) ;
#34337 = CARTESIAN_POINT ( 'NONE',  ( 0.000000000000000000, 0.000000000000000000, 0.000000000000000000 ) ) ;
#34338 = LINE ( 'NONE', #4435, #3033 ) ;
#34339 = ORIENTED_EDGE ( 'NONE', *, *, #26258, .F. ) ;
#34340 = CARTESIAN_POINT ( 'NONE',  ( -130.0000000000000000, 4.615443851143692522E-16, 6.938893903907228378E-15 ) ) ;
#34341 = EDGE_LOOP ( 'NONE', ( #21627, #7481, #8274, #15599 ) ) ;
#34342 = CARTESIAN_POINT ( 'NONE',  ( 0.000000000000000000, -51.19683565102437939, -9.104066087303987587 ) ) ;
#34343 = CARTESIAN_POINT ( 'NONE',  ( 0.000000000000000000, 0.000000000000000000, -6.000000000000000000 ) ) ;
#34344 = ADVANCED_FACE ( 'NONE', ( #17027 ), #37055, .F. ) ;
#34345 = DIRECTION ( 'NONE',  ( -1.000000000000000000, -0.000000000000000000, 0.000000000000000000 ) ) ;
#34346 = EDGE_CURVE ( 'NONE', #14329, #23796, #16490, .T. ) ;
#34347 = EDGE_CURVE ( 'NONE', #2287, #3059, #29036, .T. ) ;
#34348 = CARTESIAN_POINT ( 'NONE',  ( 17.99999999999999645, 79.94368240339426279, 90.16373242487935613 ) ) ;
#34349 = ORIENTED_EDGE ( 'NONE', *, *, #19880, .T. ) ;
#34350 = ORIENTED_EDGE ( 'NONE', *, *, #30468, .F. ) ;
#34351 = CARTESIAN_POINT ( 'NONE',  ( 17.99999999999999645, 0.000000000000000000, 0.000000000000000000 ) ) ;
#34352 = DIRECTION ( 'NONE',  ( 0.000000000000000000, 0.000000000000000000, 1.000000000000000000 ) ) ;
#34353 = EDGE_CURVE ( 'NONE', #39721, #36486, #40826, .T. ) ;
#34354 = CIRCLE ( 'NONE', #15574, 14.99999999999999822 ) ;
#34355 = CARTESIAN_POINT ( 'NONE',  ( 4.211405965630455661, 2.460463115436283932, -3.751298928144577882 ) ) ;
#34356 = ORIENTED_EDGE ( 'NONE', *, *, #27048, .F. ) ;
#34358 = ORIENTED_EDGE ( 'NONE', *, *, #26195, .F. ) ;
#34357 = FACE_OUTER_BOUND ( 'NONE', #11716, .T. ) ;
#34359 = CARTESIAN_POINT ( 'NONE',  ( -39.38196478161825809, 31.00000000000000355, 13.29643045357694398 ) ) ;
#34360 = DIRECTION ( 'NONE',  ( -1.000000000000000000, -0.000000000000000000, 0.000000000000000000 ) ) ;
#34361 = EDGE_CURVE ( 'NONE', #11603, #3472, #5991, .T. ) ;
#34363 = CARTESIAN_POINT ( 'NONE',  ( 18.00000000000000355, 27.79676263918187118, 37.88001506494779846 ) ) ;
#34362 = DIRECTION ( 'NONE',  ( 1.000000000000000000, -0.000000000000000000, 0.000000000000000000 ) ) ;
#34364 = ORIENTED_EDGE ( 'NONE', *, *, #33784, .T. ) ;
#34365 = CARTESIAN_POINT ( 'NONE',  ( -40.14822235766499148, 40.00000000000000000, 45.62378674120105160 ) ) ;
#34366 = EDGE_CURVE ( 'NONE', #7826, #36784, #13527, .T. ) ;
#34367 = CARTESIAN_POINT ( 'NONE',  ( 18.00000000000000355, -29.60891106212812574, 37.14118181634756155 ) ) ;
#34368 = UNCERTAINTY_MEASURE_WITH_UNIT (LENGTH_MEASURE( 1.000000000000000082E-05 ), #18724, 'distance_accuracy_value', 'NONE');
#34369 = LINE ( 'NONE', #552, #35304 ) ;
#34370 = VERTEX_POINT ( 'NONE', #43164 ) ;
#34371 = DIRECTION ( 'NONE',  ( 1.000000000000000000, 0.000000000000000000, 0.000000000000000000 ) ) ;
#34372 = ORIENTED_EDGE ( 'NONE', *, *, #23747, .T. ) ;
#34373 = CARTESIAN_POINT ( 'NONE',  ( 0.000000000000000000, 0.000000000000000000, 0.000000000000000000 ) ) ;
#34374 = CARTESIAN_POINT ( 'NONE',  ( 58.80287614962789888, -12.05525454449572464, 69.29271901957253021 ) ) ;
#34375 = CARTESIAN_POINT ( 'NONE',  ( 7.506055610550203205, 31.00000000000000355, 56.92102948000351148 ) ) ;
#34376 = CARTESIAN_POINT ( 'NONE',  ( 0.000000000000000000, 25.18647942089742031, 113.2326863338528824 ) ) ;
#34377 = ORIENTED_EDGE ( 'NONE', *, *, #29985, .T. ) ;
#34378 = EDGE_CURVE ( 'NONE', #10114, #26923, #42656, .T. ) ;
#34379 = ORIENTED_EDGE ( 'NONE', *, *, #2029, .T. ) ;
#34380 = CARTESIAN_POINT ( 'NONE',  ( 16.69935377588158332, 40.00000000000000000, -28.93150767131472989 ) ) ;
#34381 = ORIENTED_EDGE ( 'NONE', *, *, #28578, .F. ) ;
#34382 = DIRECTION ( 'NONE',  ( 0.000000000000000000, 0.000000000000000000, 1.000000000000000000 ) ) ;
#34383 = DIRECTION ( 'NONE',  ( 1.000000000000000000, 0.000000000000000000, -0.000000000000000000 ) ) ;
#34384 = CARTESIAN_POINT ( 'NONE',  ( -23.42519174998115616, 31.00000000000000355, 87.00664592748896098 ) ) ;
#34385 = CARTESIAN_POINT ( 'NONE',  ( -88.68107738130200346, 40.00000000000000711, 23.63280646693861087 ) ) ;
#34386 = CYLINDRICAL_SURFACE ( 'NONE', #32735, 142.4999999999992610 ) ;
#34387 = ORIENTED_EDGE ( 'NONE', *, *, #16618, .F. ) ;
#34388 = CYLINDRICAL_SURFACE ( 'NONE', #38820, 120.5010000000000190 ) ;
#34389 = ORIENTED_EDGE ( 'NONE', *, *, #16477, .F. ) ;
#34390 = AXIS2_PLACEMENT_3D ( 'NONE', #34068, #14229, #22840 ) ;
#34391 = CARTESIAN_POINT ( 'NONE',  ( 0.000000000000000000, 0.000000000000000000, 0.000000000000000000 ) ) ;
#34392 = CARTESIAN_POINT ( 'NONE',  ( -4.024497503033519941, 2.323544716729375459, -3.572167766733379768 ) ) ;
#34394 = EDGE_LOOP ( 'NONE', ( #35574, #16430 ) ) ;
#34393 = FACE_OUTER_BOUND ( 'NONE', #23620, .T. ) ;
#34395 = ADVANCED_FACE ( 'NONE', ( #1378 ), #1589, .F. ) ;
#34396 = DIRECTION ( 'NONE',  ( 1.000000000000000000, 0.000000000000000000, 0.000000000000000000 ) ) ;
#34397 = ORIENTED_EDGE ( 'NONE', *, *, #31288, .T. ) ;
#34398 = CARTESIAN_POINT ( 'NONE',  ( 2.548804901056335857E-15, 4.736522675502163437, -3.681124513963624612 ) ) ;
#34399 = AXIS2_PLACEMENT_3D ( 'NONE', #4571, #18163, #24038 ) ;
#34400 = CARTESIAN_POINT ( 'NONE',  ( -78.67873774631718220, 40.00000000000000711, 60.36924185307643143 ) ) ;
#34401 = CARTESIAN_POINT ( 'NONE',  ( 0.000000000000000000, 0.000000000000000000, 0.000000000000000000 ) ) ;
#34402 = ORIENTED_EDGE ( 'NONE', *, *, #35439, .F. ) ;
#34403 = CARTESIAN_POINT ( 'NONE',  ( 17.99999999999999645, 0.000000000000000000, 0.000000000000000000 ) ) ;
#34404 = CYLINDRICAL_SURFACE ( 'NONE', #19050, 11.00000000000000000 ) ;
#34405 = AXIS2_PLACEMENT_3D ( 'NONE', #17262, #6956, #37273 ) ;
#34406 = EDGE_CURVE ( 'NONE', #31862, #9725, #2015, .T. ) ;
#34408 = DIRECTION ( 'NONE',  ( -1.000000000000000000, -0.000000000000000000, 0.000000000000000000 ) ) ;
#34407 = DIRECTION ( 'NONE',  ( 0.000000000000000000, 0.000000000000000000, 1.000000000000000000 ) ) ;
#34409 = CIRCLE ( 'NONE', #17736, 116.0000000000000000 ) ;
#34410 = ORIENTED_EDGE ( 'NONE', *, *, #41033, .F. ) ;
#34411 = DIRECTION ( 'NONE',  ( 0.000000000000000000, -2.663829608872859574E-14, -1.000000000000000000 ) ) ;
#34412 = ORIENTED_EDGE ( 'NONE', *, *, #28095, .F. ) ;
#34413 = DIRECTION ( 'NONE',  ( -1.000000000000000000, -0.000000000000000000, -0.000000000000000000 ) ) ;
#34414 = CARTESIAN_POINT ( 'NONE',  ( -31.99444157863030114, 40.00000000000000000, -4.262017635501984536 ) ) ;
#34415 = CARTESIAN_POINT ( 'NONE',  ( 18.00000000000000355, -20.99948489194451540, 42.60488980472774045 ) ) ;
#34416 = EDGE_CURVE ( 'NONE', #34617, #36642, #6705, .T. ) ;
#34417 = CARTESIAN_POINT ( 'NONE',  ( 17.99999999999999645, 16.77566611177777034, 119.3275660838943111 ) ) ;
#34418 = DIRECTION ( 'NONE',  ( -1.000000000000000000, 0.000000000000000000, 0.000000000000000000 ) ) ;
#34419 = ORIENTED_EDGE ( 'NONE', *, *, #3613, .T. ) ;
#34422 = CARTESIAN_POINT ( 'NONE',  ( 17.99999999999999645, -105.7179949885870514, 37.57629584241652054 ) ) ;
#34421 = DIRECTION ( 'NONE',  ( 1.000000000000000000, 0.000000000000000000, 0.000000000000000000 ) ) ;
#34420 = PRODUCT_DEFINITION_FORMATION_WITH_SPECIFIED_SOURCE ( 'ANY', '', #113, .NOT_KNOWN. ) ;
#34423 = ORIENTED_EDGE ( 'NONE', *, *, #30087, .F. ) ;
#34424 = DIRECTION ( 'NONE',  ( 3.996523416598930318E-16, -2.658563593772947863E-15, -1.000000000000000000 ) ) ;
#34425 = CARTESIAN_POINT ( 'NONE',  ( 0.000000000000000000, 0.000000000000000000, 0.000000000000000000 ) ) ;
#34426 = CARTESIAN_POINT ( 'NONE',  ( -9.022452542771789652, 31.00000000000000355, 26.59230923919664491 ) ) ;
#34427 = ORIENTED_EDGE ( 'NONE', *, *, #22846, .F. ) ;
#34428 = FACE_OUTER_BOUND ( 'NONE', #25598, .T. ) ;
#34429 = FACE_OUTER_BOUND ( 'NONE', #35471, .T. ) ;
#34430 = AXIS2_PLACEMENT_3D ( 'NONE', #12226, #12447, #31432 ) ;
#34431 = ITEM_DEFINED_TRANSFORMATION ( 'NONE', 'NONE', #30261,  #13552 ) ;
#34432 = AXIS2_PLACEMENT_3D ( 'NONE', #35539, #14869, #5659 ) ;
#34433 = CARTESIAN_POINT ( 'NONE',  ( 0.000000000000000000, 0.000000000000000000, 0.000000000000000000 ) ) ;
#34434 = CARTESIAN_POINT ( 'NONE',  ( 38.42722039544141666, 31.00000000000000355, 66.52996821281629991 ) ) ;
#34435 = AXIS2_PLACEMENT_3D ( 'NONE', #40440, #6639, #33688 ) ;
#34436 = VERTEX_POINT ( 'NONE', #6481 ) ;
#34437 = CARTESIAN_POINT ( 'NONE',  ( -28.59133019391535768, 31.00000000000000355, -32.71076623427349261 ) ) ;
#34438 = AXIS2_PLACEMENT_3D ( 'NONE', #3454, #30751, #40750 ) ;
#34439 = CARTESIAN_POINT ( 'NONE',  ( 77.05880969081472642, 39.99999999999999289, 37.98468489477117771 ) ) ;
#34440 = AXIS2_PLACEMENT_3D ( 'NONE', #21369, #37670, #11088 ) ;
#34441 = DIRECTION ( 'NONE',  ( -3.996523416598930318E-16, 2.658563593772947863E-15, 1.000000000000000000 ) ) ;
#34442 = DIRECTION ( 'NONE',  ( 1.000000000000000000, 0.000000000000000000, 0.000000000000000000 ) ) ;
#34443 = FACE_OUTER_BOUND ( 'NONE', #16877, .T. ) ;
#34445 = ORIENTED_EDGE ( 'NONE', *, *, #15309, .F. ) ;
#34444 = CARTESIAN_POINT ( 'NONE',  ( 17.99999999999999645, -92.10690493017105496, 64.06707842432145128 ) ) ;
#34446 = EDGE_CURVE ( 'NONE', #18211, #25660, #20675, .T. ) ;
#34447 = LINE ( 'NONE', #1715, #3012 ) ;
#34448 = LINE ( 'NONE', #5210, #9075 ) ;
#34449 = VECTOR ( 'NONE', #4421, 1000.000000000000000 ) ;
#34450 = VERTEX_POINT ( 'NONE', #19000 ) ;
#34451 = CARTESIAN_POINT ( 'NONE',  ( 63.32575250126041055, 39.99999999999999289, 16.95471465585521997 ) ) ;
#34452 = DIRECTION ( 'NONE',  ( 0.000000000000000000, 0.000000000000000000, 1.000000000000000000 ) ) ;
#34453 = FACE_OUTER_BOUND ( 'NONE', #25954, .T. ) ;
#34454 = EDGE_LOOP ( 'NONE', ( #30832, #8313 ) ) ;
#34455 = CARTESIAN_POINT ( 'NONE',  ( 0.000000000000000000, 0.000000000000000000, -4.974599999999998801 ) ) ;
#34456 = CARTESIAN_POINT ( 'NONE',  ( -79.93711883401132923, -2.055254544495720648, -145.8806300090334673 ) ) ;
#34457 = ORIENTED_EDGE ( 'NONE', *, *, #10177, .T. ) ;
#34458 = CARTESIAN_POINT ( 'NONE',  ( 17.99999999999999645, -87.74575819880217864, 75.87280091124446813 ) ) ;
#34459 = ORIENTED_EDGE ( 'NONE', *, *, #17023, .T. ) ;
#34460 = AXIS2_PLACEMENT_3D ( 'NONE', #3381, #9737, #19588 ) ;
#34461 = EDGE_CURVE ( 'NONE', #32652, #13915, #12430, .T. ) ;
#34462 = VECTOR ( 'NONE', #16355, 1000.000000000000000 ) ;
#34463 = CARTESIAN_POINT ( 'NONE',  ( 17.99999999999999645, -37.07968990261405651, -109.9140418541961282 ) ) ;
#34464 = ORIENTED_EDGE ( 'NONE', *, *, #33421, .F. ) ;
#34465 = AXIS2_PLACEMENT_3D ( 'NONE', #13172, #17696, #39734 ) ;
#34466 = DIRECTION ( 'NONE',  ( 1.000000000000000000, 0.000000000000000000, 0.000000000000000000 ) ) ;
#34467 = CARTESIAN_POINT ( 'NONE',  ( 17.99999999999999645, -15.21076497709635156, -119.5371223922156503 ) ) ;
#34468 = ADVANCED_FACE ( 'NONE', ( #6068 ), #29873, .F. ) ;
#34469 = ORIENTED_EDGE ( 'NONE', *, *, #4895, .F. ) ;
#34470 = CARTESIAN_POINT ( 'NONE',  ( 17.99999999999999645, 0.000000000000000000, 0.000000000000000000 ) ) ;
#34471 = DIRECTION ( 'NONE',  ( 0.000000000000000000, 0.7705132427757859226, 0.6374239897486936313 ) ) ;
#34472 = ORIENTED_EDGE ( 'NONE', *, *, #39810, .T. ) ;
#34473 = LINE ( 'NONE', #4579, #17620 ) ;
#34474 = LINE ( 'NONE', #4581, #1553 ) ;
#34475 = LINE ( 'NONE', #4584, #39859 ) ;
#34476 = LINE ( 'NONE', #10952, #40930 ) ;
#34477 = ORIENTED_EDGE ( 'NONE', *, *, #8051, .T. ) ;
#34479 = CIRCLE ( 'NONE', #3772, 47.49899999999998812 ) ;
#34478 = DIRECTION ( 'NONE',  ( 3.009274222671889652E-17, 0.9999999999999998890, -2.455023324936327764E-18 ) ) ;
#34480 = CARTESIAN_POINT ( 'NONE',  ( 0.000000000000000000, 0.000000000000000000, 0.000000000000000000 ) ) ;
#34481 = CARTESIAN_POINT ( 'NONE',  ( 3.436116956419347002, 31.00000000000000355, -52.60416666537189911 ) ) ;
#34482 = EDGE_CURVE ( 'NONE', #28956, #39558, #30760, .T. ) ;
#34483 = ORIENTED_EDGE ( 'NONE', *, *, #38068, .T. ) ;
#34485 = CARTESIAN_POINT ( 'NONE',  ( 0.000000000000000000, 6.854627147200274884, -115.7972974066012881 ) ) ;
#34484 = CARTESIAN_POINT ( 'NONE',  ( -91.96080130434580724, -12.05525454449572109, 14.45886780445738218 ) ) ;
#34486 = ADVANCED_FACE ( 'NONE', ( #19202 ), #2562, .T. ) ;
#34487 = CARTESIAN_POINT ( 'NONE',  ( 0.000000000000000000, 110.8621702203448649, 34.14058016547577523 ) ) ;
#34488 = VERTEX_POINT ( 'NONE', #43136 ) ;
#34489 = AXIS2_PLACEMENT_3D ( 'NONE', #31326, #35012, #5914 ) ;
#34490 = FACE_OUTER_BOUND ( 'NONE', #9964, .T. ) ;
#34491 = CARTESIAN_POINT ( 'NONE',  ( 28.34477777927418529, 40.00000000000000000, 36.93558740410973229 ) ) ;
#34492 = CIRCLE ( 'NONE', #31705, 25.00000000000000000 ) ;
#34493 = CARTESIAN_POINT ( 'NONE',  ( -3.998040010416403334, 40.00000000000000000, 59.59469406578620720 ) ) ;
#34494 = CIRCLE ( 'NONE', #8714, 59.00000000000000000 ) ;
#34495 = DIRECTION ( 'NONE',  ( 0.000000000000000000, 1.411300455031978640E-14, -1.000000000000000000 ) ) ;
#34496 = LINE ( 'NONE', #31252, #42978 ) ;
#34497 = VECTOR ( 'NONE', #43067, 1000.000000000000000 ) ;
#34498 = CARTESIAN_POINT ( 'NONE',  ( 18.00000000000000355, 46.90537658765334328, -2.727856614653797251 ) ) ;
#34499 = CARTESIAN_POINT ( 'NONE',  ( -18.08361268445098347, 31.00000000000000355, -10.43497034982449456 ) ) ;
#34500 = VECTOR ( 'NONE', #2873, 1000.000000000000000 ) ;
#34501 = EDGE_LOOP ( 'NONE', ( #22639, #6015 ) ) ;
#34502 = CARTESIAN_POINT ( 'NONE',  ( -2.924622967158192921, 40.00000000000000000, -22.14664255385889291 ) ) ;
#34503 = EDGE_LOOP ( 'NONE', ( #33586, #8572 ) ) ;
#34504 = DIRECTION ( 'NONE',  ( 0.000000000000000000, 0.000000000000000000, 1.000000000000000000 ) ) ;
#34505 = CARTESIAN_POINT ( 'NONE',  ( 18.00000000000000355, -22.43957647427129842, -41.27978878573651400 ) ) ;
#34506 = ORIENTED_EDGE ( 'NONE', *, *, #18162, .T. ) ;
#34507 = CYLINDRICAL_SURFACE ( 'NONE', #12440, 59.00000000000000000 ) ;
#34508 = DIRECTION ( 'NONE',  ( 0.000000000000000000, -1.224646799147353454E-16, 1.000000000000000000 ) ) ;
#34509 = VERTEX_POINT ( 'NONE', #25534 ) ;
#34510 = CARTESIAN_POINT ( 'NONE',  ( 18.00000000000000355, -36.05989434073635636, 30.12041790338605551 ) ) ;
#34511 = EDGE_LOOP ( 'NONE', ( #12044, #9142, #17201, #25573 ) ) ;
#34512 = EDGE_CURVE ( 'NONE', #42903, #32742, #24155, .T. ) ;
#34513 = CIRCLE ( 'NONE', #33112, 47.49900000000000944 ) ;
#34514 = ORIENTED_EDGE ( 'NONE', *, *, #29497, .F. ) ;
#34515 = DIRECTION ( 'NONE',  ( 1.000000000000000000, -0.000000000000000000, 0.000000000000000000 ) ) ;
#34516 = CARTESIAN_POINT ( 'NONE',  ( 60.45897909542819804, 31.00000000000000000, -46.24578392211154210 ) ) ;
#34517 = EDGE_CURVE ( 'NONE', #25122, #39322, #29639, .T. ) ;
#34518 = ORIENTED_EDGE ( 'NONE', *, *, #42887, .T. ) ;
#34519 = CARTESIAN_POINT ( 'NONE',  ( 18.00000000000000355, -46.87740477351715640, -3.172455868805708956 ) ) ;
#34520 = VECTOR ( 'NONE', #18922, 1000.000000000000000 ) ;
#34521 = CIRCLE ( 'NONE', #15742, 13.59999999999999964 ) ;
#34522 = DIRECTION ( 'NONE',  ( 1.000000000000000000, 0.000000000000000000, 0.000000000000000000 ) ) ;
#34523 = ORIENTED_EDGE ( 'NONE', *, *, #34031, .T. ) ;
#34524 = AXIS2_PLACEMENT_3D ( 'NONE', #28189, #41459, #2325 ) ;
#34525 = CARTESIAN_POINT ( 'NONE',  ( -5.560781378645575757, 6.809993116116508640E-16, -4.000000000000000000 ) ) ;
#34526 = ORIENTED_EDGE ( 'NONE', *, *, #8734, .T. ) ;
#34527 = CARTESIAN_POINT ( 'NONE',  ( 84.84057271799511568, 39.99999999999999289, 49.13019966419678752 ) ) ;
#34528 = CIRCLE ( 'NONE', #3821, 2.649999999999985700 ) ;
#34529 = CIRCLE ( 'NONE', #15748, 59.00000000000000000 ) ;
#34531 = CARTESIAN_POINT ( 'NONE',  ( 0.000000000000000000, 35.78425302087538995, 3.935382540232923887 ) ) ;
#34530 = FACE_OUTER_BOUND ( 'NONE', #11954, .T. ) ;
#34532 = CIRCLE ( 'NONE', #31061, 19.59999999999999076 ) ;
#34533 = DIRECTION ( 'NONE',  ( 1.000000000000000000, -0.000000000000000000, 0.000000000000000000 ) ) ;
#34534 = CARTESIAN_POINT ( 'NONE',  ( 17.99999999999999645, -0.5156212287287311735, 112.1962860721878172 ) ) ;
#34535 = VERTEX_POINT ( 'NONE', #25947 ) ;
#34536 =( LENGTH_UNIT ( ) NAMED_UNIT ( * ) SI_UNIT ( .MILLI., .METRE. ) );
#34537 = AXIS2_PLACEMENT_3D ( 'NONE', #11850, #24972, #9779 ) ;
#34538 = DIRECTION ( 'NONE',  ( 0.000000000000000000, 0.000000000000000000, 1.000000000000000000 ) ) ;
#34539 = ORIENTED_EDGE ( 'NONE', *, *, #30325, .F. ) ;
#34540 = CARTESIAN_POINT ( 'NONE',  ( 5.000000000000000888, 0.000000000000000000, 0.000000000000000000 ) ) ;
#34541 = CARTESIAN_POINT ( 'NONE',  ( 74.49266661913014786, 31.00000000000000000, 43.00976416799198176 ) ) ;
#34542 = EDGE_CURVE ( 'NONE', #34733, #33247, #17916, .T. ) ;
#34543 = CARTESIAN_POINT ( 'NONE',  ( 0.000000000000000000, -9.484061862023704492, -30.03730300138991538 ) ) ;
#34544 = ORIENTED_EDGE ( 'NONE', *, *, #30381, .T. ) ;
#34545 = ADVANCED_FACE ( 'NONE', ( #42488 ), #9332, .T. ) ;
#34546 = CARTESIAN_POINT ( 'NONE',  ( -31.89861325429239258, 40.00000000000000000, 2.042328591206914012 ) ) ;
#34547 =( REPRESENTATION_RELATIONSHIP ('NONE','NONE', #330, #37437 ) REPRESENTATION_RELATIONSHIP_WITH_TRANSFORMATION ( #20748 )SHAPE_REPRESENTATION_RELATIONSHIP( ) );
#34548 = VERTEX_POINT ( 'NONE', #42276 ) ;
#34549 = ORIENTED_EDGE ( 'NONE', *, *, #30009, .T. ) ;
#34550 = DIRECTION ( 'NONE',  ( 0.000000000000000000, 0.000000000000000000, 1.000000000000000000 ) ) ;
#34551 = DIRECTION ( 'NONE',  ( -1.000000000000000000, -0.000000000000000000, -0.000000000000000000 ) ) ;
#34553 = CARTESIAN_POINT ( 'NONE',  ( -22.00000000000000000, 40.00000000000000000, 0.000000000000000000 ) ) ;
#34552 = CIRCLE ( 'NONE', #2483, 116.0000000000000000 ) ;
#34554 = DIRECTION ( 'NONE',  ( 0.000000000000000000, 0.5528000653611945259, -0.8333139190825142872 ) ) ;
#34555 = AXIS2_PLACEMENT_3D ( 'NONE', #40047, #7121, #3406 ) ;
#34556 = EDGE_CURVE ( 'NONE', #29115, #36343, #4617, .T. ) ;
#34557 = ORIENTED_EDGE ( 'NONE', *, *, #2655, .T. ) ;
#34558 = LINE ( 'NONE', #10799, #8227 ) ;
#34559 = ORIENTED_EDGE ( 'NONE', *, *, #8813, .T. ) ;
#34560 = CARTESIAN_POINT ( 'NONE',  ( 17.99999999999999645, -78.18175027177490222, 85.69488855492974722 ) ) ;
#34561 = CARTESIAN_POINT ( 'NONE',  ( -19.74979319748359430, 117.9447454555042754, 2.972870684497276095 ) ) ;
#34562 = COLOUR_RGB ( '', 0.40784314, 0.44705882, 0.49803922) ;
#34563 = AXIS2_PLACEMENT_3D ( 'NONE', #32046, #2130, #24901 ) ;
#34564 = DIRECTION ( 'NONE',  ( 0.000000000000000000, 0.000000000000000000, 1.000000000000000000 ) ) ;
#34565 = AXIS2_PLACEMENT_3D ( 'NONE', #39710, #24050, #40576 ) ;
#34566 = CARTESIAN_POINT ( 'NONE',  ( -10.00000000000000000, 0.000000000000000000, 0.000000000000000000 ) ) ;
#34567 = VERTEX_POINT ( 'NONE', #29217 ) ;
#34568 = VERTEX_POINT ( 'NONE', #22273 ) ;
#34569 = DIRECTION ( 'NONE',  ( -3.009274222672345096E-17, -1.000000000000000000, 2.455023325076455345E-18 ) ) ;
#34570 = FACE_OUTER_BOUND ( 'NONE', #37584, .T. ) ;
#34571 = AXIS2_PLACEMENT_3D ( 'NONE', #1247, #37887, #9082 ) ;
#34572 = EDGE_CURVE ( 'NONE', #32209, #32785, #30395, .T. ) ;
#34573 = EDGE_LOOP ( 'NONE', ( #7694, #22069 ) ) ;
#34575 = ORIENTED_EDGE ( 'NONE', *, *, #891, .F. ) ;
#34574 = DIRECTION ( 'NONE',  ( 1.000000000000000000, -1.373900992973642263E-15, -3.996523416598957436E-16 ) ) ;
#34576 = CARTESIAN_POINT ( 'NONE',  ( -20.27214883179046367, 31.00000000000000355, 34.96734655410254788 ) ) ;
#34577 = EDGE_CURVE ( 'NONE', #4569, #3310, #5636, .T. ) ;
#34578 = CARTESIAN_POINT ( 'NONE',  ( 8.999999999999998224, 54.09091620264722877, 102.6166301549519488 ) ) ;
#34579 = CARTESIAN_POINT ( 'NONE',  ( -8.920000000000003482, 1.347111479062088405E-15, -11.00000000000000000 ) ) ;
#34580 = ORIENTED_EDGE ( 'NONE', *, *, #1184, .T. ) ;
#34581 = CARTESIAN_POINT ( 'NONE',  ( -10.00000000000000000, 0.000000000000000000, 0.000000000000000000 ) ) ;
#34582 = CARTESIAN_POINT ( 'NONE',  ( 66.75914267698914273, 39.99999999999999289, 8.899205196614580871 ) ) ;
#34583 = AXIS2_PLACEMENT_3D ( 'NONE', #9125, #15921, #38793 ) ;
#34584 = FACE_OUTER_BOUND ( 'NONE', #33363, .T. ) ;
#34585 = CYLINDRICAL_SURFACE ( 'NONE', #26164, 36.00000000000000000 ) ;
#34586 = ORIENTED_EDGE ( 'NONE', *, *, #18992, .T. ) ;
#34587 = CARTESIAN_POINT ( 'NONE',  ( 9.000000000000001776, 114.8812324315177023, -16.07179003769037351 ) ) ;
#34588 = VECTOR ( 'NONE', #11672, 1000.000000000000000 ) ;
#34589 = VERTEX_POINT ( 'NONE', #15701 ) ;
#34590 = CIRCLE ( 'NONE', #15143, 4.500000000000000888 ) ;
#34591 = CARTESIAN_POINT ( 'NONE',  ( 18.00000000000000355, -27.43636312076348815, 38.14186064215142835 ) ) ;
#34592 = DIRECTION ( 'NONE',  ( -1.000000000000000000, 0.000000000000000000, -0.000000000000000000 ) ) ;
#34593 = EDGE_CURVE ( 'NONE', #39974, #17009, #12843, .T. ) ;
#34594 = CARTESIAN_POINT ( 'NONE',  ( 55.10416666547021691, 31.00000000000000355, 3.599741573803287853 ) ) ;
#34595 = ADVANCED_FACE ( 'NONE', ( #12632 ), #39426, .T. ) ;
#34596 = CARTESIAN_POINT ( 'NONE',  ( 17.99999999999999645, 105.7179949885863266, 37.57629584241859533 ) ) ;
#34597 = ORIENTED_EDGE ( 'NONE', *, *, #30321, .F. ) ;
#34598 = EDGE_CURVE ( 'NONE', #35542, #5697, #23970, .T. ) ;
#34599 = ADVANCED_FACE ( 'NONE', ( #17219 ), #10194, .F. ) ;
#34600 = VERTEX_POINT ( 'NONE', #3419 ) ;
#34601 = CARTESIAN_POINT ( 'NONE',  ( 22.22924588317381023, 40.00000000000000000, -25.35314793696836588 ) ) ;
#34602 = VECTOR ( 'NONE', #4700, 1000.000000000000000 ) ;
#34603 = ORIENTED_EDGE ( 'NONE', *, *, #36950, .F. ) ;
#34604 = LINE ( 'NONE', #40486, #16628 ) ;
#34605 = CARTESIAN_POINT ( 'NONE',  ( 0.000000000000000000, -89.07460286905904923, 81.15544420874930154 ) ) ;
#34606 = CARTESIAN_POINT ( 'NONE',  ( -81.90010630563853056, 31.00000000000000711, 5.248159452637419342 ) ) ;
#34607 = CARTESIAN_POINT ( 'NONE',  ( 86.24314314301659579, 39.99999999999999289, -11.24622374122959201 ) ) ;
#34608 = AXIS2_PLACEMENT_3D ( 'NONE', #29360, #32398, #33903 ) ;
#34609 = FACE_OUTER_BOUND ( 'NONE', #19963, .T. ) ;
#34610 = VERTEX_POINT ( 'NONE', #27227 ) ;
#34611 = DIRECTION ( 'NONE',  ( 0.000000000000000000, 0.000000000000000000, 1.000000000000000000 ) ) ;
#34612 = ORIENTED_EDGE ( 'NONE', *, *, #6141, .T. ) ;
#34613 = CARTESIAN_POINT ( 'NONE',  ( 0.000000000000000000, 106.5605152861910909, -56.26142179985713909 ) ) ;
#34614 = CARTESIAN_POINT ( 'NONE',  ( 18.00000000000000355, -51.93417535146743802, 2.615612846549011383 ) ) ;
#34615 = AXIS2_PLACEMENT_3D ( 'NONE', #34185, #27020, #30281 ) ;
#34617 = VERTEX_POINT ( 'NONE', #13496 ) ;
#34616 = PLANE ( 'NONE',  #41558 ) ;
#34618 = DIRECTION ( 'NONE',  ( 1.000000000000000000, 0.000000000000000000, 0.000000000000000000 ) ) ;
#34619 = ORIENTED_EDGE ( 'NONE', *, *, #6183, .F. ) ;
#34620 = CARTESIAN_POINT ( 'NONE',  ( 17.99999999999999645, 0.000000000000000000, 0.000000000000000000 ) ) ;
#34621 = AXIS2_PLACEMENT_3D ( 'NONE', #15387, #39301, #2024 ) ;
#34622 = CARTESIAN_POINT ( 'NONE',  ( -99.14707074559267141, 40.00000000000000711, 13.06922382031732610 ) ) ;
#34623 = CARTESIAN_POINT ( 'NONE',  ( 1.734723475976807094E-15, 4.618802153517012954, -0.4999999999999995559 ) ) ;
#34624 = AXIS2_PLACEMENT_3D ( 'NONE', #11615, #8528, #14679 ) ;
#34625 = CIRCLE ( 'NONE', #21452, 120.5010000000000474 ) ;
#34626 = ORIENTED_EDGE ( 'NONE', *, *, #31581, .F. ) ;
#34627 = CARTESIAN_POINT ( 'NONE',  ( -20.64238946400878305, 17.11489954122026447, 3.177240882809045708 ) ) ;
#34628 = EDGE_CURVE ( 'NONE', #6200, #3612, #12998, .T. ) ;
#34629 = FACE_OUTER_BOUND ( 'NONE', #20156, .T. ) ;
#34630 = AXIS2_PLACEMENT_3D ( 'NONE', #34343, #7288, #17159 ) ;
#34631 = AXIS2_PLACEMENT_3D ( 'NONE', #6643, #3946, #17332 ) ;
#34633 = CARTESIAN_POINT ( 'NONE',  ( -3.996523416598931009E-15, 2.658563593772952281E-14, 10.00000000000000178 ) ) ;
#34632 = DIRECTION ( 'NONE',  ( 1.000000000000000000, -0.000000000000000000, 0.000000000000000000 ) ) ;
#34634 = ORIENTED_EDGE ( 'NONE', *, *, #133, .T. ) ;
#34635 = CARTESIAN_POINT ( 'NONE',  ( -106.4195705685756081, 106.4195705685752529, 6.999999999999998224 ) ) ;
#34636 = VERTEX_POINT ( 'NONE', #7573 ) ;
#34637 = CARTESIAN_POINT ( 'NONE',  ( -2.171643655288372443, 3.365003104552320767, 2.541098841762897165E-18 ) ) ;
#34638 = CARTESIAN_POINT ( 'NONE',  ( -14.91913624998189825, 40.00000000000000000, -30.37684071747814230 ) ) ;
#34639 = CARTESIAN_POINT ( 'NONE',  ( 0.000000000000000000, -118.8387007424472159, 19.94628303336444475 ) ) ;
#34640 = AXIS2_PLACEMENT_3D ( 'NONE', #13860, #40420, #14068 ) ;
#34641 = DIRECTION ( 'NONE',  ( -1.000000000000000000, 0.000000000000000000, -0.000000000000000000 ) ) ;
#34642 =( BOUNDED_SURFACE ( )  B_SPLINE_SURFACE ( 3, 2, ( 
 ( #8479, #5204, #18567 ),
 ( #39847, #36579, #6272 ),
 ( #29869, #26150, #26784 ),
 ( #19834, #12629, #29213 ),
 ( #23320, #6478, #23118 ),
 ( #42911, #32465, #9973 ) ),
 .UNSPECIFIED., .F., .F., .F. ) 
 B_SPLINE_SURFACE_WITH_KNOTS ( ( 4, 2, 4 ),
 ( 3, 3 ),
 ( 0.02032853247518126918, 0.02278863295364821906, 0.02524873343211516893 ),
 ( 0.000000000000000000, 1.000000000000000000 ),
 .UNSPECIFIED. ) 
 GEOMETRIC_REPRESENTATION_ITEM ( )  RATIONAL_B_SPLINE_SURFACE ( (
 ( 1.000000000000000000, 0.8047781615896838492, 1.000000000000000000),
 ( 1.000000000000000000, 0.8123767586288186404, 1.000000000000000000),
 ( 1.000000000000000000, 0.8190662415565814758, 1.000000000000000000),
 ( 1.000000000000000000, 0.8192361015667604107, 1.000000000000000000),
 ( 1.000000000000000000, 0.8126135807104967190, 1.000000000000000000),
 ( 1.000000000000000000, 0.8047712338318580017, 1.000000000000000000) ) ) 
 REPRESENTATION_ITEM ( '' )  SURFACE ( )  );
#34643 = DIRECTION ( 'NONE',  ( 1.000000000000000000, -1.373900992973642263E-15, 0.000000000000000000 ) ) ;
#34644 = ORIENTED_EDGE ( 'NONE', *, *, #19876, .T. ) ;
#34646 = CARTESIAN_POINT ( 'NONE',  ( 0.6640947660595348800, -4.471078309994175548, -3.602146406945708090 ) ) ;
#34645 = CARTESIAN_POINT ( 'NONE',  ( 17.99999999999999645, 17.77780072541854040, -114.6296200873374147 ) ) ;
#34647 = EDGE_LOOP ( 'NONE', ( #21637, #36571, #446, #9463 ) ) ;
#34648 = DIRECTION ( 'NONE',  ( -1.000000000000000000, -0.000000000000000000, -0.000000000000000000 ) ) ;
#34649 = LINE ( 'NONE', #23632, #18520 ) ;
#34650 = CARTESIAN_POINT ( 'NONE',  ( 8.699408683037360035, 31.00000000000000355, 25.59862650653646909 ) ) ;
#34651 = ORIENTED_EDGE ( 'NONE', *, *, #10125, .T. ) ;
#34652 = DIRECTION ( 'NONE',  ( 1.000000000000000000, 0.000000000000000000, 0.000000000000000000 ) ) ;
#34653 = EDGE_CURVE ( 'NONE', #8703, #27194, #16525, .T. ) ;
#34654 = ADVANCED_FACE ( 'NONE', ( #39851 ), #351, .F. ) ;
#34655 = FACE_BOUND ( 'NONE', #3839, .T. ) ;
#34656 = AXIS2_PLACEMENT_3D ( 'NONE', #30606, #14032, #28422 ) ;
#34657 = CIRCLE ( 'NONE', #37416, 59.00000000000000711 ) ;
#34658 = EDGE_CURVE ( 'NONE', #1973, #40378, #462, .T. ) ;
#34659 = DIRECTION ( 'NONE',  ( -1.000000000000000000, -0.000000000000000000, -0.000000000000000000 ) ) ;
#34660 = CARTESIAN_POINT ( 'NONE',  ( 10.81967497908702214, 31.00000000000000355, -82.17651821321413763 ) ) ;
#34661 = AXIS2_PLACEMENT_3D ( 'NONE', #17868, #11082, #24187 ) ;
#34662 = AXIS2_PLACEMENT_3D ( 'NONE', #8181, #35432, #8387 ) ;
#34663 = ORIENTED_EDGE ( 'NONE', *, *, #874, .F. ) ;
#34665 = CARTESIAN_POINT ( 'NONE',  ( 3.665567271000699012, 31.00000000000000355, -54.59530427605618996 ) ) ;
#34664 = CIRCLE ( 'NONE', #17300, 120.5010000000000332 ) ;
#34666 = CARTESIAN_POINT ( 'NONE',  ( 64.90595555531619709, 39.99999999999999289, 56.92265028770086843 ) ) ;
#34667 = ORIENTED_EDGE ( 'NONE', *, *, #19051, .T. ) ;
#34668 = CARTESIAN_POINT ( 'NONE',  ( 17.99999999999999645, -120.3696465864706369, 5.624871700595674540 ) ) ;
#34669 = AXIS2_PLACEMENT_3D ( 'NONE', #12400, #22450, #19173 ) ;
#34670 = EDGE_CURVE ( 'NONE', #13195, #23588, #16788, .T. ) ;
#34671 = DIRECTION ( 'NONE',  ( -3.009274222672345096E-17, -1.000000000000000000, 2.455023325076454960E-18 ) ) ;
#34672 = FACE_OUTER_BOUND ( 'NONE', #31436, .T. ) ;
#34674 = EDGE_LOOP ( 'NONE', ( #731, #23384, #7592, #17723 ) ) ;
#34673 = DIRECTION ( 'NONE',  ( -1.000000000000000000, 0.000000000000000000, 0.000000000000000000 ) ) ;
#34675 = CARTESIAN_POINT ( 'NONE',  ( 17.99999999999999645, 110.0562500189205224, -49.07252625220001363 ) ) ;
#34676 = CARTESIAN_POINT ( 'NONE',  ( 3.983177536951266529, -13.66651769228263191, -1.199999999999999956 ) ) ;
#34677 = ORIENTED_EDGE ( 'NONE', *, *, #7254, .F. ) ;
#34678 = CARTESIAN_POINT ( 'NONE',  ( 21.58803501788969115, 40.00000000000000000, 63.55567069162312777 ) ) ;
#34679 = FACE_OUTER_BOUND ( 'NONE', #8809, .T. ) ;
#34680 = ORIENTED_EDGE ( 'NONE', *, *, #7652, .F. ) ;
#34681 = VECTOR ( 'NONE', #19313, 1000.000000000000000 ) ;
#34682 = FACE_OUTER_BOUND ( 'NONE', #4148, .T. ) ;
#34683 = CARTESIAN_POINT ( 'NONE',  ( -4.000000000000000000, 0.000000000000000000, 0.000000000000000000 ) ) ;
#34684 = ORIENTED_EDGE ( 'NONE', *, *, #19528, .F. ) ;
#34685 = DIRECTION ( 'NONE',  ( 0.000000000000000000, 0.000000000000000000, -1.000000000000000000 ) ) ;
#34686 = ORIENTED_EDGE ( 'NONE', *, *, #22006, .T. ) ;
#34687 = AXIS2_PLACEMENT_3D ( 'NONE', #30120, #13120, #20324 ) ;
#34688 = CIRCLE ( 'NONE', #29138, 20.00000000000000711 ) ;
#34689 = DIRECTION ( 'NONE',  ( 0.000000000000000000, 0.000000000000000000, 1.000000000000000000 ) ) ;
#34690 = VERTEX_POINT ( 'NONE', #17654 ) ;
#34691 = AXIS2_PLACEMENT_3D ( 'NONE', #19782, #6431, #12789 ) ;
#34692 = DIRECTION ( 'NONE',  ( 0.000000000000000000, 0.000000000000000000, 1.000000000000000000 ) ) ;
#34693 = CARTESIAN_POINT ( 'NONE',  ( -66.59699903142619348, 31.00000000000000711, 75.74378954611491110 ) ) ;
#34694 = ORIENTED_EDGE ( 'NONE', *, *, #5686, .T. ) ;
#34695 = CIRCLE ( 'NONE', #11050, 116.0000000000000000 ) ;
#34696 = FACE_OUTER_BOUND ( 'NONE', #31442, .T. ) ;
#34697 = DIRECTION ( 'NONE',  ( -1.000000000000000000, -0.000000000000000000, -0.000000000000000000 ) ) ;
#34698 = EDGE_LOOP ( 'NONE', ( #5803, #39118 ) ) ;
#34699 = LINE ( 'NONE', #31440, #29423 ) ;
#34700 = VECTOR ( 'NONE', #27633, 1000.000000000000000 ) ;
#34701 = FACE_OUTER_BOUND ( 'NONE', #902, .T. ) ;
#34702 = ORIENTED_EDGE ( 'NONE', *, *, #2848, .F. ) ;
#34703 = DIRECTION ( 'NONE',  ( -1.000000000000000000, -0.000000000000000000, 0.000000000000000000 ) ) ;
#34704 = EDGE_CURVE ( 'NONE', #32609, #23378, #16997, .T. ) ;
#34705 = DIRECTION ( 'NONE',  ( -1.000000000000000000, 0.000000000000000000, -0.000000000000000000 ) ) ;
#34706 = PRODUCT_CONTEXT ( 'NONE', #37852, 'mechanical' ) ;
#34707 = DIRECTION ( 'NONE',  ( 0.000000000000000000, 0.000000000000000000, 1.000000000000000000 ) ) ;
#34708 = CARTESIAN_POINT ( 'NONE',  ( -16.75480014238754478, 31.00000000000000355, -49.32177912249007790 ) ) ;
#34709 = ORIENTED_EDGE ( 'NONE', *, *, #4427, .T. ) ;
#34711 = CARTESIAN_POINT ( 'NONE',  ( -20.39032260654148487, 31.00000000000000355, 1.150830359615497178 ) ) ;
#34710 = CYLINDRICAL_SURFACE ( 'NONE', #16351, 13.60000000000000142 ) ;
#34712 = DIRECTION ( 'NONE',  ( 1.000000000000000000, 0.000000000000000000, 0.000000000000000000 ) ) ;
#34713 = CIRCLE ( 'NONE', #15931, 58.99999999999999289 ) ;
#34714 = EDGE_LOOP ( 'NONE', ( #16782, #24399, #26769 ) ) ;
#34715 = AXIS2_PLACEMENT_3D ( 'NONE', #7626, #1294, #34034 ) ;
#34716 = EDGE_CURVE ( 'NONE', #28980, #17756, #26581, .T. ) ;
#34717 = LINE ( 'NONE', #7880, #367 ) ;
#34718 = CARTESIAN_POINT ( 'NONE',  ( 52.83624534446448706, 40.00000000000000000, -14.15919354876300318 ) ) ;
#34719 = CIRCLE ( 'NONE', #14535, 31.49899999999999878 ) ;
#34720 = CARTESIAN_POINT ( 'NONE',  ( 57.09498703527649610, 40.00000000000000000, 3.831922229401318880 ) ) ;
#34721 = EDGE_CURVE ( 'NONE', #36878, #9086, #14433, .T. ) ;
#34722 = CIRCLE ( 'NONE', #15936, 58.99999999999999289 ) ;
#34723 = AXIS2_PLACEMENT_3D ( 'NONE', #39774, #23892, #50 ) ;
#34724 = CIRCLE ( 'NONE', #21546, 59.00000000000001421 ) ;
#34725 = CARTESIAN_POINT ( 'NONE',  ( 0.000000000000000000, 1.178949249685217415, 2.041999999999998483 ) ) ;
#34726 = EDGE_CURVE ( 'NONE', #4308, #29708, #13932, .T. ) ;
#34727 = FACE_OUTER_BOUND ( 'NONE', #12770, .T. ) ;
#34728 = AXIS2_PLACEMENT_3D ( 'NONE', #40997, #38746, #4559 ) ;
#34729 = CARTESIAN_POINT ( 'NONE',  ( 17.99999999999999645, -13.00789606333550097, 115.2683592318614672 ) ) ;
#34730 = CARTESIAN_POINT ( 'NONE',  ( -9.654069774896838041, 31.00000000000000355, -19.56573356436190636 ) ) ;
#34731 = VERTEX_POINT ( 'NONE', #10638 ) ;
#34732 = CARTESIAN_POINT ( 'NONE',  ( -8.325335757348113930, 40.00000000000000000, -31.05587074991522201 ) ) ;
#34733 = VERTEX_POINT ( 'NONE', #6706 ) ;
#34734 = LINE ( 'NONE', #5053, #25753 ) ;
#34735 = CARTESIAN_POINT ( 'NONE',  ( -4.236525694536558362, 2.416953475386465211, -3.751298745799836354 ) ) ;
#34736 = ORIENTED_EDGE ( 'NONE', *, *, #2206, .T. ) ;
#34737 = CYLINDRICAL_SURFACE ( 'NONE', #23596, 10.50000000000000178 ) ;
#34738 = CARTESIAN_POINT ( 'NONE',  ( -23.34979319748359927, 5.944745455504278020, 2.972870684497277427 ) ) ;
#34739 = ORIENTED_EDGE ( 'NONE', *, *, #22986, .F. ) ;
#34740 = DIRECTION ( 'NONE',  ( 0.000000000000000000, 0.000000000000000000, 1.000000000000000000 ) ) ;
#34741 = ORIENTED_EDGE ( 'NONE', *, *, #38286, .F. ) ;
#34742 = EDGE_CURVE ( 'NONE', #3059, #40767, #10940, .T. ) ;
#34743 = EDGE_CURVE ( 'NONE', #40301, #25300, #15832, .T. ) ;
#34744 = ORIENTED_EDGE ( 'NONE', *, *, #20368, .T. ) ;
#34745 = CYLINDRICAL_SURFACE ( 'NONE', #2055, 11.00000000000023448 ) ;
#34746 = CARTESIAN_POINT ( 'NONE',  ( -53.44803860757283331, 31.00000000000000355, 46.73995993579659114 ) ) ;
#34748 = EDGE_CURVE ( 'NONE', #37926, #8001, #20710, .T. ) ;
#34747 = ORIENTED_EDGE ( 'NONE', *, *, #31112, .F. ) ;
#34749 = CARTESIAN_POINT ( 'NONE',  ( 0.000000000000000000, 0.000000000000000000, 0.000000000000000000 ) ) ;
#34750 = AXIS2_PLACEMENT_3D ( 'NONE', #20131, #36423, #419 ) ;
#34751 = LINE ( 'NONE', #14922, #40040 ) ;
#34752 = CIRCLE ( 'NONE', #593, 13.59999999999999964 ) ;
#34753 = ORIENTED_EDGE ( 'NONE', *, *, #4262, .T. ) ;
#34754 = DIRECTION ( 'NONE',  ( -1.000000000000000000, 0.000000000000000000, 0.000000000000000000 ) ) ;
#34755 = VERTEX_POINT ( 'NONE', #33976 ) ;
#34756 = CARTESIAN_POINT ( 'NONE',  ( 73.86091552542920624, 39.99999999999999289, 64.94433634442138725 ) ) ;
#34757 = CARTESIAN_POINT ( 'NONE',  ( 21.18498618631003083, 31.00000000000000355, 18.62224443192850387 ) ) ;
#34759 = DIRECTION ( 'NONE',  ( 0.000000000000000000, 0.000000000000000000, 1.000000000000000000 ) ) ;
#34758 = DIRECTION ( 'NONE',  ( 0.000000000000000000, 0.4132121857683728749, 0.9106347728549155640 ) ) ;
#34760 = CARTESIAN_POINT ( 'NONE',  ( 9.000000000000001776, -25.18647942089668490, -113.2326863338530245 ) ) ;
#34761 = DIRECTION ( 'NONE',  ( -1.000000000000000000, 0.000000000000000000, -0.000000000000000000 ) ) ;
#34762 = EDGE_CURVE ( 'NONE', #5703, #3775, #1157, .T. ) ;
#34763 = VERTEX_POINT ( 'NONE', #30715 ) ;
#34764 = SHAPE_REPRESENTATION_RELATIONSHIP ( 'NONE' , 'NONE' ,  #16840, #20853 ) ;
#34765 = CYLINDRICAL_SURFACE ( 'NONE', #41532, 120.5010000000000190 ) ;
#34766 = ORIENTED_EDGE ( 'NONE', *, *, #20312, .T. ) ;
#34767 = CARTESIAN_POINT ( 'NONE',  ( 0.000000000000000000, -18.42432724429495394, 30.92804820215996386 ) ) ;
#34768 = CARTESIAN_POINT ( 'NONE',  ( 83.17098260925966713, 31.00000000000000000, 48.02127090943169208 ) ) ;
#34769 = PLANE ( 'NONE',  #7206 ) ;
#34770 = ORIENTED_EDGE ( 'NONE', *, *, #41973, .T. ) ;
#34771 = CARTESIAN_POINT ( 'NONE',  ( 25.73918080462997082, 40.00000000000000000, -6.871072672212912735 ) ) ;
#34772 = ADVANCED_FACE ( 'NONE', ( #790 ), #40058, .F. ) ;
#34773 = EDGE_LOOP ( 'NONE', ( #36770, #21173, #9184, #5928 ) ) ;
#34774 = VERTEX_POINT ( 'NONE', #41144 ) ;
#34775 = DIRECTION ( 'NONE',  ( 3.996523416598993920E-16, 2.658563593772947074E-15, 1.000000000000000000 ) ) ;
#34776 = DIRECTION ( 'NONE',  ( -1.000000000000000000, -0.000000000000000000, -0.000000000000000000 ) ) ;
#34777 = CIRCLE ( 'NONE', #2695, 2.649999999999993694 ) ;
#34778 = CARTESIAN_POINT ( 'NONE',  ( 18.00000000000000355, 0.000000000000000000, 0.000000000000000000 ) ) ;
#34779 = CIRCLE ( 'NONE', #18110, 0.4000000000000010214 ) ;
#34780 = EDGE_CURVE ( 'NONE', #15532, #23705, #28541, .T. ) ;
#34781 = DIRECTION ( 'NONE',  ( -1.000000000000000000, 0.000000000000000000, 0.000000000000000000 ) ) ;
#34782 = CIRCLE ( 'NONE', #20183, 116.0000000000000000 ) ;
#34783 = VERTEX_POINT ( 'NONE', #4950 ) ;
#34784 = CYLINDRICAL_SURFACE ( 'NONE', #42335, 120.5010000000000190 ) ;
#34785 = EDGE_LOOP ( 'NONE', ( #27983, #4348, #7739, #21423 ) ) ;
#34786 = DIRECTION ( 'NONE',  ( 1.000000000000000000, -0.000000000000000000, 0.000000000000000000 ) ) ;
#34787 = DIRECTION ( 'NONE',  ( 0.000000000000000000, 0.000000000000000000, -1.000000000000000000 ) ) ;
#34788 = CARTESIAN_POINT ( 'NONE',  ( 8.999999999999998224, 1.641026710857453510E-15, 13.40000000000000213 ) ) ;
#34789 = CARTESIAN_POINT ( 'NONE',  ( 18.00000000000000355, -44.25018368420723647, -27.31155879685227106 ) ) ;
#34790 = ORIENTED_EDGE ( 'NONE', *, *, #15255, .F. ) ;
#34791 = VERTEX_POINT ( 'NONE', #31362 ) ;
#34792 = CARTESIAN_POINT ( 'NONE',  ( 0.000000000000000000, -83.58328028049608349, -80.43528614701409651 ) ) ;
#34793 = DIRECTION ( 'NONE',  ( -1.000000000000000000, 0.000000000000000000, 0.000000000000000000 ) ) ;
#34794 = EDGE_CURVE ( 'NONE', #23705, #1507, #15132, .T. ) ;
#34795 = ORIENTED_EDGE ( 'NONE', *, *, #22623, .F. ) ;
#34797 = ORIENTED_EDGE ( 'NONE', *, *, #12257, .T. ) ;
#34796 = DIRECTION ( 'NONE',  ( 0.000000000000000000, 1.000000000000000000, 0.000000000000000000 ) ) ;
#34798 = CARTESIAN_POINT ( 'NONE',  ( -41.89947471387618805, 31.00000000000000355, 2.670153906482984674 ) ) ;
#34799 = EDGE_CURVE ( 'NONE', #41039, #6230, #18305, .T. ) ;
#34800 = DIRECTION ( 'NONE',  ( -1.058513553088275437E-16, -1.000000000000000000, 8.813324511995299047E-17 ) ) ;
#34802 = FACE_OUTER_BOUND ( 'NONE', #37946, .T. ) ;
#34801 = CARTESIAN_POINT ( 'NONE',  ( -4.000000000000000000, 1.941961291383472732, -0.3515519931180205448 ) ) ;
#34803 = ORIENTED_EDGE ( 'NONE', *, *, #3400, .T. ) ;
#34804 = CARTESIAN_POINT ( 'NONE',  ( 17.99999999999999645, 62.45178862086215332, 93.20969140437529177 ) ) ;
#34805 = CARTESIAN_POINT ( 'NONE',  ( -61.40313508883502891, 40.00000000000000711, 7.989450542818913092 ) ) ;
#34806 = AXIS2_PLACEMENT_3D ( 'NONE', #24645, #14165, #27246 ) ;
#34807 = CIRCLE ( 'NONE', #17437, 51.99999999999999289 ) ;
#34808 = AXIS2_PLACEMENT_3D ( 'NONE', #6158, #23416, #19503 ) ;
#34809 = FACE_OUTER_BOUND ( 'NONE', #18595, .T. ) ;
#34810 = DIRECTION ( 'NONE',  ( 0.000000000000000000, 0.4817536741017100499, 0.8763066800438665815 ) ) ;
#34811 = VERTEX_POINT ( 'NONE', #22000 ) ;
#34812 = CARTESIAN_POINT ( 'NONE',  ( 18.00000000000000355, 47.49120266317495265, -0.8606222198177008176 ) ) ;
#34813 = EDGE_CURVE ( 'NONE', #41650, #11761, #25272, .T. ) ;
#34814 = EDGE_LOOP ( 'NONE', ( #9621, #23288, #24224, #11226, #39338 ) ) ;
#34815 = CARTESIAN_POINT ( 'NONE',  ( 0.000000000000000000, 0.000000000000000000, 0.000000000000000000 ) ) ;
#34816 = DIRECTION ( 'NONE',  ( 0.000000000000000000, 0.000000000000000000, 1.000000000000000000 ) ) ;
#34817 = DIRECTION ( 'NONE',  ( 1.000000000000000000, 0.000000000000000000, 0.000000000000000000 ) ) ;
#34818 = CARTESIAN_POINT ( 'NONE',  ( 4.745113895470035814, 31.00000000000000355, -72.60416666572081112 ) ) ;
#34819 = CARTESIAN_POINT ( 'NONE',  ( 18.00000000000000355, 0.000000000000000000, 0.000000000000000000 ) ) ;
#34820 = ORIENTED_EDGE ( 'NONE', *, *, #1790, .F. ) ;
#34821 = ADVANCED_FACE ( 'NONE', ( #28323 ), #11511, .T. ) ;
#34822 = ORIENTED_EDGE ( 'NONE', *, *, #33637, .T. ) ;
#34823 = DIRECTION ( 'NONE',  ( 0.000000000000000000, 0.000000000000000000, 1.000000000000000000 ) ) ;
#34824 = EDGE_CURVE ( 'NONE', #24285, #39306, #18522, .T. ) ;
#34825 = CARTESIAN_POINT ( 'NONE',  ( 18.00000000000000355, -19.44205635905570873, 43.33776004284602124 ) ) ;
#34826 = CARTESIAN_POINT ( 'NONE',  ( 11.57239447661056353, 31.00000000000000355, 88.72710294830137912 ) ) ;
#34827 = CARTESIAN_POINT ( 'NONE',  ( 64.75392801420538547, 39.99999999999999289, -56.64582372546511380 ) ) ;
#34828 = DIRECTION ( 'NONE',  ( -0.000000000000000000, -0.000000000000000000, 1.000000000000000000 ) ) ;
#34829 = EDGE_LOOP ( 'NONE', ( #2652, #32730, #13168, #90 ) ) ;
#34830 = FACE_OUTER_BOUND ( 'NONE', #30624, .T. ) ;
#34831 = VERTEX_POINT ( 'NONE', #27670 ) ;
#34832 = CARTESIAN_POINT ( 'NONE',  ( 0.000000000000000000, 112.1702510623870381, -2.471285140322999840 ) ) ;
#34833 = CIRCLE ( 'NONE', #24441, 58.99999999999999289 ) ;
#34834 = CARTESIAN_POINT ( 'NONE',  ( 7.000000000000002665, -18.77999999999998337, 2.299886688798728323E-15 ) ) ;
#34836 = ORIENTED_EDGE ( 'NONE', *, *, #32623, .T. ) ;
#34835 = CARTESIAN_POINT ( 'NONE',  ( 0.000000000000000000, 0.000000000000000000, 0.000000000000000000 ) ) ;
#34837 = DIRECTION ( 'NONE',  ( 1.000000000000000000, -0.000000000000000000, -0.000000000000000000 ) ) ;
#34838 = ORIENTED_EDGE ( 'NONE', *, *, #27111, .F. ) ;
#34839 = CARTESIAN_POINT ( 'NONE',  ( 0.000000000000000000, 49.25004636492411692, -16.68630974939707556 ) ) ;
#34840 = CARTESIAN_POINT ( 'NONE',  ( -74.47060461443528823, 40.00000000000000711, 65.33029858165178894 ) ) ;
#34841 = CARTESIAN_POINT ( 'NONE',  ( 18.00000000000000355, 30.93515269692163017, -36.04401931830219752 ) ) ;
#34842 = VERTEX_POINT ( 'NONE', #11293 ) ;
#34843 = ADVANCED_FACE ( 'NONE', ( #5382 ), #1237, .F. ) ;
#34844 = LINE ( 'NONE', #38117, #3210 ) ;
#34845 = EDGE_CURVE ( 'NONE', #16742, #42167, #24193, .T. ) ;
#34846 = DIRECTION ( 'NONE',  ( -0.000000000000000000, 1.000000000000000000, 1.224646799147353207E-16 ) ) ;
#34847 = EDGE_CURVE ( 'NONE', #39905, #40629, #37878, .T. ) ;
#34848 = EDGE_CURVE ( 'NONE', #1340, #40004, #7786, .T. ) ;
#34849 = EDGE_CURVE ( 'NONE', #27222, #19395, #27669, .T. ) ;
#34851 = FACE_OUTER_BOUND ( 'NONE', #7331, .T. ) ;
#34850 = DIRECTION ( 'NONE',  ( 0.000000000000000000, 0.000000000000000000, 1.000000000000000000 ) ) ;
#34852 = ORIENTED_EDGE ( 'NONE', *, *, #40653, .F. ) ;
#34853 = CARTESIAN_POINT ( 'NONE',  ( 9.000000000000001776, 51.85248208264517444, 3.914090171286374265 ) ) ;
#34854 = VERTEX_POINT ( 'NONE', #24414 ) ;
#34855 = CARTESIAN_POINT ( 'NONE',  ( 0.000000000000000000, 47.58001226230536673, 110.7096808509485300 ) ) ;
#34856 = CARTESIAN_POINT ( 'NONE',  ( 35.42814233786123879, 40.00000000000000000, -9.427541829740359702 ) ) ;
#34857 = DIRECTION ( 'NONE',  ( 1.000000000000000000, 0.000000000000000000, 0.000000000000000000 ) ) ;
#34858 = LINE ( 'NONE', #31590, #17305 ) ;
#34859 = DIRECTION ( 'NONE',  ( -1.000000000000000000, -0.000000000000000000, -0.000000000000000000 ) ) ;
#34860 = ORIENTED_EDGE ( 'NONE', *, *, #24425, .F. ) ;
#34861 = CARTESIAN_POINT ( 'NONE',  ( -0.02448733951239248641, -4.877042772274742255, -3.751161874094027571 ) ) ;
#34862 = ORIENTED_EDGE ( 'NONE', *, *, #29586, .F. ) ;
#34863 = AXIS2_PLACEMENT_3D ( 'NONE', #34235, #36255, #30970 ) ;
#34864 = DIRECTION ( 'NONE',  ( 1.000000000000000000, 0.000000000000000000, 0.000000000000000000 ) ) ;
#34865 = LINE ( 'NONE', #18337, #24104 ) ;
#34866 = AXIS2_PLACEMENT_3D ( 'NONE', #964, #14975, #7960 ) ;
#34868 = CARTESIAN_POINT ( 'NONE',  ( -25.29482881991252086, 31.00000000000000355, -32.96004927633274662 ) ) ;
#34867 = CIRCLE ( 'NONE', #16077, 7.500000000000000000 ) ;
#34869 = ORIENTED_EDGE ( 'NONE', *, *, #13155, .F. ) ;
#34870 = CARTESIAN_POINT ( 'NONE',  ( 17.99999999999999645, 104.0201923570375300, 51.34003878071097660 ) ) ;
#34871 = CIRCLE ( 'NONE', #18196, 2.041999999999999815 ) ;
#34872 = CYLINDRICAL_SURFACE ( 'NONE', #30280, 116.0000000000000000 ) ;
#34873 = EDGE_CURVE ( 'NONE', #35008, #32609, #11626, .T. ) ;
#34874 = CARTESIAN_POINT ( 'NONE',  ( 34.02738612458995959, 31.00000000000000355, 69.00154638599002510 ) ) ;
#34875 = ORIENTED_EDGE ( 'NONE', *, *, #22136, .T. ) ;
#34876 = CARTESIAN_POINT ( 'NONE',  ( 50.61746024623598572, 31.00000000000000355, -24.85206051842254737 ) ) ;
#34877 = EDGE_CURVE ( 'NONE', #40017, #35289, #21367, .T. ) ;
#34878 = CARTESIAN_POINT ( 'NONE',  ( -66.93673649651354651, 40.00000000000000711, 58.72203107584222437 ) ) ;
#34879 = ORIENTED_EDGE ( 'NONE', *, *, #14090, .F. ) ;
#34880 = DIRECTION ( 'NONE',  ( -1.000000000000000000, 3.009274222672345096E-17, 0.000000000000000000 ) ) ;
#34881 = CIRCLE ( 'NONE', #13975, 59.00000000000000000 ) ;
#34882 = DIRECTION ( 'NONE',  ( 1.000000000000000000, -0.000000000000000000, -0.000000000000000000 ) ) ;
#34883 = LINE ( 'NONE', #18356, #1731 ) ;
#34885 = ORIENTED_EDGE ( 'NONE', *, *, #18108, .F. ) ;
#34884 = FACE_OUTER_BOUND ( 'NONE', #34773, .T. ) ;
#34886 = CARTESIAN_POINT ( 'NONE',  ( 0.000000000000000000, 0.000000000000000000, 0.000000000000000000 ) ) ;
#34887 = AXIS2_PLACEMENT_3D ( 'NONE', #42465, #26129, #19810 ) ;
#34888 = CARTESIAN_POINT ( 'NONE',  ( 18.00000000000000355, 35.11945359308163006, -38.34871548465977753 ) ) ;
#34889 = ORIENTED_EDGE ( 'NONE', *, *, #42114, .T. ) ;
#34890 = CARTESIAN_POINT ( 'NONE',  ( 64.78932475141161262, 39.99999999999999289, 8.528958657501300777 ) ) ;
#34891 = CARTESIAN_POINT ( 'NONE',  ( 17.99999999999999645, -40.13512380274045199, 113.6206972269520179 ) ) ;
#34892 = AXIS2_PLACEMENT_3D ( 'NONE', #22651, #39384, #16090 ) ;
#34893 = CIRCLE ( 'NONE', #734, 58.99999999999999289 ) ;
#34894 = ORIENTED_EDGE ( 'NONE', *, *, #22618, .F. ) ;
#34895 = CIRCLE ( 'NONE', #16012, 2.649999999999971934 ) ;
#34896 = LINE ( 'NONE', #1508, #19693 ) ;
#34897 = CYLINDRICAL_SURFACE ( 'NONE', #40984, 116.0000000000000000 ) ;
#34898 = ADVANCED_FACE ( 'NONE', ( #34393 ), #34616, .T. ) ;
#34899 = EDGE_CURVE ( 'NONE', #30887, #5278, #38104, .T. ) ;
#34900 = AXIS2_PLACEMENT_3D ( 'NONE', #24855, #38526, #17659 ) ;
#34901 = ORIENTED_EDGE ( 'NONE', *, *, #24395, .T. ) ;
#34902 = DIRECTION ( 'NONE',  ( 0.000000000000000000, 0.000000000000000000, 1.000000000000000000 ) ) ;
#34903 = ORIENTED_EDGE ( 'NONE', *, *, #28712, .T. ) ;
#34904 = EDGE_CURVE ( 'NONE', #3569, #32160, #35969, .T. ) ;
#34905 = LINE ( 'NONE', #28806, #7229 ) ;
#34906 = ORIENTED_EDGE ( 'NONE', *, *, #38569, .T. ) ;
#34907 = VECTOR ( 'NONE', #5460, 1000.000000000000000 ) ;
#34908 = DIRECTION ( 'NONE',  ( -1.000000000000000000, 0.000000000000000000, 0.000000000000000000 ) ) ;
#34909 = CARTESIAN_POINT ( 'NONE',  ( 17.99999999999999645, -82.63181128086789329, 81.41243003646944487 ) ) ;
#34910 = CARTESIAN_POINT ( 'NONE',  ( 17.99999999999999645, 83.58328028049768932, -80.43528614701241963 ) ) ;
#34911 = DIRECTION ( 'NONE',  ( 0.000000000000000000, 0.000000000000000000, -1.000000000000000000 ) ) ;
#34912 = ORIENTED_EDGE ( 'NONE', *, *, #20866, .F. ) ;
#34913 = CYLINDRICAL_SURFACE ( 'NONE', #1524, 59.00000000000000000 ) ;
#34914 = DIRECTION ( 'NONE',  ( 0.000000000000000000, -0.8993121301712143634, -0.4373073204588656115 ) ) ;
#34915 = EDGE_CURVE ( 'NONE', #16293, #34548, #40168, .T. ) ;
#34916 = ORIENTED_EDGE ( 'NONE', *, *, #20884, .T. ) ;
#34917 = CARTESIAN_POINT ( 'NONE',  ( 0.000000000000000000, -47.22458491092815791, -5.098390039074710778 ) ) ;
#34918 = AXIS2_PLACEMENT_3D ( 'NONE', #24387, #28073, #4468 ) ;
#34919 = DIRECTION ( 'NONE',  ( 0.000000000000000000, 0.000000000000000000, 1.000000000000000000 ) ) ;
#34920 = PRODUCT_CONTEXT ( 'NONE', #41755, 'mechanical' ) ;
#34921 = CARTESIAN_POINT ( 'NONE',  ( 0.000000000000000000, -97.19627249181046125, -71.22763238166585609 ) ) ;
#34922 = CARTESIAN_POINT ( 'NONE',  ( 40.56819808336118882, 31.00000000000000355, -35.59309480518532354 ) ) ;
#34923 = CIRCLE ( 'NONE', #1460, 2.649999999999957723 ) ;
#34924 = ORIENTED_EDGE ( 'NONE', *, *, #32604, .T. ) ;
#34926 = CARTESIAN_POINT ( 'NONE',  ( 150.4999999999986926, 1.396217360982896810E-12, 9.999999999999960920 ) ) ;
#34925 = CARTESIAN_POINT ( 'NONE',  ( 0.000000000000000000, 64.58410930313661424, -101.7319213743675732 ) ) ;
#34927 = AXIS2_PLACEMENT_3D ( 'NONE', #2830, #38865, #16194 ) ;
#34928 = ORIENTED_EDGE ( 'NONE', *, *, #19068, .T. ) ;
#34929 = AXIS2_PLACEMENT_3D ( 'NONE', #28957, #22004, #12163 ) ;
#34930 = EDGE_CURVE ( 'NONE', #13563, #8001, #31834, .T. ) ;
#34931 = CARTESIAN_POINT ( 'NONE',  ( 34.44467569804516671, 40.00000000000000000, 44.88666365967159777 ) ) ;
#34932 = CARTESIAN_POINT ( 'NONE',  ( 43.74200748489512591, 40.00000000000000000, 38.49442098324160355 ) ) ;
#34933 = AXIS2_PLACEMENT_3D ( 'NONE', #39334, #32385, #29141 ) ;
#34934 = DIRECTION ( 'NONE',  ( 0.000000000000000000, 0.000000000000000000, 1.000000000000000000 ) ) ;
#34935 = CARTESIAN_POINT ( 'NONE',  ( 17.99999999999999645, -113.8630351447204134, -22.16324045874526405 ) ) ;
#34936 = DIRECTION ( 'NONE',  ( 1.000000000000000000, 0.000000000000000000, 0.000000000000000000 ) ) ;
#34937 = CARTESIAN_POINT ( 'NONE',  ( 21.81281596512078025, 31.00000000000000355, -10.76194779073239083 ) ) ;
#34938 = VERTEX_POINT ( 'NONE', #2923 ) ;
#34939 = CARTESIAN_POINT ( 'NONE',  ( -28.96462450050677973, 40.00000000000000000, -9.827991688575851370 ) ) ;
#34940 = ORIENTED_EDGE ( 'NONE', *, *, #36502, .T. ) ;
#34941 = CYLINDRICAL_SURFACE ( 'NONE', #18801, 59.00000000000000000 ) ;
#34942 = DIRECTION ( 'NONE',  ( -1.000000000000000000, 0.000000000000000000, 0.000000000000000000 ) ) ;
#34943 = ORIENTED_EDGE ( 'NONE', *, *, #10444, .T. ) ;
#34944 = CARTESIAN_POINT ( 'NONE',  ( 17.99999999999999645, 24.22031524826126514, -109.5520369638034879 ) ) ;
#34945 = EDGE_CURVE ( 'NONE', #27962, #39003, #39593, .T. ) ;
#34946 = CARTESIAN_POINT ( 'NONE',  ( 17.99999999999999645, 29.36437154452156761, -116.8684075565133043 ) ) ;
#34947 = ORIENTED_EDGE ( 'NONE', *, *, #34192, .F. ) ;
#34948 = CARTESIAN_POINT ( 'NONE',  ( 2.500000000000000000, -1.178949249685214307, 2.042000000000001592 ) ) ;
#34949 = ORIENTED_EDGE ( 'NONE', *, *, #25958, .F. ) ;
#34950 = AXIS2_PLACEMENT_3D ( 'NONE', #37585, #31490, #18012 ) ;
#34951 = ORIENTED_EDGE ( 'NONE', *, *, #7947, .T. ) ;
#34952 = LINE ( 'NONE', #5063, #38962 ) ;
#34953 = AXIS2_PLACEMENT_3D ( 'NONE', #24872, #28115, #25092 ) ;
#34954 = CARTESIAN_POINT ( 'NONE',  ( 44.33290732825512492, 31.00000000000000355, 77.00207852755224280 ) ) ;
#34955 = ORIENTED_EDGE ( 'NONE', *, *, #12294, .T. ) ;
#34956 = DIRECTION ( 'NONE',  ( -1.000000000000000000, -0.000000000000000000, -0.000000000000000000 ) ) ;
#34957 = AXIS2_PLACEMENT_3D ( 'NONE', #26638, #39483, #25998 ) ;
#34958 = DIRECTION ( 'NONE',  ( -1.000000000000000000, 0.000000000000000000, -0.000000000000000000 ) ) ;
#34959 = ORIENTED_EDGE ( 'NONE', *, *, #34799, .F. ) ;
#34960 = EDGE_CURVE ( 'NONE', #40092, #32698, #4654, .T. ) ;
#34961 = CARTESIAN_POINT ( 'NONE',  ( -4.204015924366189871, 1.626724848190922446, -3.610627190413390419 ) ) ;
#34962 = ORIENTED_EDGE ( 'NONE', *, *, #18885, .F. ) ;
#34963 = CARTESIAN_POINT ( 'NONE',  ( 0.000000000000000000, -8.827181066045094227, -120.1772519049560231 ) ) ;
#34964 = AXIS2_PLACEMENT_3D ( 'NONE', #23039, #26070, #3336 ) ;
#34965 = CARTESIAN_POINT ( 'NONE',  ( -22.10416666678001008, 31.00000000000000355, -1.441157586896874898 ) ) ;
#34966 = EDGE_CURVE ( 'NONE', #29868, #6044, #5588, .T. ) ;
#34968 = FACE_BOUND ( 'NONE', #26451, .T. ) ;
#34967 = CARTESIAN_POINT ( 'NONE',  ( 50.00005079999999680, 0.000000000000000000, 0.000000000000000000 ) ) ;
#34969 = CARTESIAN_POINT ( 'NONE',  ( 17.99999999999999645, 0.000000000000000000, 0.000000000000000000 ) ) ;
#34970 = DIRECTION ( 'NONE',  ( -1.000000000000000000, 0.000000000000000000, -0.000000000000000000 ) ) ;
#34971 = ORIENTED_EDGE ( 'NONE', *, *, #42992, .T. ) ;
#34972 = PRESENTATION_STYLE_ASSIGNMENT (( #15369 ) ) ;
#34973 = FACE_OUTER_BOUND ( 'NONE', #11114, .T. ) ;
#34974 = VERTEX_POINT ( 'NONE', #9509 ) ;
#34975 = DIRECTION ( 'NONE',  ( 0.000000000000000000, -0.9996456111234522934, -0.02662052143778445568 ) ) ;
#34976 = CARTESIAN_POINT ( 'NONE',  ( -99.89583333318432778, 31.00000000000000711, 6.544984695199788760 ) ) ;
#34977 = DIRECTION ( 'NONE',  ( -1.000000000000000000, -0.000000000000000000, -0.000000000000000000 ) ) ;
#34978 = VERTEX_POINT ( 'NONE', #2286 ) ;
#34979 = CARTESIAN_POINT ( 'NONE',  ( 26.89767027507547326, 40.00000000000000000, -1.736414864505229305 ) ) ;
#34980 = CIRCLE ( 'NONE', #31538, 120.5010000000000190 ) ;
#34982 = EDGE_CURVE ( 'NONE', #36319, #6919, #29065, .T. ) ;
#34981 = CIRCLE ( 'NONE', #21805, 120.5010000000000190 ) ;
#34983 = VERTEX_POINT ( 'NONE', #32206 ) ;
#34984 = AXIS2_PLACEMENT_3D ( 'NONE', #7309, #33713, #3800 ) ;
#34985 = ORIENTED_EDGE ( 'NONE', *, *, #32134, .T. ) ;
#34986 = DIRECTION ( 'NONE',  ( 1.000000000000000000, 0.000000000000000000, 0.000000000000000000 ) ) ;
#34987 = CARTESIAN_POINT ( 'NONE',  ( 0.000000000000000000, 0.7408941433508176022, 0.000000000000000000 ) ) ;
#34988 = DIRECTION ( 'NONE',  ( -1.000000000000000000, -0.000000000000000000, -0.000000000000000000 ) ) ;
#34989 = AXIS2_PLACEMENT_3D ( 'NONE', #42701, #16344, #13087 ) ;
#34990 = DIRECTION ( 'NONE',  ( 0.000000000000000000, 0.9968120070307499025, 0.07978610555308651708 ) ) ;
#34991 = ORIENTED_EDGE ( 'NONE', *, *, #37683, .F. ) ;
#34992 = CARTESIAN_POINT ( 'NONE',  ( 9.000000000000001776, 29.86146781000101669, -112.0905559814575696 ) ) ;
#34993 = ORIENTED_EDGE ( 'NONE', *, *, #40623, .T. ) ;
#34994 = CARTESIAN_POINT ( 'NONE',  ( 17.99999999999999645, 10.40101730206366959, 120.0512800434971581 ) ) ;
#34995 = CIRCLE ( 'NONE', #19008, 116.0000000000000000 ) ;
#34996 = CARTESIAN_POINT ( 'NONE',  ( 17.99999999999999645, -101.1249659627859216, 48.60055280209385842 ) ) ;
#34997 = DIRECTION ( 'NONE',  ( -1.000000000000000000, -0.000000000000000000, 0.000000000000000000 ) ) ;
#34998 = CARTESIAN_POINT ( 'NONE',  ( 18.00000000000000355, 0.000000000000000000, 0.000000000000000000 ) ) ;
#34999 = ORIENTED_EDGE ( 'NONE', *, *, #15661, .F. ) ;
#35000 = ORIENTED_EDGE ( 'NONE', *, *, #2376, .F. ) ;
#35001 = CARTESIAN_POINT ( 'NONE',  ( 17.99999999999999645, -35.72777019205738469, 106.3569410558016273 ) ) ;
#35002 = ADVANCED_FACE ( 'NONE', ( #25703 ), #38953, .T. ) ;
#35003 = LINE ( 'NONE', #25030, #1199 ) ;
#35004 = VERTEX_POINT ( 'NONE', #6435 ) ;
#35006 = VERTEX_POINT ( 'NONE', #9284 ) ;
#35005 = PLANE ( 'NONE',  #20872 ) ;
#35007 = CARTESIAN_POINT ( 'NONE',  ( 44.12914893500597202, 31.00000000000000355, -14.89880614700436112 ) ) ;
#35008 = VERTEX_POINT ( 'NONE', #26324 ) ;
#35009 = DIRECTION ( 'NONE',  ( 1.000000000000000000, -3.035766082959412415E-17, 0.000000000000000000 ) ) ;
#35010 = EDGE_CURVE ( 'NONE', #36814, #276, #33214, .T. ) ;
#35012 = DIRECTION ( 'NONE',  ( -1.000000000000000000, 0.000000000000000000, -0.000000000000000000 ) ) ;
#35011 = CARTESIAN_POINT ( 'NONE',  ( 0.000000000000000000, 84.77518783075095143, 73.49448960231384831 ) ) ;
#35013 = ORIENTED_EDGE ( 'NONE', *, *, #11477, .F. ) ;
#35014 = AXIS2_PLACEMENT_3D ( 'NONE', #8032, #34864, #28126 ) ;
#35015 = FACE_OUTER_BOUND ( 'NONE', #4561, .T. ) ;
#35016 = CARTESIAN_POINT ( 'NONE',  ( -15.62887661519555493, 40.00000000000000000, 57.97203279869352599 ) ) ;
#35017 = AXIS2_PLACEMENT_3D ( 'NONE', #32678, #10412, #3410 ) ;
#35018 = ADVANCED_FACE ( 'NONE', ( #9073, #6228 ), #35676, .T. ) ;
#35019 = CYLINDRICAL_SURFACE ( 'NONE', #26277, 59.00000000000001421 ) ;
#35020 = CIRCLE ( 'NONE', #13458, 116.0000000000000000 ) ;
#35021 = CARTESIAN_POINT ( 'NONE',  ( 17.99999999999999645, -68.63002662989811142, 93.51962064069482494 ) ) ;
#35022 = ORIENTED_EDGE ( 'NONE', *, *, #2813, .T. ) ;
#35023 = CARTESIAN_POINT ( 'NONE',  ( 0.000000000000000000, -91.51415974874549875, -64.91094698989387268 ) ) ;
#35024 = ORIENTED_EDGE ( 'NONE', *, *, #9472, .T. ) ;
#35025 = AXIS2_PLACEMENT_3D ( 'NONE', #9155, #15524, #12462 ) ;
#35026 = CARTESIAN_POINT ( 'NONE',  ( 18.00000000000000355, 0.000000000000000000, 0.000000000000000000 ) ) ;
#35027 = CARTESIAN_POINT ( 'NONE',  ( 17.99999999999999645, 0.000000000000000000, 0.000000000000000000 ) ) ;
#35028 = CARTESIAN_POINT ( 'NONE',  ( -18.69663849766352826, 31.00000000000000355, -69.77653669617104981 ) ) ;
#35029 = DIRECTION ( 'NONE',  ( 0.000000000000000000, 0.000000000000000000, 1.000000000000000000 ) ) ;
#35030 = ORIENTED_EDGE ( 'NONE', *, *, #32913, .T. ) ;
#35031 = EDGE_CURVE ( 'NONE', #22633, #26052, #35300, .T. ) ;
#35032 = EDGE_LOOP ( 'NONE', ( #1214, #11303, #5810, #19059 ) ) ;
#35033 = DIRECTION ( 'NONE',  ( 0.000000000000000000, 0.000000000000000000, -1.000000000000000000 ) ) ;
#35034 = ADVANCED_FACE ( 'NONE', ( #28743 ), #42642, .F. ) ;
#35035 = DIRECTION ( 'NONE',  ( -1.734723475976807834E-16, 1.000000000000000000, 0.000000000000000000 ) ) ;
#35036 = CARTESIAN_POINT ( 'NONE',  ( -21.69137426901471954, 31.00000000000000355, -81.42030341110597647 ) ) ;
#35037 = CARTESIAN_POINT ( 'NONE',  ( -55.31949386280459180, 40.00000000000000711, 71.91600076662652441 ) ) ;
#35038 = DIRECTION ( 'NONE',  ( 0.000000000000000000, 0.000000000000000000, 1.000000000000000000 ) ) ;
#35039 = AXIS2_PLACEMENT_3D ( 'NONE', #40264, #10835, #556 ) ;
#35040 = VERTEX_POINT ( 'NONE', #42219 ) ;
#35041 = DIRECTION ( 'NONE',  ( 0.000000000000000000, -0.8477344278896755680, 0.5304209081197350795 ) ) ;
#35042 = ORIENTED_EDGE ( 'NONE', *, *, #612, .F. ) ;
#35043 = CARTESIAN_POINT ( 'NONE',  ( 0.000000000000000000, 46.87740477351718482, -3.172455868805370560 ) ) ;
#35045 = VERTEX_POINT ( 'NONE', #32418 ) ;
#35044 = DIRECTION ( 'NONE',  ( -1.000000000000000000, 0.000000000000000000, -0.000000000000000000 ) ) ;
#35046 = CARTESIAN_POINT ( 'NONE',  ( 17.99999999999999645, -29.03409033315590904, 12.21509719675380623 ) ) ;
#35047 = EDGE_LOOP ( 'NONE', ( #34514, #12085, #18733, #8136 ) ) ;
#35048 = CARTESIAN_POINT ( 'NONE',  ( 0.000000000000000000, 0.000000000000000000, 0.000000000000000000 ) ) ;
#35049 =( GEOMETRIC_REPRESENTATION_CONTEXT ( 3 ) GLOBAL_UNCERTAINTY_ASSIGNED_CONTEXT ( ( #12029 ) ) GLOBAL_UNIT_ASSIGNED_CONTEXT ( ( #3755, #9480, #29561 ) ) REPRESENTATION_CONTEXT ( 'NONE', 'WORKASPACE' ) );
#35050 = DIRECTION ( 'NONE',  ( -1.000000000000000000, -0.000000000000000000, -0.000000000000000000 ) ) ;
#35051 = CIRCLE ( 'NONE', #39887, 20.00000000000000355 ) ;
#35052 = ORIENTED_EDGE ( 'NONE', *, *, #26767, .F. ) ;
#35053 = LINE ( 'NONE', #34627, #33889 ) ;
#35054 = CARTESIAN_POINT ( 'NONE',  ( 17.99999999999999645, -107.1354928292872728, 44.47455650398029547 ) ) ;
#35055 = ADVANCED_FACE ( 'NONE', ( #38741 ), #12159, .T. ) ;
#35057 = DIRECTION ( 'NONE',  ( 0.000000000000000000, 0.000000000000000000, -1.000000000000000000 ) ) ;
#35056 = DIRECTION ( 'NONE',  ( -3.996523416598930318E-16, 2.658563593772947863E-15, 1.000000000000000000 ) ) ;
#35058 = VERTEX_POINT ( 'NONE', #19366 ) ;
#35059 = LINE ( 'NONE', #8888, #17787 ) ;
#35060 = ORIENTED_EDGE ( 'NONE', *, *, #792, .T. ) ;
#35061 = DIRECTION ( 'NONE',  ( -1.000000000000000000, -0.000000000000000000, -0.000000000000000000 ) ) ;
#35062 = CARTESIAN_POINT ( 'NONE',  ( 36.89914868738106435, 40.00000000000000000, -2.354335741662294978 ) ) ;
#35063 = DIRECTION ( 'NONE',  ( -1.000000000000000000, -0.000000000000000000, -0.000000000000000000 ) ) ;
#35064 = EDGE_CURVE ( 'NONE', #42813, #18280, #17255, .T. ) ;
#35065 = DIRECTION ( 'NONE',  ( -1.000000000000000000, 0.000000000000000000, 0.000000000000000000 ) ) ;
#35066 = CIRCLE ( 'NONE', #19101, 116.0000000000000000 ) ;
#35067 = ADVANCED_FACE ( 'NONE', ( #25902 ), #5793, .F. ) ;
#35068 = DIRECTION ( 'NONE',  ( 0.000000000000000000, -0.9714298932647122964, 0.2373266998711056064 ) ) ;
#35069 = VERTEX_POINT ( 'NONE', #16078 ) ;
#35070 = DIRECTION ( 'NONE',  ( 0.000000000000000000, 0.8477344278896686847, 0.5304209081197462927 ) ) ;
#35071 = ORIENTED_EDGE ( 'NONE', *, *, #20552, .T. ) ;
#35072 = VECTOR ( 'NONE', #2811, 1000.000000000000000 ) ;
#35073 = DIRECTION ( 'NONE',  ( 1.000000000000000000, -0.000000000000000000, 0.000000000000000000 ) ) ;
#35074 = CARTESIAN_POINT ( 'NONE',  ( 0.000000000000000000, 0.000000000000000000, 0.000000000000000000 ) ) ;
#35075 = CARTESIAN_POINT ( 'NONE',  ( -2.454369252093152376, 31.00000000000000355, 37.60416666486730009 ) ) ;
#35076 = ORIENTED_EDGE ( 'NONE', *, *, #32583, .T. ) ;
#35077 = DIRECTION ( 'NONE',  ( -0.000000000000000000, -0.000000000000000000, -1.000000000000000000 ) ) ;
#35078 = MECHANICAL_DESIGN_GEOMETRIC_PRESENTATION_REPRESENTATION (  '', ( #42040 ), #12122 ) ;
#35079 = CARTESIAN_POINT ( 'NONE',  ( 0.000000000000000000, -73.78980555658671392, 95.26571049921966505 ) ) ;
#35080 = CARTESIAN_POINT ( 'NONE',  ( -34.66105084696506822, 31.00000000000000355, 70.31756248751102589 ) ) ;
#35081 = VECTOR ( 'NONE', #9314, 1000.000000000000000 ) ;
#35082 = EDGE_CURVE ( 'NONE', #20186, #23198, #18677, .T. ) ;
#35083 = EDGE_CURVE ( 'NONE', #17013, #34048, #1880, .T. ) ;
#35084 = ORIENTED_EDGE ( 'NONE', *, *, #32844, .T. ) ;
#35085 = CARTESIAN_POINT ( 'NONE',  ( -51.46673616000524021, 31.00000000000000355, 6.691140578787329041 ) ) ;
#35086 = EDGE_CURVE ( 'NONE', #37209, #22175, #492, .T. ) ;
#35087 = EDGE_CURVE ( 'NONE', #5323, #13299, #13777, .T. ) ;
#35088 = CARTESIAN_POINT ( 'NONE',  ( -22.78857244739539212, 40.00000000000000000, 85.10612709700112077 ) ) ;
#35089 = AXIS2_PLACEMENT_3D ( 'NONE', #27293, #10699, #27958 ) ;
#35090 = EDGE_LOOP ( 'NONE', ( #42386, #6945, #10525, #2946 ) ) ;
#35091 = CARTESIAN_POINT ( 'NONE',  ( 106.4195705685763471, -106.4195705685744855, 9.999999999999998224 ) ) ;
#35092 = DIRECTION ( 'NONE',  ( -1.000000000000000000, -0.000000000000000000, -0.000000000000000000 ) ) ;
#35093 = CYLINDRICAL_SURFACE ( 'NONE', #31020, 13.40000000000000213 ) ;
#35094 = VECTOR ( 'NONE', #27708, 1000.000000000000000 ) ;
#35096 = ORIENTED_EDGE ( 'NONE', *, *, #8182, .T. ) ;
#35095 = CARTESIAN_POINT ( 'NONE',  ( 0.000000000000000000, -117.9424311864590891, 24.69967462998996766 ) ) ;
#35097 = CARTESIAN_POINT ( 'NONE',  ( 0.000000000000000000, 114.6488492393084613, -37.09625815499892809 ) ) ;
#35098 = CYLINDRICAL_SURFACE ( 'NONE', #36941, 20.00000000000000355 ) ;
#35099 = ORIENTED_EDGE ( 'NONE', *, *, #6677, .T. ) ;
#35100 = CARTESIAN_POINT ( 'NONE',  ( -41.80404827410195168, 40.00000000000000000, 54.50178954758867889 ) ) ;
#35101 = CARTESIAN_POINT ( 'NONE',  ( 18.00000000000000355, -46.87740477351715640, -3.172455868805708956 ) ) ;
#35102 = VERTEX_POINT ( 'NONE', #6871 ) ;
#35103 = DIRECTION ( 'NONE',  ( 0.000000000000000000, 0.000000000000000000, 1.000000000000000000 ) ) ;
#35104 = LINE ( 'NONE', #19377, #20900 ) ;
#35105 = DIRECTION ( 'NONE',  ( 0.000000000000000000, 0.000000000000000000, 1.000000000000000000 ) ) ;
#35106 = VERTEX_POINT ( 'NONE', #3138 ) ;
#35107 = AXIS2_PLACEMENT_3D ( 'NONE', #7655, #7002, #21018 ) ;
#35108 = EDGE_CURVE ( 'NONE', #37953, #39739, #24956, .T. ) ;
#35109 = ORIENTED_EDGE ( 'NONE', *, *, #9272, .T. ) ;
#35110 = DIRECTION ( 'NONE',  ( 1.000000000000000000, 0.000000000000000000, 0.000000000000000000 ) ) ;
#35111 = AXIS2_PLACEMENT_3D ( 'NONE', #28079, #772, #1213 ) ;
#35112 = ORIENTED_EDGE ( 'NONE', *, *, #33882, .F. ) ;
#35113 = DIRECTION ( 'NONE',  ( -0.000000000000000000, 1.287488025362403787E-15, 1.000000000000000000 ) ) ;
#35114 = CYLINDRICAL_SURFACE ( 'NONE', #10212, 2.799122904894268071 ) ;
#35115 = ADVANCED_FACE ( 'NONE', ( #7290 ), #735, .F. ) ;
#35116 = DIRECTION ( 'NONE',  ( -1.000000000000000000, -0.000000000000000000, -0.000000000000000000 ) ) ;
#35117 = DIRECTION ( 'NONE',  ( 0.000000000000000000, 0.000000000000000000, 1.000000000000000000 ) ) ;
#35119 = ORIENTED_EDGE ( 'NONE', *, *, #28483, .F. ) ;
#35118 = CIRCLE ( 'NONE', #39981, 59.00000000000000000 ) ;
#35120 = CARTESIAN_POINT ( 'NONE',  ( -10.00000000000000000, 0.000000000000000000, 0.000000000000000000 ) ) ;
#35121 = CARTESIAN_POINT ( 'NONE',  ( 22.90854556226710415, -12.05525454449572997, -74.83297477053821467 ) ) ;
#35122 = ORIENTED_EDGE ( 'NONE', *, *, #17978, .T. ) ;
#35123 = CARTESIAN_POINT ( 'NONE',  ( 17.99999999999999645, 0.000000000000000000, 0.000000000000000000 ) ) ;
#35124 = VECTOR ( 'NONE', #13698, 1000.000000000000000 ) ;
#35125 = DIRECTION ( 'NONE',  ( -1.000000000000000000, 0.000000000000000000, 0.000000000000000000 ) ) ;
#35126 = APPLICATION_PROTOCOL_DEFINITION ( 'draft international standard', 'automotive_design', 1998, #37852 ) ;
#35128 = CIRCLE ( 'NONE', #14226, 2.649999999999971934 ) ;
#35127 = DIRECTION ( 'NONE',  ( 0.9470131699890049770, 1.701542661702850483E-16, 0.3211947320043963550 ) ) ;
#35129 = CARTESIAN_POINT ( 'NONE',  ( -3.436116956419240864, 31.00000000000000355, -52.39583333462812931 ) ) ;
#35130 = ORIENTED_EDGE ( 'NONE', *, *, #25310, .T. ) ;
#35132 = CARTESIAN_POINT ( 'NONE',  ( 0.000000000000000000, -6.007673836297746206, -35.49518073030003507 ) ) ;
#35131 = DIRECTION ( 'NONE',  ( 0.000000000000000000, 0.000000000000000000, 1.000000000000000000 ) ) ;
#35133 = ADVANCED_FACE ( 'NONE', ( #10368 ), #33488, .F. ) ;
#35134 = EDGE_CURVE ( 'NONE', #29671, #33221, #15865, .T. ) ;
#35135 = VERTEX_POINT ( 'NONE', #40654 ) ;
#35136 = ADVANCED_FACE ( 'NONE', ( #33049 ), #3572, .T. ) ;
#35137 = EDGE_CURVE ( 'NONE', #9970, #27084, #35333, .T. ) ;
#35138 = CARTESIAN_POINT ( 'NONE',  ( 54.85378563033546584, 40.00000000000000000, 7.219977902337870290 ) ) ;
#35139 = EDGE_CURVE ( 'NONE', #9697, #36354, #32559, .T. ) ;
#35140 = AXIS2_PLACEMENT_3D ( 'NONE', #20805, #21023, #34275 ) ;
#35141 = CARTESIAN_POINT ( 'NONE',  ( 150.4999999999986926, 1.396217360982896810E-12, 9.999999999999962697 ) ) ;
#35142 = CARTESIAN_POINT ( 'NONE',  ( -10.00000000000000000, 0.000000000000000000, 0.000000000000000000 ) ) ;
#35143 = CARTESIAN_POINT ( 'NONE',  ( 0.000000000000000000, -90.81729652456213842, 72.16798910853589177 ) ) ;
#35144 = AXIS2_PLACEMENT_3D ( 'NONE', #15668, #42024, #22016 ) ;
#35145 = CARTESIAN_POINT ( 'NONE',  ( -18.63466726053507472, 31.00000000000000355, -9.179856479542758407 ) ) ;
#35146 = AXIS2_PLACEMENT_3D ( 'NONE', #33132, #26811, #43154 ) ;
#35147 = ORIENTED_EDGE ( 'NONE', *, *, #7064, .T. ) ;
#35148 = CARTESIAN_POINT ( 'NONE',  ( 2.127120017302678523, 40.00000000000000000, -32.60416666460785962 ) ) ;
#35149 = VERTEX_POINT ( 'NONE', #17162 ) ;
#35150 = CARTESIAN_POINT ( 'NONE',  ( 18.00000000000000355, 38.92705108641732892, 27.21837053747810842 ) ) ;
#35151 = CARTESIAN_POINT ( 'NONE',  ( -0.5276280594146446346, 4.314175951381965746, -3.320322319201721495 ) ) ;
#35152 = ORIENTED_EDGE ( 'NONE', *, *, #3083, .F. ) ;
#35153 = CARTESIAN_POINT ( 'NONE',  ( 17.99999999999999645, 6.486220790509957368, -112.0098273076986715 ) ) ;
#35154 = CARTESIAN_POINT ( 'NONE',  ( 17.99999999999999645, 0.000000000000000000, 0.000000000000000000 ) ) ;
#35155 = ORIENTED_EDGE ( 'NONE', *, *, #9446, .F. ) ;
#35156 = DIRECTION ( 'NONE',  ( -1.000000000000000000, -0.000000000000000000, -0.000000000000000000 ) ) ;
#35157 = ORIENTED_EDGE ( 'NONE', *, *, #4245, .F. ) ;
#35158 = AXIS2_PLACEMENT_3D ( 'NONE', #6920, #27230, #6709 ) ;
#35159 = ORIENTED_EDGE ( 'NONE', *, *, #31907, .F. ) ;
#35160 = DIRECTION ( 'NONE',  ( -0.9470131699890049770, 0.000000000000000000, -0.3211947320043963550 ) ) ;
#35161 = CARTESIAN_POINT ( 'NONE',  ( -78.26717753304431824, 31.00000000000000711, -26.69481836928899554 ) ) ;
#35162 = ORIENTED_EDGE ( 'NONE', *, *, #21835, .T. ) ;
#35163 = LINE ( 'NONE', #5282, #11272 ) ;
#35164 = CARTESIAN_POINT ( 'NONE',  ( 17.99999999999999645, 69.90696807222620635, -98.15042952503443985 ) ) ;
#35165 = ORIENTED_EDGE ( 'NONE', *, *, #36924, .T. ) ;
#35166 = CARTESIAN_POINT ( 'NONE',  ( 0.000000000000000000, 111.2721026680460596, -14.38025178762657852 ) ) ;
#35167 = DIRECTION ( 'NONE',  ( 1.000000000000000000, 0.000000000000000000, 0.000000000000000000 ) ) ;
#35168 = CARTESIAN_POINT ( 'NONE',  ( 16.96065435355024320, 31.00000000000000355, -19.31014141889295388 ) ) ;
#35170 = DIRECTION ( 'NONE',  ( 0.000000000000000000, 0.000000000000000000, -1.000000000000000000 ) ) ;
#35169 = DIRECTION ( 'NONE',  ( 0.000000000000000000, 0.2631025642275218179, -0.9647678688145158166 ) ) ;
#35171 = AXIS2_PLACEMENT_3D ( 'NONE', #38281, #3039, #33608 ) ;
#35172 = CARTESIAN_POINT ( 'NONE',  ( 17.99999999999999645, 0.000000000000000000, 0.000000000000000000 ) ) ;
#35173 = DIRECTION ( 'NONE',  ( 1.000000000000000000, 0.000000000000000000, 0.000000000000000000 ) ) ;
#35174 = VECTOR ( 'NONE', #18659, 1000.000000000000000 ) ;
#35175 = VERTEX_POINT ( 'NONE', #20012 ) ;
#35176 = AXIS2_PLACEMENT_3D ( 'NONE', #26176, #6297, #19647 ) ;
#35177 = DIRECTION ( 'NONE',  ( 1.000000000000000000, 0.000000000000000000, 0.000000000000000000 ) ) ;
#35178 = VERTEX_POINT ( 'NONE', #20433 ) ;
#35179 = CIRCLE ( 'NONE', #28243, 58.99999999999998579 ) ;
#35180 = DIRECTION ( 'NONE',  ( 0.000000000000000000, 0.9957341762950349118, -0.09226835946329871307 ) ) ;
#35181 = CARTESIAN_POINT ( 'NONE',  ( -25.38139813252123034, 31.00000000000000355, 94.78629358389331117 ) ) ;
#35182 = VECTOR ( 'NONE', #30155, 1000.000000000000000 ) ;
#35183 = DIRECTION ( 'NONE',  ( 0.000000000000000000, 0.000000000000000000, -1.000000000000000000 ) ) ;
#35184 = EDGE_LOOP ( 'NONE', ( #5854, #36363, #7836, #40889 ) ) ;
#35185 =( GEOMETRIC_REPRESENTATION_CONTEXT ( 3 ) GLOBAL_UNCERTAINTY_ASSIGNED_CONTEXT ( ( #27851 ) ) GLOBAL_UNIT_ASSIGNED_CONTEXT ( ( #39575, #29571, #35868 ) ) REPRESENTATION_CONTEXT ( 'NONE', 'WORKASPACE' ) );
#35186 = EDGE_CURVE ( 'NONE', #34791, #10990, #40204, .T. ) ;
#35187 = EDGE_CURVE ( 'NONE', #32376, #2948, #14098, .T. ) ;
#35188 = CARTESIAN_POINT ( 'NONE',  ( 11.33656872182470643, 40.00000000000000000, -33.21392199183605953 ) ) ;
#35189 = EDGE_CURVE ( 'NONE', #20926, #9697, #43084, .T. ) ;
#35190 = CIRCLE ( 'NONE', #310, 13.60000000000000142 ) ;
#35191 = VERTEX_POINT ( 'NONE', #39799 ) ;
#35192 = ORIENTED_EDGE ( 'NONE', *, *, #29821, .T. ) ;
#35193 = CARTESIAN_POINT ( 'NONE',  ( 17.99999999999999645, -106.5605152861907072, 56.26142179985788516 ) ) ;
#35194 = CARTESIAN_POINT ( 'NONE',  ( 17.99999999999999645, 112.1702510623870381, -2.471285140322999840 ) ) ;
#35195 = DIRECTION ( 'NONE',  ( 1.000000000000000000, 0.000000000000000000, 0.000000000000000000 ) ) ;
#35196 = CYLINDRICAL_SURFACE ( 'NONE', #31677, 59.00000000000000000 ) ;
#35197 = EDGE_CURVE ( 'NONE', #37254, #32443, #8867, .T. ) ;
#35198 = CARTESIAN_POINT ( 'NONE',  ( 17.99999999999999645, 105.3681574666264282, 38.54638589714925700 ) ) ;
#35199 = ORIENTED_EDGE ( 'NONE', *, *, #11291, .F. ) ;
#35200 = DIRECTION ( 'NONE',  ( 1.000000000000000000, 0.000000000000000000, 0.000000000000000000 ) ) ;
#35201 = VERTEX_POINT ( 'NONE', #9924 ) ;
#35202 = DIRECTION ( 'NONE',  ( 0.000000000000000000, -0.8993121301712141413, -0.4373073204588656671 ) ) ;
#35203 = CIRCLE ( 'NONE', #25499, 116.0000000000000000 ) ;
#35204 = FACE_OUTER_BOUND ( 'NONE', #18947, .T. ) ;
#35205 = EDGE_CURVE ( 'NONE', #29131, #8886, #22150, .T. ) ;
#35206 = AXIS2_PLACEMENT_3D ( 'NONE', #1204, #37427, #40259 ) ;
#35207 = DIRECTION ( 'NONE',  ( 0.000000000000000000, 0.000000000000000000, -1.000000000000000000 ) ) ;
#35208 = CARTESIAN_POINT ( 'NONE',  ( 17.99999999999999645, 0.000000000000000000, 0.000000000000000000 ) ) ;
#35209 = ORIENTED_EDGE ( 'NONE', *, *, #33326, .F. ) ;
#35210 = AXIS2_PLACEMENT_3D ( 'NONE', #8733, #25783, #35554 ) ;
#35211 = VERTEX_POINT ( 'NONE', #33281 ) ;
#35212 = AXIS2_PLACEMENT_3D ( 'NONE', #24046, #10943, #24488 ) ;
#35213 = DIRECTION ( 'NONE',  ( -0.000000000000000000, 0.000000000000000000, 1.000000000000000000 ) ) ;
#35214 = EDGE_LOOP ( 'NONE', ( #33205, #38629 ) ) ;
#35216 = VERTEX_POINT ( 'NONE', #3365 ) ;
#35215 = DIRECTION ( 'NONE',  ( -1.000000000000000000, 0.000000000000000000, 0.000000000000000000 ) ) ;
#35217 = CARTESIAN_POINT ( 'NONE',  ( 3.148395399070833989, 31.00000000000000355, 49.39975974383467872 ) ) ;
#35218 = AXIS2_PLACEMENT_3D ( 'NONE', #39402, #16314, #43115 ) ;
#35219 = ORIENTED_EDGE ( 'NONE', *, *, #22114, .F. ) ;
#35220 = CARTESIAN_POINT ( 'NONE',  ( -19.99999999999999645, 31.00000000000000355, 2.168407390121265812E-15 ) ) ;
#35221 = CIRCLE ( 'NONE', #342, 116.0000000000000000 ) ;
#35222 = CARTESIAN_POINT ( 'NONE',  ( 17.99999999999999645, 47.58001226230686598, -110.7096808509478763 ) ) ;
#35223 = VECTOR ( 'NONE', #1833, 1000.000000000000000 ) ;
#35224 = EDGE_LOOP ( 'NONE', ( #37090, #9162, #20387, #231 ) ) ;
#35225 = CARTESIAN_POINT ( 'NONE',  ( -72.09351246578157202, 40.00000000000000711, -4.825959690424619808 ) ) ;
#35226 = FACE_OUTER_BOUND ( 'NONE', #21297, .T. ) ;
#35227 = DIRECTION ( 'NONE',  ( 1.000000000000000000, 0.000000000000000000, -6.546126324440847704E-16 ) ) ;
#35228 = ORIENTED_EDGE ( 'NONE', *, *, #28857, .F. ) ;
#35229 = CARTESIAN_POINT ( 'NONE',  ( -105.9879088449591933, 40.00000000000000000, -0.3807199291576673361 ) ) ;
#35230 = ORIENTED_EDGE ( 'NONE', *, *, #8499, .T. ) ;
#35231 = LINE ( 'NONE', #12563, #17008 ) ;
#35232 = DIRECTION ( 'NONE',  ( -1.000000000000000000, 0.000000000000000000, 0.000000000000000000 ) ) ;
#35233 = CARTESIAN_POINT ( 'NONE',  ( 65.10416666562252885, 31.00000000000000000, 4.254240043327690124 ) ) ;
#35234 = CARTESIAN_POINT ( 'NONE',  ( 17.99999999999999645, -80.74349901498355564, -77.90224541347362219 ) ) ;
#35235 = AXIS2_PLACEMENT_3D ( 'NONE', #30846, #6846, #33461 ) ;
#35236 = ORIENTED_EDGE ( 'NONE', *, *, #9038, .T. ) ;
#35237 = EDGE_CURVE ( 'NONE', #8432, #16960, #3945, .T. ) ;
#35238 = AXIS2_PLACEMENT_3D ( 'NONE', #10889, #1261, #34643 ) ;
#35239 = CARTESIAN_POINT ( 'NONE',  ( 0.000000000000000000, -40.37724737310141165, 104.6802291180865865 ) ) ;
#35240 = AXIS2_PLACEMENT_3D ( 'NONE', #35402, #38025, #1806 ) ;
#35241 = ORIENTED_EDGE ( 'NONE', *, *, #42373, .T. ) ;
#35243 = CIRCLE ( 'NONE', #20653, 0.08000000000000020983 ) ;
#35242 = DIRECTION ( 'NONE',  ( -1.000000000000000000, -0.000000000000000000, -0.000000000000000000 ) ) ;
#35244 = CARTESIAN_POINT ( 'NONE',  ( 17.99999999999999645, 0.000000000000000000, 0.000000000000000000 ) ) ;
#35245 = CARTESIAN_POINT ( 'NONE',  ( 76.16439905407254685, 31.00000000000000000, 44.11546174421767574 ) ) ;
#35247 = CARTESIAN_POINT ( 'NONE',  ( 84.58694138809387653, 39.99999999999999289, 22.77597867319729374 ) ) ;
#35246 = CIRCLE ( 'NONE', #1071, 59.00000000000000000 ) ;
#35248 = EDGE_CURVE ( 'NONE', #15357, #19261, #28395, .T. ) ;
#35249 = CIRCLE ( 'NONE', #6689, 120.5010000000000190 ) ;
#35250 = CARTESIAN_POINT ( 'NONE',  ( 17.99999999999999645, -46.83041522348427321, -101.9567785075606139 ) ) ;
#35251 = EDGE_CURVE ( 'NONE', #1122, #29131, #14465, .T. ) ;
#35252 = VECTOR ( 'NONE', #7241, 1000.000000000000000 ) ;
#35253 = VERTEX_POINT ( 'NONE', #37826 ) ;
#35254 = DIRECTION ( 'NONE',  ( -1.000000000000000000, 0.000000000000000000, 0.000000000000000000 ) ) ;
#35255 = ORIENTED_EDGE ( 'NONE', *, *, #25766, .F. ) ;
#35256 = EDGE_CURVE ( 'NONE', #16155, #32590, #9552, .T. ) ;
#35257 = CARTESIAN_POINT ( 'NONE',  ( 17.99999999999999645, -112.1702510623870666, 2.471285140322257323 ) ) ;
#35259 = ORIENTED_EDGE ( 'NONE', *, *, #32134, .F. ) ;
#35258 = CARTESIAN_POINT ( 'NONE',  ( 18.00000000000000355, 3.840921266750508156, -47.34345070675165346 ) ) ;
#35260 = DIRECTION ( 'NONE',  ( 0.000000000000000000, -0.5877852522924802425, 0.8090169943749421222 ) ) ;
#35261 = ORIENTED_EDGE ( 'NONE', *, *, #7476, .T. ) ;
#35262 = LINE ( 'NONE', #26327, #1468 ) ;
#35263 = CYLINDRICAL_SURFACE ( 'NONE', #42272, 47.49900000000000233 ) ;
#35264 = DIRECTION ( 'NONE',  ( -1.000000000000000000, 0.000000000000000000, 0.000000000000000000 ) ) ;
#35265 = ORIENTED_EDGE ( 'NONE', *, *, #20759, .T. ) ;
#35266 = CARTESIAN_POINT ( 'NONE',  ( 25.13348990051749254, 31.00000000000000355, -8.510361017572021680 ) ) ;
#35267 = DIRECTION ( 'NONE',  ( -1.000000000000000000, -0.000000000000000000, -0.000000000000000000 ) ) ;
#35268 = AXIS2_PLACEMENT_3D ( 'NONE', #2415, #10006, #15783 ) ;
#35269 = AXIS2_PLACEMENT_3D ( 'NONE', #9406, #3868, #3652 ) ;
#35270 = AXIS2_PLACEMENT_3D ( 'NONE', #13045, #2529, #6456 ) ;
#35271 = EDGE_CURVE ( 'NONE', #3223, #24128, #19365, .T. ) ;
#35272 = AXIS2_PLACEMENT_3D ( 'NONE', #8856, #38510, #35664 ) ;
#35274 = CARTESIAN_POINT ( 'NONE',  ( 8.999999999999998224, 37.07968990261482389, 109.9140418541958724 ) ) ;
#35273 = DIRECTION ( 'NONE',  ( -1.000000000000000000, 0.000000000000000000, -0.000000000000000000 ) ) ;
#35275 = ORIENTED_EDGE ( 'NONE', *, *, #4766, .F. ) ;
#35276 = CARTESIAN_POINT ( 'NONE',  ( 0.000000000000000000, -16.77727049691128869, 27.19001440037539297 ) ) ;
#35277 = EDGE_CURVE ( 'NONE', #1814, #35938, #31865, .T. ) ;
#35278 = CYLINDRICAL_SURFACE ( 'NONE', #25919, 13.59999999999999964 ) ;
#35279 = CARTESIAN_POINT ( 'NONE',  ( -5.264430561742839743, 40.00000000000000000, 39.44269128746232411 ) ) ;
#35280 = VECTOR ( 'NONE', #31945, 1000.000000000000000 ) ;
#35281 = DIRECTION ( 'NONE',  ( -1.000000000000000000, -0.000000000000000000, 0.000000000000000000 ) ) ;
#35282 = EDGE_CURVE ( 'NONE', #26486, #36379, #14299, .T. ) ;
#35283 = AXIS2_PLACEMENT_3D ( 'NONE', #38564, #4995, #12427 ) ;
#35284 = CARTESIAN_POINT ( 'NONE',  ( 31.80287614962791665, -40.05525454449572464, 69.29271901957253021 ) ) ;
#35285 = DIRECTION ( 'NONE',  ( 0.000000000000000000, 0.8951632913550604531, 0.4457383557765421944 ) ) ;
#35286 = ORIENTED_EDGE ( 'NONE', *, *, #22427, .T. ) ;
#35287 = CARTESIAN_POINT ( 'NONE',  ( 17.99999999999999645, 0.000000000000000000, 0.000000000000000000 ) ) ;
#35289 = VERTEX_POINT ( 'NONE', #11458 ) ;
#35288 = AXIS2_PLACEMENT_3D ( 'NONE', #41371, #8010, #11520 ) ;
#35290 = LINE ( 'NONE', #40967, #2252 ) ;
#35291 = CARTESIAN_POINT ( 'NONE',  ( 18.00000000000000355, 35.20873326984080620, 31.88259874184042886 ) ) ;
#35292 = CARTESIAN_POINT ( 'NONE',  ( 16.69935377588158332, 31.00000000000000355, -28.93150767131472989 ) ) ;
#35293 = VERTEX_POINT ( 'NONE', #1832 ) ;
#35294 = CARTESIAN_POINT ( 'NONE',  ( -10.00000000000000000, 0.000000000000000000, 0.000000000000000000 ) ) ;
#35295 = ORIENTED_EDGE ( 'NONE', *, *, #26767, .T. ) ;
#35296 = VECTOR ( 'NONE', #43063, 1000.000000000000114 ) ;
#35297 = EDGE_CURVE ( 'NONE', #10495, #11938, #39482, .T. ) ;
#35298 = LINE ( 'NONE', #21623, #29599 ) ;
#35299 = CARTESIAN_POINT ( 'NONE',  ( 36.87680687886029318, 31.00000000000000355, -74.81172728975037955 ) ) ;
#35301 = ORIENTED_EDGE ( 'NONE', *, *, #874, .T. ) ;
#35300 = CIRCLE ( 'NONE', #38780, 59.00000000000001421 ) ;
#35302 = CARTESIAN_POINT ( 'NONE',  ( 7.251580242022521716, 31.00000000000000355, -54.34182998361462325 ) ) ;
#35303 = CARTESIAN_POINT ( 'NONE',  ( 41.30831894254264824, 40.00000000000000000, -83.80005689411834169 ) ) ;
#35304 = VECTOR ( 'NONE', #24158, 1000.000000000000000 ) ;
#35305 = CIRCLE ( 'NONE', #16527, 59.00000000000000711 ) ;
#35306 = ADVANCED_FACE ( 'NONE', ( #40882 ), #24575, .T. ) ;
#35307 = ORIENTED_EDGE ( 'NONE', *, *, #18377, .T. ) ;
#35308 = CIRCLE ( 'NONE', #20718, 22.99999999999987921 ) ;
#35309 = DIRECTION ( 'NONE',  ( -1.000000000000000000, -0.000000000000000000, -0.000000000000000000 ) ) ;
#35310 = DIRECTION ( 'NONE',  ( 0.000000000000000000, 0.000000000000000000, 1.000000000000000000 ) ) ;
#35311 = EDGE_CURVE ( 'NONE', #2440, #16214, #15167, .T. ) ;
#35312 = CARTESIAN_POINT ( 'NONE',  ( -10.00000000000000000, 0.000000000000000000, 0.000000000000000000 ) ) ;
#35313 = VECTOR ( 'NONE', #40933, 1000.000000000000000 ) ;
#35315 = ORIENTED_EDGE ( 'NONE', *, *, #18863, .F. ) ;
#35314 = CARTESIAN_POINT ( 'NONE',  ( -19.99999999999999645, 40.00000000000000000, 1.283214542831033755 ) ) ;
#35316 = CARTESIAN_POINT ( 'NONE',  ( 17.99999999999999645, 103.1672962317651496, 44.09967643725903486 ) ) ;
#35317 = LINE ( 'NONE', #1502, #40421 ) ;
#35318 = AXIS2_PLACEMENT_3D ( 'NONE', #14866, #10488, #23827 ) ;
#35319 = ORIENTED_EDGE ( 'NONE', *, *, #24444, .T. ) ;
#35320 = CARTESIAN_POINT ( 'NONE',  ( 50.84997085138504502, 39.99999999999999289, -39.01959913716785167 ) ) ;
#35321 = CARTESIAN_POINT ( 'NONE',  ( -22.00000000000000000, 31.00000000000000355, 0.000000000000000000 ) ) ;
#35322 = VECTOR ( 'NONE', #40851, 1000.000000000000000 ) ;
#35323 = VERTEX_POINT ( 'NONE', #38268 ) ;
#35324 = CARTESIAN_POINT ( 'NONE',  ( 0.000000000000000000, -12.42760411676013987, -33.78690065568439138 ) ) ;
#35325 = CARTESIAN_POINT ( 'NONE',  ( 0.000000000000000000, -32.32520163883607722, 34.09746168776025854 ) ) ;
#35326 = ORIENTED_EDGE ( 'NONE', *, *, #36948, .T. ) ;
#35327 = VERTEX_POINT ( 'NONE', #8176 ) ;
#35328 = DIRECTION ( 'NONE',  ( -1.000000000000000000, -0.000000000000000000, -0.000000000000000000 ) ) ;
#35329 = ORIENTED_EDGE ( 'NONE', *, *, #30375, .T. ) ;
#35330 = CARTESIAN_POINT ( 'NONE',  ( 18.00000000000000355, 43.83938735307292944, -18.28286404005752175 ) ) ;
#35331 = DIRECTION ( 'NONE',  ( -1.000000000000000000, -0.000000000000000000, 0.000000000000000000 ) ) ;
#35332 = ADVANCED_FACE ( 'NONE', ( #41756 ), #7734, .T. ) ;
#35333 = CIRCLE ( 'NONE', #4688, 24.99999999999998934 ) ;
#35334 = PRODUCT_RELATED_PRODUCT_CATEGORY ( 'part', '', ( #26283 ) ) ;
#35335 = DIRECTION ( 'NONE',  ( 0.000000000000000000, 0.000000000000000000, 1.000000000000000000 ) ) ;
#35336 = CARTESIAN_POINT ( 'NONE',  ( 17.99999999999999645, 90.81729652456265001, -72.16798910853526650 ) ) ;
#35337 = VERTEX_POINT ( 'NONE', #11245 ) ;
#35338 = CIRCLE ( 'NONE', #16563, 19.19999999999999218 ) ;
#35339 = DIRECTION ( 'NONE',  ( 0.000000000000000000, 0.000000000000000000, 1.000000000000000000 ) ) ;
#35340 = CIRCLE ( 'NONE', #27012, 59.00000000000000000 ) ;
#35341 = EDGE_LOOP ( 'NONE', ( #16635, #2398, #2089, #39577 ) ) ;
#35343 = CARTESIAN_POINT ( 'NONE',  ( 17.99999999999999645, 16.77727049691110750, 27.19001440037552086 ) ) ;
#35342 = VECTOR ( 'NONE', #6876, 1000.000000000000000 ) ;
#35344 = ORIENTED_EDGE ( 'NONE', *, *, #37138, .F. ) ;
#35345 = CARTESIAN_POINT ( 'NONE',  ( 17.99999999999999645, -45.89132998247981732, -102.3829004574634496 ) ) ;
#35346 = AXIS2_PLACEMENT_3D ( 'NONE', #21095, #733, #14097 ) ;
#35347 = CARTESIAN_POINT ( 'NONE',  ( -132.0000507999999968, 0.000000000000000000, 0.000000000000000000 ) ) ;
#35348 = DIRECTION ( 'NONE',  ( 6.123233995736766036E-17, 1.000000000000000000, 0.000000000000000000 ) ) ;
#35349 = EDGE_CURVE ( 'NONE', #9926, #714, #10260, .T. ) ;
#35350 = CARTESIAN_POINT ( 'NONE',  ( -4.000000000000000000, -2.309401076758515803, -0.4999999999999995559 ) ) ;
#35351 = EDGE_CURVE ( 'NONE', #41306, #41672, #37413, .T. ) ;
#35352 = CARTESIAN_POINT ( 'NONE',  ( -24.21661388771557100, 31.00000000000000355, 41.94898165618241137 ) ) ;
#35353 = VERTEX_POINT ( 'NONE', #27836 ) ;
#35354 = CARTESIAN_POINT ( 'NONE',  ( 0.000000000000000000, 0.000000000000000000, 0.000000000000000000 ) ) ;
#35355 = AXIS2_PLACEMENT_3D ( 'NONE', #6845, #10343, #23681 ) ;
#35356 = ORIENTED_EDGE ( 'NONE', *, *, #686, .F. ) ;
#35357 = CARTESIAN_POINT ( 'NONE',  ( -30.90996028308246224, 40.00000000000000000, -53.51249422725337013 ) ) ;
#35358 = ADVANCED_FACE ( 'NONE', ( #15190 ), #21313, .F. ) ;
#35359 = DIRECTION ( 'NONE',  ( -1.000000000000000000, 0.000000000000000000, 0.000000000000000000 ) ) ;
#35360 = CARTESIAN_POINT ( 'NONE',  ( 17.99999999999999645, 23.85344185397197947, 113.5209818126991621 ) ) ;
#35361 = EDGE_CURVE ( 'NONE', #31070, #2459, #7519, .T. ) ;
#35362 = CIRCLE ( 'NONE', #1224, 13.59999999999999964 ) ;
#35363 = FACE_OUTER_BOUND ( 'NONE', #34200, .T. ) ;
#35364 = CYLINDRICAL_SURFACE ( 'NONE', #42649, 116.0000000000000000 ) ;
#35365 = VECTOR ( 'NONE', #32936, 1000.000000000000114 ) ;
#35366 = VECTOR ( 'NONE', #7189, 1000.000000000000000 ) ;
#35367 = VERTEX_POINT ( 'NONE', #20883 ) ;
#35368 = CARTESIAN_POINT ( 'NONE',  ( -35.29531037056285214, 40.00000000000000000, 17.40921588598563119 ) ) ;
#35369 = VERTEX_POINT ( 'NONE', #34788 ) ;
#35370 = CIRCLE ( 'NONE', #17292, 10.50000000000000178 ) ;
#35371 = DIRECTION ( 'NONE',  ( 0.000000000000000000, 0.9957341762950348008, -0.09226835946329869920 ) ) ;
#35372 = CARTESIAN_POINT ( 'NONE',  ( 4.000000000000000000, 0.000000000000000000, 0.000000000000000000 ) ) ;
#35373 = CIRCLE ( 'NONE', #31220, 31.49899999999999878 ) ;
#35374 = ORIENTED_EDGE ( 'NONE', *, *, #11897, .F. ) ;
#35375 = CIRCLE ( 'NONE', #6811, 20.00000000000001066 ) ;
#35376 = DIRECTION ( 'NONE',  ( 0.000000000000000000, 0.000000000000000000, -1.000000000000000000 ) ) ;
#35377 = VERTEX_POINT ( 'NONE', #4896 ) ;
#35378 = LINE ( 'NONE', #34948, #43081 ) ;
#35379 = ORIENTED_EDGE ( 'NONE', *, *, #35010, .T. ) ;
#35380 = ORIENTED_EDGE ( 'NONE', *, *, #4310, .F. ) ;
#35381 = DIRECTION ( 'NONE',  ( 0.000000000000000000, 0.5264321628773507289, 0.8502171357296173237 ) ) ;
#35382 = AXIS2_PLACEMENT_3D ( 'NONE', #4758, #22245, #14819 ) ;
#35383 = EDGE_CURVE ( 'NONE', #30536, #42073, #18258, .T. ) ;
#35384 = CARTESIAN_POINT ( 'NONE',  ( 86.90011881125596460, 31.00000000000000000, -5.573058087428397478 ) ) ;
#35385 = ORIENTED_EDGE ( 'NONE', *, *, #248, .F. ) ;
#35386 = DIRECTION ( 'NONE',  ( 0.000000000000000000, 0.000000000000000000, 1.000000000000000000 ) ) ;
#35387 = EDGE_CURVE ( 'NONE', #26141, #26339, #11686, .T. ) ;
#35388 = EDGE_CURVE ( 'NONE', #32556, #23084, #35362, .T. ) ;
#35389 = EDGE_CURVE ( 'NONE', #23944, #18098, #19401, .T. ) ;
#35390 = DIRECTION ( 'NONE',  ( 0.000000000000000000, 0.000000000000000000, 1.000000000000000000 ) ) ;
#35391 = ORIENTED_EDGE ( 'NONE', *, *, #19958, .T. ) ;
#35392 = CARTESIAN_POINT ( 'NONE',  ( -106.4195705685741871, -106.4195705685773135, 9.999999999999753086 ) ) ;
#35393 = DIRECTION ( 'NONE',  ( 1.000000000000000000, -1.058513553088275437E-16, 0.000000000000000000 ) ) ;
#35394 = CARTESIAN_POINT ( 'NONE',  ( -98.36195137680903144, 40.00000000000000711, 26.22212808230024805 ) ) ;
#35395 = AXIS2_PLACEMENT_3D ( 'NONE', #41044, #14250, #4618 ) ;
#35397 = CARTESIAN_POINT ( 'NONE',  ( 17.99999999999999645, 71.21168426767221149, -86.70160608319253015 ) ) ;
#35396 = DIRECTION ( 'NONE',  ( -0.000000000000000000, 0.000000000000000000, 1.000000000000000000 ) ) ;
#35398 = LINE ( 'NONE', #28459, #36654 ) ;
#35399 = DIRECTION ( 'NONE',  ( -1.000000000000000000, 0.000000000000000000, 0.000000000000000000 ) ) ;
#35400 = AXIS2_PLACEMENT_3D ( 'NONE', #21419, #34671, #4785 ) ;
#35401 = ORIENTED_EDGE ( 'NONE', *, *, #14157, .F. ) ;
#35402 = CARTESIAN_POINT ( 'NONE',  ( 0.000000000000000000, 0.000000000000000000, 0.000000000000000000 ) ) ;
#35403 = CIRCLE ( 'NONE', #13158, 51.99999999999999289 ) ;
#35404 = VERTEX_POINT ( 'NONE', #31958 ) ;
#35405 = LINE ( 'NONE', #37807, #10093 ) ;
#35406 = CARTESIAN_POINT ( 'NONE',  ( 6.381360069253262601, 31.00000000000000355, 97.39583333395333398 ) ) ;
#35407 = CARTESIAN_POINT ( 'NONE',  ( 0.000000000000000000, 32.00046193115198179, -34.40241257139653186 ) ) ;
#35409 = ORIENTED_EDGE ( 'NONE', *, *, #39011, .T. ) ;
#35408 = VECTOR ( 'NONE', #33167, 1000.000000000000000 ) ;
#35410 = CARTESIAN_POINT ( 'NONE',  ( 7.028922914820973311, 40.00000000000000000, 26.21578750688660264 ) ) ;
#35411 = CARTESIAN_POINT ( 'NONE',  ( 2.511863649308039736, 40.00000000000000000, 39.39933062585536305 ) ) ;
#35412 = ORIENTED_EDGE ( 'NONE', *, *, #24000, .F. ) ;
#35413 = EDGE_LOOP ( 'NONE', ( #32822, #1889, #721, #1730 ) ) ;
#35414 = CARTESIAN_POINT ( 'NONE',  ( 0.000000000000000000, 95.31344542257733110, 66.11616384574480776 ) ) ;
#35415 = LINE ( 'NONE', #29106, #13034 ) ;
#35416 = EDGE_CURVE ( 'NONE', #433, #19203, #42593, .T. ) ;
#35417 = CARTESIAN_POINT ( 'NONE',  ( -3.996523416598931009E-15, 2.658563593772952281E-14, 10.00000000000000178 ) ) ;
#35418 = CARTESIAN_POINT ( 'NONE',  ( 18.00000000000000355, 37.91532898920922889, 28.61088654061651937 ) ) ;
#35419 = CYLINDRICAL_SURFACE ( 'NONE', #31356, 116.0000000000000000 ) ;
#35420 = ORIENTED_EDGE ( 'NONE', *, *, #24061, .F. ) ;
#35421 = DIRECTION ( 'NONE',  ( 2.932542530036133930E-17, 1.000000000000000000, -5.216001792149171863E-18 ) ) ;
#35422 = ORIENTED_EDGE ( 'NONE', *, *, #30757, .T. ) ;
#35423 = DIRECTION ( 'NONE',  ( 0.000000000000000000, 1.000000000000000000, -1.060184893785364939E-15 ) ) ;
#35424 = DIRECTION ( 'NONE',  ( 0.000000000000000000, 0.000000000000000000, 1.000000000000000000 ) ) ;
#35425 = AXIS2_PLACEMENT_3D ( 'NONE', #3148, #1723, #16085 ) ;
#35426 = CIRCLE ( 'NONE', #22244, 59.00000000000000000 ) ;
#35427 = DIRECTION ( 'NONE',  ( 0.000000000000000000, 0.000000000000000000, 1.000000000000000000 ) ) ;
#35428 = DIRECTION ( 'NONE',  ( 0.000000000000000000, 0.000000000000000000, -1.000000000000000000 ) ) ;
#35429 = ORIENTED_EDGE ( 'NONE', *, *, #15000, .T. ) ;
#35430 = ORIENTED_EDGE ( 'NONE', *, *, #35792, .T. ) ;
#35431 = VECTOR ( 'NONE', #35622, 1000.000000000000000 ) ;
#35432 = DIRECTION ( 'NONE',  ( -1.000000000000000000, 0.000000000000000000, 0.000000000000000000 ) ) ;
#35433 = VERTEX_POINT ( 'NONE', #8815 ) ;
#35435 = ORIENTED_EDGE ( 'NONE', *, *, #35086, .T. ) ;
#35434 = DIRECTION ( 'NONE',  ( 0.000000000000000000, 1.000000000000000000, 0.000000000000000000 ) ) ;
#35436 = CARTESIAN_POINT ( 'NONE',  ( -50.71442127988192539, 31.00000000000000355, -13.67646662467867991 ) ) ;
#35437 = VERTEX_POINT ( 'NONE', #39311 ) ;
#35438 = CARTESIAN_POINT ( 'NONE',  ( 0.000000000000000000, -68.61497464550522807, -99.05794392877676557 ) ) ;
#35439 = EDGE_CURVE ( 'NONE', #36920, #4115, #31210, .T. ) ;
#35440 = EDGE_CURVE ( 'NONE', #23495, #15009, #32596, .T. ) ;
#35441 = FACE_OUTER_BOUND ( 'NONE', #5376, .T. ) ;
#35442 = EDGE_CURVE ( 'NONE', #28874, #13089, #26323, .T. ) ;
#35443 = VERTEX_POINT ( 'NONE', #15595 ) ;
#35444 = CARTESIAN_POINT ( 'NONE',  ( 77.09314031436157677, 39.99999999999999289, 5.156213784760051766 ) ) ;
#35446 = DIRECTION ( 'NONE',  ( 0.000000000000000000, 0.000000000000000000, 1.000000000000000000 ) ) ;
#35445 = CARTESIAN_POINT ( 'NONE',  ( 0.000000000000000000, 111.2721026680460596, 44.61974821237342326 ) ) ;
#35447 = DIRECTION ( 'NONE',  ( -3.996523416598930318E-16, 2.658563593772947863E-15, 1.000000000000000000 ) ) ;
#35448 = VERTEX_POINT ( 'NONE', #16237 ) ;
#35449 = FACE_OUTER_BOUND ( 'NONE', #3814, .T. ) ;
#35450 = ORIENTED_EDGE ( 'NONE', *, *, #33539, .F. ) ;
#35451 = DIRECTION ( 'NONE',  ( -1.000000000000000000, -0.000000000000000000, -0.000000000000000000 ) ) ;
#35452 = LINE ( 'NONE', #18495, #1101 ) ;
#35453 = ADVANCED_FACE ( 'NONE', ( #26049, #12744, #36057 ), #38908, .T. ) ;
#35454 = CARTESIAN_POINT ( 'NONE',  ( -70.10416666575086708, 31.00000000000000711, -4.581489278090966621 ) ) ;
#35455 = AXIS2_PLACEMENT_3D ( 'NONE', #33496, #4904, #18476 ) ;
#35457 = DIRECTION ( 'NONE',  ( -1.000000000000000000, -0.000000000000000000, -0.000000000000000000 ) ) ;
#35456 = DIRECTION ( 'NONE',  ( 1.000000000000000000, 0.000000000000000000, 0.000000000000000000 ) ) ;
#35458 = ORIENTED_EDGE ( 'NONE', *, *, #7549, .F. ) ;
#35459 = AXIS2_PLACEMENT_3D ( 'NONE', #8536, #25171, #35371 ) ;
#35460 = DIRECTION ( 'NONE',  ( 0.000000000000000000, 0.000000000000000000, 1.000000000000000000 ) ) ;
#35461 = VERTEX_POINT ( 'NONE', #12959 ) ;
#35462 = CARTESIAN_POINT ( 'NONE',  ( 0.000000000000000000, -98.69720329640912837, -60.94966826380012037 ) ) ;
#35463 = CARTESIAN_POINT ( 'NONE',  ( -91.96080130434573618, -35.35525454449571470, 14.45886780445633946 ) ) ;
#35464 = CARTESIAN_POINT ( 'NONE',  ( -91.90012763196533285, 31.00000000000000711, 5.898218105444796855 ) ) ;
#35465 = CARTESIAN_POINT ( 'NONE',  ( 72.29027477046881245, 39.99999999999999289, -63.25088587038124643 ) ) ;
#35466 = DIRECTION ( 'NONE',  ( 1.000000000000000000, 1.836909530733573776E-16, 0.000000000000000000 ) ) ;
#35467 = ORIENTED_EDGE ( 'NONE', *, *, #3043, .F. ) ;
#35468 = DIRECTION ( 'NONE',  ( 1.000000000000000000, 0.000000000000000000, 0.000000000000000000 ) ) ;
#35469 = ORIENTED_EDGE ( 'NONE', *, *, #6314, .T. ) ;
#35471 = EDGE_LOOP ( 'NONE', ( #30410, #29889, #643, #42227 ) ) ;
#35470 = DIRECTION ( 'NONE',  ( -1.000000000000000000, 0.000000000000000000, -0.000000000000000000 ) ) ;
#35472 = DIRECTION ( 'NONE',  ( 0.000000000000000000, 0.000000000000000000, -1.000000000000000000 ) ) ;
#35473 = ORIENTED_EDGE ( 'NONE', *, *, #36834, .F. ) ;
#35474 = DIRECTION ( 'NONE',  ( -1.000000000000000000, -0.000000000000000000, 0.000000000000000000 ) ) ;
#35475 = FACE_OUTER_BOUND ( 'NONE', #4241, .T. ) ;
#35476 = CARTESIAN_POINT ( 'NONE',  ( 4.999999999999997335, 5.204748896376250699E-16, -4.250000000000000000 ) ) ;
#35477 = ORIENTED_EDGE ( 'NONE', *, *, #17716, .F. ) ;
#35478 = CARTESIAN_POINT ( 'NONE',  ( 21.18498618631003083, 31.00000000000000355, 18.62224443192850387 ) ) ;
#35479 = CIRCLE ( 'NONE', #3417, 116.0000000000000000 ) ;
#35480 = CYLINDRICAL_SURFACE ( 'NONE', #41101, 116.0000000000000000 ) ;
#35481 = VECTOR ( 'NONE', #37620, 1000.000000000000000 ) ;
#35482 = EDGE_CURVE ( 'NONE', #1782, #40246, #39113, .T. ) ;
#35483 = AXIS2_PLACEMENT_3D ( 'NONE', #42107, #12266, #25593 ) ;
#35485 = ORIENTED_EDGE ( 'NONE', *, *, #35589, .F. ) ;
#35484 = CARTESIAN_POINT ( 'NONE',  ( 9.000000000000001776, 31.08872492060014636, -41.68322423723067516 ) ) ;
#35486 = ORIENTED_EDGE ( 'NONE', *, *, #982, .F. ) ;
#35487 = DIRECTION ( 'NONE',  ( -1.000000000000000000, -0.000000000000000000, -0.000000000000000000 ) ) ;
#35488 = CARTESIAN_POINT ( 'NONE',  ( -15.99999999999997691, 17.11489954122026447, 4.500000000000005329 ) ) ;
#35489 = CARTESIAN_POINT ( 'NONE',  ( 20.11321884379431779, 40.00000000000000000, -40.61652209560084259 ) ) ;
#35490 = DIRECTION ( 'NONE',  ( -1.000000000000000000, 0.000000000000000000, 0.000000000000000000 ) ) ;
#35491 = ADVANCED_FACE ( 'NONE', ( #19522 ), #32582, .F. ) ;
#35492 = FACE_OUTER_BOUND ( 'NONE', #31859, .T. ) ;
#35493 = CARTESIAN_POINT ( 'NONE',  ( 17.99999999999999645, -31.94619804602753277, -16.59639811537389775 ) ) ;
#35494 = ORIENTED_EDGE ( 'NONE', *, *, #24456, .T. ) ;
#35495 = LINE ( 'NONE', #9744, #2805 ) ;
#35496 = EDGE_CURVE ( 'NONE', #13162, #30365, #6112, .T. ) ;
#35497 = ORIENTED_EDGE ( 'NONE', *, *, #33156, .T. ) ;
#35498 = DIRECTION ( 'NONE',  ( 0.000000000000000000, 0.000000000000000000, -1.000000000000000000 ) ) ;
#35499 = DIRECTION ( 'NONE',  ( -1.000000000000000000, -0.000000000000000000, -0.000000000000000000 ) ) ;
#35500 = ADVANCED_FACE ( 'NONE', ( #32790 ), #2871, .T. ) ;
#35501 = CARTESIAN_POINT ( 'NONE',  ( 32.11716166826300167, 31.00000000000000355, 15.82712457579038912 ) ) ;
#35502 = ORIENTED_EDGE ( 'NONE', *, *, #18565, .F. ) ;
#35503 = CARTESIAN_POINT ( 'NONE',  ( 1.567478505476134606E-15, 4.618802153517012066, -3.433295621305382905 ) ) ;
#35504 = ORIENTED_EDGE ( 'NONE', *, *, #13697, .F. ) ;
#35505 = CONTEXT_DEPENDENT_SHAPE_REPRESENTATION ( #4742, #12075 ) ;
#35506 = DIRECTION ( 'NONE',  ( 1.000000000000000000, -0.000000000000000000, -0.000000000000000000 ) ) ;
#35507 = CARTESIAN_POINT ( 'NONE',  ( 84.89583333414414312, 31.00000000000000000, -5.563236982362012029 ) ) ;
#35508 = CIRCLE ( 'NONE', #16740, 59.00000000000000000 ) ;
#35509 = CIRCLE ( 'NONE', #1377, 120.5010000000000474 ) ;
#35510 = AXIS2_PLACEMENT_3D ( 'NONE', #15354, #2624, #12066 ) ;
#35511 = CARTESIAN_POINT ( 'NONE',  ( 17.99999999999999645, -100.8494052988175298, 65.95368414178875582 ) ) ;
#35512 = ORIENTED_EDGE ( 'NONE', *, *, #12137, .T. ) ;
#35513 = CARTESIAN_POINT ( 'NONE',  ( -45.80426865612386678, 31.00000000000000355, -26.55377233851146812 ) ) ;
#35514 = CYLINDRICAL_SURFACE ( 'NONE', #2930, 47.49900000000000233 ) ;
#35515 = ORIENTED_EDGE ( 'NONE', *, *, #35439, .T. ) ;
#35516 = EDGE_CURVE ( 'NONE', #8087, #38742, #18017, .T. ) ;
#35517 = CARTESIAN_POINT ( 'NONE',  ( -19.85879968743109458, -2.055254544495720648, 67.01652747270929922 ) ) ;
#35518 = LINE ( 'NONE', #25320, #41692 ) ;
#35519 = DIRECTION ( 'NONE',  ( 0.000000000000000000, 0.000000000000000000, -1.000000000000000000 ) ) ;
#35521 = VERTEX_POINT ( 'NONE', #18699 ) ;
#35520 = DIRECTION ( 'NONE',  ( 0.000000000000000000, -2.487417051993862264E-14, -1.000000000000000000 ) ) ;
#35522 = DIRECTION ( 'NONE',  ( 0.000000000000000000, 0.000000000000000000, 1.000000000000000000 ) ) ;
#35523 = FACE_OUTER_BOUND ( 'NONE', #26747, .T. ) ;
#35524 = ORIENTED_EDGE ( 'NONE', *, *, #21536, .T. ) ;
#35525 = CARTESIAN_POINT ( 'NONE',  ( 64.36038921521112854, 39.99999999999999289, -37.17434371002195803 ) ) ;
#35526 = DIRECTION ( 'NONE',  ( -0.000000000000000000, -0.000000000000000000, -1.000000000000000000 ) ) ;
#35527 = ORIENTED_EDGE ( 'NONE', *, *, #8443, .F. ) ;
#35528 = CARTESIAN_POINT ( 'NONE',  ( -80.96080130434580724, -40.05525454449572464, 14.45886780445738395 ) ) ;
#35529 = ORIENTED_EDGE ( 'NONE', *, *, #7899, .F. ) ;
#35530 = EDGE_CURVE ( 'NONE', #28999, #20186, #38688, .T. ) ;
#35531 = ORIENTED_EDGE ( 'NONE', *, *, #3451, .F. ) ;
#35532 = DIRECTION ( 'NONE',  ( 0.000000000000000000, 0.000000000000000000, 1.000000000000000000 ) ) ;
#35534 = ORIENTED_EDGE ( 'NONE', *, *, #13364, .F. ) ;
#35533 = AXIS2_PLACEMENT_3D ( 'NONE', #10079, #39532, #12952 ) ;
#35535 = DIRECTION ( 'NONE',  ( 1.000000000000000000, 0.000000000000000000, 0.000000000000000000 ) ) ;
#35536 = AXIS2_PLACEMENT_3D ( 'NONE', #9248, #23030, #42605 ) ;
#35537 = CYLINDRICAL_SURFACE ( 'NONE', #39470, 31.49899999999999878 ) ;
#35538 = VECTOR ( 'NONE', #34908, 1000.000000000000000 ) ;
#35539 = CARTESIAN_POINT ( 'NONE',  ( 0.000000000000000000, 17.08890430202750110, 43.76671000081951490 ) ) ;
#35540 = VECTOR ( 'NONE', #16843, 1000.000000000000000 ) ;
#35541 = CARTESIAN_POINT ( 'NONE',  ( -6.896599878636567205, -12.98179148322719101, 0.000000000000000000 ) ) ;
#35542 = VERTEX_POINT ( 'NONE', #42163 ) ;
#35543 = CARTESIAN_POINT ( 'NONE',  ( -1.420922472151883646E-13, 9.833206111663764869E-13, 369.6955262170047831 ) ) ;
#35544 = UNCERTAINTY_MEASURE_WITH_UNIT (LENGTH_MEASURE( 1.000000000000000082E-05 ), #36447, 'distance_accuracy_value', 'NONE');
#35545 = EDGE_CURVE ( 'NONE', #4843, #41828, #40233, .T. ) ;
#35546 = ORIENTED_EDGE ( 'NONE', *, *, #17212, .F. ) ;
#35547 = CARTESIAN_POINT ( 'NONE',  ( -100.6569797752917879, -12.05525454449572109, -8.979913733870429127 ) ) ;
#35548 = ORIENTED_EDGE ( 'NONE', *, *, #13697, .T. ) ;
#35549 = CYLINDRICAL_SURFACE ( 'NONE', #11371, 2.649999999999993694 ) ;
#35550 = FACE_OUTER_BOUND ( 'NONE', #41217, .T. ) ;
#35551 = CARTESIAN_POINT ( 'NONE',  ( 0.000000000000000000, 110.8621702203453339, -34.14058016547420493 ) ) ;
#35552 = CARTESIAN_POINT ( 'NONE',  ( 50.84997085137049311, 31.00000000000000000, -39.01959913718239648 ) ) ;
#35553 = ORIENTED_EDGE ( 'NONE', *, *, #758, .T. ) ;
#35554 = DIRECTION ( 'NONE',  ( 0.000000000000000000, 0.7865515558026436871, -0.6175246149461904865 ) ) ;
#35555 = CIRCLE ( 'NONE', #32755, 58.99999999999999289 ) ;
#35556 = EDGE_LOOP ( 'NONE', ( #19908, #22726 ) ) ;
#35557 = CARTESIAN_POINT ( 'NONE',  ( -3.763366191185464782, 40.00000000000000000, 57.60416666550938203 ) ) ;
#35558 = AXIS2_PLACEMENT_3D ( 'NONE', #39397, #9539, #22891 ) ;
#35560 = EDGE_CURVE ( 'NONE', #32031, #32639, #7487, .T. ) ;
#35559 = AXIS2_PLACEMENT_3D ( 'NONE', #22013, #14810, #18320 ) ;
#35561 = AXIS2_PLACEMENT_3D ( 'NONE', #35895, #4243, #26750 ) ;
#35562 = CARTESIAN_POINT ( 'NONE',  ( 0.000000000000000000, 0.000000000000000000, 0.000000000000000000 ) ) ;
#35563 = DIRECTION ( 'NONE',  ( 0.000000000000000000, 0.000000000000000000, 1.000000000000000000 ) ) ;
#35565 = EDGE_CURVE ( 'NONE', #38794, #14329, #32158, .T. ) ;
#35564 = AXIS2_PLACEMENT_3D ( 'NONE', #15035, #42027, #2526 ) ;
#35566 = AXIS2_PLACEMENT_3D ( 'NONE', #42057, #19424, #25950 ) ;
#35567 = CARTESIAN_POINT ( 'NONE',  ( 0.000000000000000000, -10.40101730206288622, -120.0512800434972149 ) ) ;
#35568 = FACE_OUTER_BOUND ( 'NONE', #9859, .T. ) ;
#35569 = ORIENTED_EDGE ( 'NONE', *, *, #25464, .T. ) ;
#35570 = CARTESIAN_POINT ( 'NONE',  ( -42.66459923921424036, 40.00000000000000000, 24.64557685607233140 ) ) ;
#35571 = EDGE_LOOP ( 'NONE', ( #16940, #38645 ) ) ;
#35572 = CARTESIAN_POINT ( 'NONE',  ( 17.99999999999999645, 0.000000000000000000, 0.000000000000000000 ) ) ;
#35573 = DIRECTION ( 'NONE',  ( -1.847415842360817484E-16, 1.000000000000000000, 0.000000000000000000 ) ) ;
#35574 = ORIENTED_EDGE ( 'NONE', *, *, #22902, .F. ) ;
#35575 = DIRECTION ( 'NONE',  ( -1.000000000000000000, -0.000000000000000000, 0.000000000000000000 ) ) ;
#35576 = ORIENTED_EDGE ( 'NONE', *, *, #7549, .T. ) ;
#35577 = DIRECTION ( 'NONE',  ( 3.009274222672345096E-17, 1.000000000000000000, -2.455023325076454960E-18 ) ) ;
#35578 = ORIENTED_EDGE ( 'NONE', *, *, #24098, .T. ) ;
#35579 = EDGE_CURVE ( 'NONE', #16529, #2667, #16687, .T. ) ;
#35580 = EDGE_LOOP ( 'NONE', ( #38483, #19871 ) ) ;
#35581 = LINE ( 'NONE', #2827, #26495 ) ;
#35582 = CARTESIAN_POINT ( 'NONE',  ( -26.95034633362163845, 31.00000000000000355, -79.72278128421110921 ) ) ;
#35583 = ORIENTED_EDGE ( 'NONE', *, *, #41343, .F. ) ;
#35584 = CARTESIAN_POINT ( 'NONE',  ( -4.000000000000000000, -1.680117682357936904, -3.316611593218794951 ) ) ;
#35585 = CIRCLE ( 'NONE', #6348, 120.5010000000000190 ) ;
#35586 = CARTESIAN_POINT ( 'NONE',  ( 18.00000000000000355, -46.19362259308827845, -8.585149169758995669 ) ) ;
#35587 = ORIENTED_EDGE ( 'NONE', *, *, #12557, .F. ) ;
#35588 = DIRECTION ( 'NONE',  ( 1.000000000000000000, 0.000000000000000000, -6.546126324440850663E-16 ) ) ;
#35589 = EDGE_CURVE ( 'NONE', #27630, #12333, #13814, .T. ) ;
#35590 = CARTESIAN_POINT ( 'NONE',  ( 17.99999999999999645, 0.000000000000000000, 0.000000000000000000 ) ) ;
#35591 = AXIS2_PLACEMENT_3D ( 'NONE', #4246, #40021, #10595 ) ;
#35592 = CYLINDRICAL_SURFACE ( 'NONE', #42212, 13.60000000000000142 ) ;
#35593 = EDGE_CURVE ( 'NONE', #39812, #36216, #8220, .T. ) ;
#35595 = DIRECTION ( 'NONE',  ( 0.000000000000000000, 0.000000000000000000, 1.000000000000000000 ) ) ;
#35594 = PLANE ( 'NONE',  #6393 ) ;
#35596 = AXIS2_PLACEMENT_3D ( 'NONE', #6654, #3782, #80 ) ;
#35597 = CARTESIAN_POINT ( 'NONE',  ( -19.76500330823589735, 31.00000000000000355, -5.286999072153966139 ) ) ;
#35598 = ADVANCED_FACE ( 'NONE', ( #30396 ), #6821, .F. ) ;
#35599 = CARTESIAN_POINT ( 'NONE',  ( 0.000000000000000000, 71.21168426767107462, 86.70160608319346807 ) ) ;
#35600 = ORIENTED_EDGE ( 'NONE', *, *, #27930, .T. ) ;
#35601 = AXIS2_PLACEMENT_3D ( 'NONE', #30534, #13315, #13956 ) ;
#35602 = ORIENTED_EDGE ( 'NONE', *, *, #29228, .T. ) ;
#35603 = CYLINDRICAL_SURFACE ( 'NONE', #20604, 2.649999999999957723 ) ;
#35604 = CARTESIAN_POINT ( 'NONE',  ( 18.00000000000000355, -38.92705108641711576, -27.21837053747839263 ) ) ;
#35605 = ORIENTED_EDGE ( 'NONE', *, *, #22730, .F. ) ;
#35606 = CARTESIAN_POINT ( 'NONE',  ( 23.79574588541966662, 40.00000000000000000, -6.380716493563439506 ) ) ;
#35607 = CARTESIAN_POINT ( 'NONE',  ( -8.786317949316114095, 40.00000000000000000, -33.00646673686679833 ) ) ;
#35608 = VECTOR ( 'NONE', #29691, 1000.000000000000000 ) ;
#35609 = ORIENTED_EDGE ( 'NONE', *, *, #37600, .T. ) ;
#35610 = EDGE_CURVE ( 'NONE', #27138, #37158, #11003, .T. ) ;
#35611 = EDGE_LOOP ( 'NONE', ( #35152, #29342, #33667, #14328 ) ) ;
#35612 =( NAMED_UNIT ( * ) PLANE_ANGLE_UNIT ( ) SI_UNIT ( $, .RADIAN. ) );
#35613 = DIRECTION ( 'NONE',  ( -1.000000000000000000, -0.000000000000000000, -0.000000000000000000 ) ) ;
#35614 = EDGE_CURVE ( 'NONE', #32794, #28703, #40924, .T. ) ;
#35615 = EDGE_CURVE ( 'NONE', #6740, #32276, #24991, .T. ) ;
#35616 = EDGE_CURVE ( 'NONE', #20160, #38193, #17320, .T. ) ;
#35617 = DIRECTION ( 'NONE',  ( -1.000000000000000000, 0.000000000000000000, 0.000000000000000000 ) ) ;
#35618 = CARTESIAN_POINT ( 'NONE',  ( 0.000000000000000000, 0.000000000000000000, 0.000000000000000000 ) ) ;
#35619 = ORIENTED_EDGE ( 'NONE', *, *, #3974, .F. ) ;
#35620 = CARTESIAN_POINT ( 'NONE',  ( 5.657435538624008755E-15, 4.615443851143735910E-16, 367.6955262170047263 ) ) ;
#35621 = ORIENTED_EDGE ( 'NONE', *, *, #12156, .T. ) ;
#35622 = DIRECTION ( 'NONE',  ( -1.000000000000000000, 0.000000000000000000, 0.000000000000000000 ) ) ;
#35623 = AXIS2_PLACEMENT_3D ( 'NONE', #32326, #25611, #29496 ) ;
#35624 = DIRECTION ( 'NONE',  ( -1.000000000000000000, -0.000000000000000000, -0.000000000000000000 ) ) ;
#35625 = APPLICATION_CONTEXT ( 'automotive_design' ) ;
#35626 = AXIS2_PLACEMENT_3D ( 'NONE', #10274, #26650, #37685 ) ;
#35627 = DIRECTION ( 'NONE',  ( -1.000000000000000000, 0.000000000000000000, 0.000000000000000000 ) ) ;
#35628 = VECTOR ( 'NONE', #8180, 1000.000000000000000 ) ;
#35629 = CARTESIAN_POINT ( 'NONE',  ( 18.00000000000000355, -11.46872990052412788, 45.56340405422441364 ) ) ;
#35630 = VERTEX_POINT ( 'NONE', #6592 ) ;
#35631 = CARTESIAN_POINT ( 'NONE',  ( 29.96647033545507455, 40.00000000000000000, -88.27250603610892199 ) ) ;
#35632 = EDGE_LOOP ( 'NONE', ( #32340, #29267, #24323, #33123 ) ) ;
#35633 = CARTESIAN_POINT ( 'NONE',  ( 17.99999999999999645, -16.86122981692037825, 27.13802899033285954 ) ) ;
#35634 = VERTEX_POINT ( 'NONE', #36918 ) ;
#35636 = ORIENTED_EDGE ( 'NONE', *, *, #5551, .F. ) ;
#35635 = FACE_OUTER_BOUND ( 'NONE', #20826, .T. ) ;
#35637 = CARTESIAN_POINT ( 'NONE',  ( -3.331996295684063192, 31.00000000000000355, 49.59602437330212865 ) ) ;
#35638 = ORIENTED_EDGE ( 'NONE', *, *, #4379, .F. ) ;
#35639 = FACE_OUTER_BOUND ( 'NONE', #30162, .T. ) ;
#35640 = DIRECTION ( 'NONE',  ( 1.000000000000000000, 0.000000000000000000, 0.000000000000000000 ) ) ;
#35641 = PRODUCT ( 'BR-544', 'BR-544', '', ( #39776 ) ) ;
#35642 = ADVANCED_FACE ( 'NONE', ( #20178 ), #13834, .F. ) ;
#35643 = VERTEX_POINT ( 'NONE', #33437 ) ;
#35644 = CARTESIAN_POINT ( 'NONE',  ( -36.82253293460209420, 40.00000000000000000, -63.98115709648401150 ) ) ;
#35646 = CARTESIAN_POINT ( 'NONE',  ( 0.000000000000000000, 0.000000000000000000, 0.000000000000000000 ) ) ;
#35645 = DIRECTION ( 'NONE',  ( -1.000000000000000000, 0.000000000000000000, -0.000000000000000000 ) ) ;
#35647 = DIRECTION ( 'NONE',  ( 1.000000000000000000, -0.000000000000000000, -0.000000000000000000 ) ) ;
#35648 = EDGE_LOOP ( 'NONE', ( #2484, #29444, #39313, #24845, #4226 ) ) ;
#35649 = DIRECTION ( 'NONE',  ( -1.000000000000000000, -0.000000000000000000, 0.000000000000000000 ) ) ;
#35650 = VERTEX_POINT ( 'NONE', #10318 ) ;
#35651 = AXIS2_PLACEMENT_3D ( 'NONE', #7433, #33830, #27095 ) ;
#35652 = CARTESIAN_POINT ( 'NONE',  ( 0.000000000000000000, 107.2885202478273783, -54.86040852957203384 ) ) ;
#35653 = CARTESIAN_POINT ( 'NONE',  ( 9.000000000000001776, 115.5737863835463628, -9.934782381632540904 ) ) ;
#35654 = AXIS2_PLACEMENT_3D ( 'NONE', #30469, #14114, #20243 ) ;
#35655 = CARTESIAN_POINT ( 'NONE',  ( -35.92146702467432817, 31.00000000000000355, -62.19081021767443218 ) ) ;
#35657 = DIRECTION ( 'NONE',  ( 0.000000000000000000, 0.000000000000000000, -1.000000000000000000 ) ) ;
#35656 = CARTESIAN_POINT ( 'NONE',  ( 17.99999999999999645, 62.45178862086215332, 93.20969140437529177 ) ) ;
#35658 = ORIENTED_EDGE ( 'NONE', *, *, #4541, .T. ) ;
#35659 = AXIS2_PLACEMENT_3D ( 'NONE', #34247, #34039, #20777 ) ;
#35660 = CYLINDRICAL_SURFACE ( 'NONE', #33097, 116.0000000000000000 ) ;
#35661 = AXIS2_PLACEMENT_3D ( 'NONE', #31283, #21507, #21918 ) ;
#35662 = ORIENTED_EDGE ( 'NONE', *, *, #27769, .T. ) ;
#35663 = DIRECTION ( 'NONE',  ( -1.000000000000000000, 0.000000000000000000, -0.000000000000000000 ) ) ;
#35664 = DIRECTION ( 'NONE',  ( 0.000000000000000000, 0.000000000000000000, 1.000000000000000000 ) ) ;
#35665 = EDGE_CURVE ( 'NONE', #12333, #12218, #22896, .T. ) ;
#35666 = CARTESIAN_POINT ( 'NONE',  ( -73.90312034494817794, 31.00000000000000711, -56.84521418461152109 ) ) ;
#35667 = CARTESIAN_POINT ( 'NONE',  ( -89.42636861580037078, 40.00000000000000711, -24.07434901465519417 ) ) ;
#35668 = EDGE_CURVE ( 'NONE', #25672, #14569, #22183, .T. ) ;
#35669 = EDGE_CURVE ( 'NONE', #40129, #13510, #3979, .T. ) ;
#35670 = LINE ( 'NONE', #9277, #18452 ) ;
#35671 = EDGE_CURVE ( 'NONE', #13710, #9297, #4720, .T. ) ;
#35672 = ORIENTED_EDGE ( 'NONE', *, *, #38570, .T. ) ;
#35673 = CARTESIAN_POINT ( 'NONE',  ( 0.000000000000000000, 73.51007459736548810, -89.73443560133290475 ) ) ;
#35674 = ORIENTED_EDGE ( 'NONE', *, *, #3883, .T. ) ;
#35675 = DIRECTION ( 'NONE',  ( 0.000000000000000000, -3.528251137579946599E-15, -1.000000000000000000 ) ) ;
#35677 = ORIENTED_EDGE ( 'NONE', *, *, #35883, .T. ) ;
#35676 = PLANE ( 'NONE',  #5349 ) ;
#35678 = EDGE_CURVE ( 'NONE', #38810, #15150, #16898, .T. ) ;
#35679 = DIRECTION ( 'NONE',  ( -1.000000000000000000, 0.000000000000000000, 0.000000000000000000 ) ) ;
#35680 = ORIENTED_EDGE ( 'NONE', *, *, #16440, .T. ) ;
#35681 = FACE_BOUND ( 'NONE', #27931, .T. ) ;
#35682 = LINE ( 'NONE', #5595, #4775 ) ;
#35683 = CYLINDRICAL_SURFACE ( 'NONE', #25748, 20.00000000000000355 ) ;
#35684 = EDGE_LOOP ( 'NONE', ( #20490, #11808, #15368, #21184 ) ) ;
#35685 = CARTESIAN_POINT ( 'NONE',  ( 26.89767027507546615, 31.00000000000000355, -1.736414864505229527 ) ) ;
#35686 = CARTESIAN_POINT ( 'NONE',  ( 12.49999999999995204, -1.368091241319530598E-13, -45.00000000000000000 ) ) ;
#35688 = ORIENTED_EDGE ( 'NONE', *, *, #6991, .T. ) ;
#35687 = CARTESIAN_POINT ( 'NONE',  ( -126.0000000000000284, 4.615443851143735910E-16, -20.00000000000001776 ) ) ;
#35689 = ORIENTED_EDGE ( 'NONE', *, *, #24444, .F. ) ;
#35690 = DIRECTION ( 'NONE',  ( 1.000000000000000000, 0.000000000000000000, 0.000000000000000000 ) ) ;
#35691 = DIRECTION ( 'NONE',  ( -1.000000000000000000, 0.000000000000000000, 0.000000000000000000 ) ) ;
#35692 = CARTESIAN_POINT ( 'NONE',  ( 11.72132095739929625, 40.00000000000000000, -43.45763713125776917 ) ) ;
#35693 = DIRECTION ( 'NONE',  ( 1.000000000000000000, 0.000000000000000000, 0.000000000000000000 ) ) ;
#35694 = LINE ( 'NONE', #32659, #20796 ) ;
#35695 = CARTESIAN_POINT ( 'NONE',  ( 8.919999999999996376, 0.000000000000000000, 0.000000000000000000 ) ) ;
#35696 = EDGE_LOOP ( 'NONE', ( #35319, #23242, #16903, #3349 ) ) ;
#35697 = EDGE_CURVE ( 'NONE', #12125, #1957, #43004, .T. ) ;
#35698 = CARTESIAN_POINT ( 'NONE',  ( 17.99999999999999645, 0.000000000000000000, 0.000000000000000000 ) ) ;
#35699 = ORIENTED_EDGE ( 'NONE', *, *, #18565, .T. ) ;
#35700 = CARTESIAN_POINT ( 'NONE',  ( -10.00000000000000000, 0.000000000000000000, 0.000000000000000000 ) ) ;
#35701 = LINE ( 'NONE', #15477, #12230 ) ;
#35702 = CARTESIAN_POINT ( 'NONE',  ( -31.00354902519490352, 31.00000000000000355, -27.18544651223506392 ) ) ;
#35703 = EDGE_LOOP ( 'NONE', ( #6340, #3227, #12027, #6603 ) ) ;
#35704 = ORIENTED_EDGE ( 'NONE', *, *, #31112, .T. ) ;
#35705 = DIRECTION ( 'NONE',  ( -1.000000000000000000, 0.000000000000000000, 0.000000000000000000 ) ) ;
#35706 = CARTESIAN_POINT ( 'NONE',  ( -58.57471716409879292, 31.00000000000000711, 66.78942258476980953 ) ) ;
#35707 = CARTESIAN_POINT ( 'NONE',  ( 0.000000000000000000, -74.56001736500559218, -88.86396238369110279 ) ) ;
#35708 = ORIENTED_EDGE ( 'NONE', *, *, #30577, .T. ) ;
#35709 = CARTESIAN_POINT ( 'NONE',  ( -60.39136959358631174, 31.00000000000000711, -16.27924862579292054 ) ) ;
#35710 = VECTOR ( 'NONE', #19795, 1000.000000000000000 ) ;
#35711 = CARTESIAN_POINT ( 'NONE',  ( 66.90003082753170816, 39.99999999999999289, -4.275635516647131595 ) ) ;
#35712 = EDGE_CURVE ( 'NONE', #21873, #13037, #10296, .T. ) ;
#35713 = CARTESIAN_POINT ( 'NONE',  ( 0.000000000000000000, -18.42432724429453827, -30.92804820216021611 ) ) ;
#35714 = ADVANCED_FACE ( 'NONE', ( #7027 ), #20382, .T. ) ;
#35715 = ORIENTED_EDGE ( 'NONE', *, *, #8211, .T. ) ;
#35716 = AXIS2_PLACEMENT_3D ( 'NONE', #32283, #2367, #39674 ) ;
#35717 = SURFACE_SIDE_STYLE ('',( #42485 ) ) ;
#35718 = DIRECTION ( 'NONE',  ( -1.000000000000000000, 0.000000000000000000, 0.000000000000000000 ) ) ;
#35719 = CARTESIAN_POINT ( 'NONE',  ( 17.99999999999999645, -84.77518783075143460, 73.49448960231327987 ) ) ;
#35721 = VERTEX_POINT ( 'NONE', #13183 ) ;
#35720 = CARTESIAN_POINT ( 'NONE',  ( 17.99999999999999645, 41.33768078145642022, -104.3046912715537076 ) ) ;
#35722 = LINE ( 'NONE', #26155, #39275 ) ;
#35723 = CARTESIAN_POINT ( 'NONE',  ( 9.000000000000000000, 34.78944633786291973, -9.257128253673258200 ) ) ;
#35724 = EDGE_CURVE ( 'NONE', #23495, #12305, #26476, .T. ) ;
#35725 = ORIENTED_EDGE ( 'NONE', *, *, #24466, .F. ) ;
#35726 = CARTESIAN_POINT ( 'NONE',  ( 68.07048008643859305, 39.99999999999999289, 33.55317283102968418 ) ) ;
#35727 = FACE_OUTER_BOUND ( 'NONE', #2203, .T. ) ;
#35728 = ORIENTED_EDGE ( 'NONE', *, *, #22643, .F. ) ;
#35729 = EDGE_CURVE ( 'NONE', #17094, #11164, #38218, .T. ) ;
#35730 = DIRECTION ( 'NONE',  ( 1.000000000000000000, -1.373900992973641868E-15, -4.017254365419995317E-16 ) ) ;
#35731 = ORIENTED_EDGE ( 'NONE', *, *, #17099, .T. ) ;
#35732 = AXIS2_PLACEMENT_3D ( 'NONE', #21124, #11489, #5133 ) ;
#35733 = ORIENTED_EDGE ( 'NONE', *, *, #27111, .T. ) ;
#35734 = DIRECTION ( 'NONE',  ( -1.000000000000000000, -0.000000000000000000, 0.000000000000000000 ) ) ;
#35735 = ORIENTED_EDGE ( 'NONE', *, *, #12460, .T. ) ;
#35736 = LINE ( 'NONE', #19438, #32099 ) ;
#35737 = CARTESIAN_POINT ( 'NONE',  ( -6.896599878636567205, -12.98179148322719101, -1.199999999999999956 ) ) ;
#35738 = CARTESIAN_POINT ( 'NONE',  ( 17.99999999999999645, 5.822172717930716779, -31.41458249383134671 ) ) ;
#35739 = DIRECTION ( 'NONE',  ( -1.000000000000000000, -0.000000000000000000, 0.000000000000000000 ) ) ;
#35740 = ORIENTED_EDGE ( 'NONE', *, *, #21375, .T. ) ;
#35741 = DIRECTION ( 'NONE',  ( 1.000000000000000000, 0.000000000000000000, 0.000000000000000000 ) ) ;
#35742 = ORIENTED_EDGE ( 'NONE', *, *, #26869, .F. ) ;
#35743 = AXIS2_PLACEMENT_3D ( 'NONE', #11118, #24446, #7819 ) ;
#35744 = DIRECTION ( 'NONE',  ( 1.000000000000000000, 0.000000000000000000, 0.000000000000000000 ) ) ;
#35745 = ORIENTED_EDGE ( 'NONE', *, *, #6305, .F. ) ;
#35746 = FACE_OUTER_BOUND ( 'NONE', #21489, .T. ) ;
#35747 = DIRECTION ( 'NONE',  ( 0.000000000000000000, 0.000000000000000000, 1.000000000000000000 ) ) ;
#35748 = DIRECTION ( 'NONE',  ( 0.000000000000000000, -9.408669700213189617E-16, -1.000000000000000000 ) ) ;
#35749 = CARTESIAN_POINT ( 'NONE',  ( -8.160545988181935328, 31.00000000000000355, -61.88879904071598048 ) ) ;
#35750 = CARTESIAN_POINT ( 'NONE',  ( 17.99999999999999645, -18.25486108452643208, 25.66996392254267079 ) ) ;
#35751 = CIRCLE ( 'NONE', #3697, 120.5010000000000190 ) ;
#35752 = ORIENTED_EDGE ( 'NONE', *, *, #15189, .F. ) ;
#35753 = CARTESIAN_POINT ( 'NONE',  ( 5.076274692534474831, 31.00000000000000355, 39.04542013319161953 ) ) ;
#35754 = AXIS2_PLACEMENT_3D ( 'NONE', #22405, #19128, #32183 ) ;
#35755 = ADVANCED_FACE ( 'NONE', ( #14909 ), #24084, .F. ) ;
#35756 = CARTESIAN_POINT ( 'NONE',  ( -41.80404827410195168, 40.00000000000000000, 54.50178954758867889 ) ) ;
#35757 = EDGE_CURVE ( 'NONE', #3682, #39427, #42354, .T. ) ;
#35758 = CIRCLE ( 'NONE', #40620, 116.0000000000000000 ) ;
#35759 = DIRECTION ( 'NONE',  ( 0.000000000000000000, 0.000000000000000000, 1.000000000000000000 ) ) ;
#35760 = FACE_OUTER_BOUND ( 'NONE', #11312, .T. ) ;
#35761 = CARTESIAN_POINT ( 'NONE',  ( 17.99999999999999645, 46.12538073176347808, 111.3235835452212825 ) ) ;
#35762 = CYLINDRICAL_SURFACE ( 'NONE', #11914, 2.100000000000000089 ) ;
#35763 = ADVANCED_FACE ( 'NONE', ( #31262 ), #34737, .F. ) ;
#35764 = ORIENTED_EDGE ( 'NONE', *, *, #29198, .T. ) ;
#35765 = CARTESIAN_POINT ( 'NONE',  ( 15.14372185054182651, 40.00000000000000000, 44.57714859939663654 ) ) ;
#35766 = DIRECTION ( 'NONE',  ( 0.000000000000000000, -0.8747630845319560589, -0.4845508703326597000 ) ) ;
#35767 = TOROIDAL_SURFACE ( 'NONE', #37189, 15.08402000000000065, 0.08401999999999888724 ) ;
#35768 = DIRECTION ( 'NONE',  ( 3.996523416598930318E-16, -2.658563593772947863E-15, -1.000000000000000000 ) ) ;
#35769 = EDGE_LOOP ( 'NONE', ( #37574, #30924, #40670, #35071 ) ) ;
#35770 = EDGE_CURVE ( 'NONE', #26433, #27839, #9639, .T. ) ;
#35771 = DIRECTION ( 'NONE',  ( 0.000000000000000000, 0.000000000000000000, 1.000000000000000000 ) ) ;
#35772 = LINE ( 'NONE', #29276, #24293 ) ;
#35773 = ORIENTED_EDGE ( 'NONE', *, *, #30811, .F. ) ;
#35774 = DIRECTION ( 'NONE',  ( -0.000000000000000000, -0.000000000000000000, 1.000000000000000000 ) ) ;
#35775 = VERTEX_POINT ( 'NONE', #18416 ) ;
#35776 = AXIS2_PLACEMENT_3D ( 'NONE', #6597, #39751, #23233 ) ;
#35777 = ORIENTED_EDGE ( 'NONE', *, *, #4486, .T. ) ;
#35778 = AXIS2_PLACEMENT_3D ( 'NONE', #16507, #34127, #17380 ) ;
#35779 = DIRECTION ( 'NONE',  ( 1.000000000000000000, 0.000000000000000000, 0.000000000000000000 ) ) ;
#35780 = CARTESIAN_POINT ( 'NONE',  ( 58.29702017945731285, 31.00000000000000000, 66.63806913872474524 ) ) ;
#35781 = ORIENTED_EDGE ( 'NONE', *, *, #23994, .T. ) ;
#35782 = DIRECTION ( 'NONE',  ( -1.000000000000000000, 0.000000000000000000, 0.000000000000000000 ) ) ;
#35783 = CIRCLE ( 'NONE', #15628, 58.99999999999999289 ) ;
#35784 = CYLINDRICAL_SURFACE ( 'NONE', #37260, 13.59999999999999964 ) ;
#35785 = DIRECTION ( 'NONE',  ( 0.000000000000000000, -0.6382441836448261574, 0.7698339834299012807 ) ) ;
#35786 = ORIENTED_EDGE ( 'NONE', *, *, #24802, .T. ) ;
#35787 = EDGE_CURVE ( 'NONE', #12205, #19014, #4755, .T. ) ;
#35788 = CYLINDRICAL_SURFACE ( 'NONE', #25941, 120.5010000000000190 ) ;
#35789 = DIRECTION ( 'NONE',  ( 1.000000000000000000, 0.000000000000000000, 0.000000000000000000 ) ) ;
#35790 = ADVANCED_FACE ( 'NONE', ( #11196 ), #28001, .F. ) ;
#35791 = CARTESIAN_POINT ( 'NONE',  ( 17.99999999999999645, 69.72480978690046527, 92.70626138606037614 ) ) ;
#35792 = EDGE_CURVE ( 'NONE', #8378, #21461, #8251, .T. ) ;
#35794 = CARTESIAN_POINT ( 'NONE',  ( 17.99999999999999645, -41.62036691425604573, 113.0850832732712945 ) ) ;
#35793 = CARTESIAN_POINT ( 'NONE',  ( 17.99999999999999645, -29.36437154452078246, 116.8684075565134890 ) ) ;
#35795 = DIRECTION ( 'NONE',  ( -1.058513553088275437E-16, -1.000000000000000000, 8.813324511995299047E-17 ) ) ;
#35796 = DIRECTION ( 'NONE',  ( 1.000000000000000000, 0.000000000000000000, 0.000000000000000000 ) ) ;
#35797 = EDGE_LOOP ( 'NONE', ( #23014, #38910, #26101, #14710 ) ) ;
#35798 = VECTOR ( 'NONE', #1328, 1000.000000000000000 ) ;
#35799 = CARTESIAN_POINT ( 'NONE',  ( 23.12883206328222130, 31.00000000000000355, 11.39561251172168355 ) ) ;
#35800 = ORIENTED_EDGE ( 'NONE', *, *, #24608, .T. ) ;
#35801 = CARTESIAN_POINT ( 'NONE',  ( 17.99999999999999645, -40.37724737310141165, 104.6802291180865865 ) ) ;
#35802 = DIRECTION ( 'NONE',  ( 0.000000000000000000, -0.9510565162951500895, -0.3090169943749582204 ) ) ;
#35803 = ORIENTED_EDGE ( 'NONE', *, *, #24492, .F. ) ;
#35804 = CLOSED_SHELL ( 'NONE', ( #29870, #11295, #3794, #40196, #13325, #10875, #3634, #18656, #31000, #41480, #4086, #3024, #8423, #19867, #24373, #16560, #38991, #11983, #37008, #7923, #13795, #36700, #31960, #14009, #29519, #36851, #40491, #43171, #29531, #6312, #7718, #24661, #12434, #26307, #26870, #20355, #11803, #26145, #20598, #3459, #29439, #30633, #1539 ) ) ;
#35805 = CARTESIAN_POINT ( 'NONE',  ( 42.20483333784007840, 40.00000000000000000, -14.33818270462009359 ) ) ;
#35806 = AXIS2_PLACEMENT_3D ( 'NONE', #18811, #29024, #32270 ) ;
#35807 = ADVANCED_FACE ( 'NONE', ( #10982 ), #28211, .T. ) ;
#35808 = CARTESIAN_POINT ( 'NONE',  ( 30.20675218207097501, 40.00000000000000000, 23.25504409023340813 ) ) ;
#35809 = ORIENTED_EDGE ( 'NONE', *, *, #39822, .F. ) ;
#35810 = AXIS2_PLACEMENT_3D ( 'NONE', #24019, #31199, #41194 ) ;
#35811 = EDGE_LOOP ( 'NONE', ( #3368, #11588, #2318, #19675 ) ) ;
#35812 = LINE ( 'NONE', #9012, #29718 ) ;
#35813 = DIRECTION ( 'NONE',  ( -1.000000000000000000, -0.000000000000000000, -0.000000000000000000 ) ) ;
#35814 = DIRECTION ( 'NONE',  ( 0.000000000000000000, 0.000000000000000000, 1.000000000000000000 ) ) ;
#35815 = VECTOR ( 'NONE', #14833, 1000.000000000000000 ) ;
#35816 = CARTESIAN_POINT ( 'NONE',  ( 17.99999999999999645, 0.000000000000000000, 0.000000000000000000 ) ) ;
#35817 = ADVANCED_FACE ( 'NONE', ( #37778 ), #7897, .T. ) ;
#35818 = DIRECTION ( 'NONE',  ( 0.000000000000000000, 0.3641605752528168649, 0.9313361774523405412 ) ) ;
#35819 = ADVANCED_FACE ( 'NONE', ( #21259 ), #34507, .F. ) ;
#35820 = DIRECTION ( 'NONE',  ( 1.000000000000000000, 0.000000000000000000, 0.000000000000000000 ) ) ;
#35821 = CIRCLE ( 'NONE', #7278, 47.49900000000000233 ) ;
#35822 = EDGE_LOOP ( 'NONE', ( #22287, #25370, #3509, #38530 ) ) ;
#35823 = CARTESIAN_POINT ( 'NONE',  ( 17.99999999999999645, 9.484061862024356415, -30.03730300138970932 ) ) ;
#35824 = ORIENTED_EDGE ( 'NONE', *, *, #39889, .T. ) ;
#35825 = CARTESIAN_POINT ( 'NONE',  ( 17.99999999999999645, -69.90696807222551001, 98.15042952503490881 ) ) ;
#35826 = DIRECTION ( 'NONE',  ( 0.000000000000000000, 0.000000000000000000, -1.000000000000000000 ) ) ;
#35827 = ADVANCED_FACE ( 'NONE', ( #14693 ), #11627, .T. ) ;
#35828 = DIRECTION ( 'NONE',  ( 1.000000000000000000, 0.000000000000000000, 0.000000000000000000 ) ) ;
#35829 = CARTESIAN_POINT ( 'NONE',  ( 18.00000000000000355, 32.32520163883631170, -34.09746168776002406 ) ) ;
#35830 = EDGE_CURVE ( 'NONE', #20361, #4481, #36788, .T. ) ;
#35831 = ORIENTED_EDGE ( 'NONE', *, *, #37501, .T. ) ;
#35832 = CARTESIAN_POINT ( 'NONE',  ( 57.05379307147669721, 39.99999999999999289, -74.37948018729004218 ) ) ;
#35833 = ORIENTED_EDGE ( 'NONE', *, *, #4465, .F. ) ;
#35834 = CARTESIAN_POINT ( 'NONE',  ( 17.99999999999999645, 111.9370513079675789, -44.61600100275060043 ) ) ;
#35835 = AXIS2_PLACEMENT_3D ( 'NONE', #19342, #32613, #43060 ) ;
#35836 = ORIENTED_EDGE ( 'NONE', *, *, #19364, .T. ) ;
#35838 = VERTEX_POINT ( 'NONE', #10746 ) ;
#35837 = CARTESIAN_POINT ( 'NONE',  ( 18.00000000000000355, -50.95304419620831737, 10.38206564895643957 ) ) ;
#35839 = CARTESIAN_POINT ( 'NONE',  ( -25.29816761085220378, 31.00000000000000355, 43.63644233510515846 ) ) ;
#35840 = ORIENTED_EDGE ( 'NONE', *, *, #39664, .T. ) ;
#35841 = CARTESIAN_POINT ( 'NONE',  ( 18.00000000000000355, 35.11945359308110426, 38.34871548466026070 ) ) ;
#35842 = CLOSED_SHELL ( 'NONE', ( #30823, #25016, #38873, #16413, #39693, #22107, #6551, #10871, #8686, #29764, #9603, #35807, #36847, #27075, #14089, #9981, #39937, #10208, #10370, #37118, #18654, #10060, #35714, #37246, #12673, #5115, #804, #23592, #40303, #5185, #31407, #30268, #28455, #31514, #9769, #15739, #21719, #25118, #42065, #42372, #21225, #1609, #4293, #23037, #38132, #32534, #28034, #13166, #23267, #9951, #15944, #34486, #29252, #32391, #21559, #24305, #40710, #5807, #26781 ) ) ;
#35843 = AXIS2_PLACEMENT_3D ( 'NONE', #6934, #20291, #27243 ) ;
#35844 = ORIENTED_EDGE ( 'NONE', *, *, #24339, .F. ) ;
#35845 = CARTESIAN_POINT ( 'NONE',  ( 0.000000000000000000, 0.000000000000000000, 0.000000000000000000 ) ) ;
#35846 = ORIENTED_EDGE ( 'NONE', *, *, #36161, .T. ) ;
#35847 = CARTESIAN_POINT ( 'NONE',  ( -35.33737842959504860, 40.00000000000000000, 60.98257694382487415 ) ) ;
#35848 = CIRCLE ( 'NONE', #32384, 12.49999999999993427 ) ;
#35849 = EDGE_CURVE ( 'NONE', #2932, #16830, #37481, .T. ) ;
#35851 = DIRECTION ( 'NONE',  ( 0.000000000000000000, 0.7525707698561396874, -0.6585113790650372056 ) ) ;
#35850 = CARTESIAN_POINT ( 'NONE',  ( 17.99999999999999645, -8.827181066046698277, 120.1772519049559378 ) ) ;
#35852 = PRODUCT_DEFINITION ( 'UNKNOWN', '', #25401, #29452 ) ;
#35853 = CIRCLE ( 'NONE', #5902, 59.00000000000000711 ) ;
#35854 = CYLINDRICAL_SURFACE ( 'NONE', #3160, 120.5010000000000190 ) ;
#35855 = ORIENTED_EDGE ( 'NONE', *, *, #25362, .F. ) ;
#35856 = CARTESIAN_POINT ( 'NONE',  ( 17.99999999999999645, 35.72777019205808813, -106.3569410558013715 ) ) ;
#35857 = ORIENTED_EDGE ( 'NONE', *, *, #7235, .F. ) ;
#35858 = FILL_AREA_STYLE_COLOUR ( '', #5087 ) ;
#35859 = AXIS2_PLACEMENT_3D ( 'NONE', #7291, #37827, #4897 ) ;
#35860 = DIRECTION ( 'NONE',  ( 0.000000000000000000, 0.000000000000000000, 1.000000000000000000 ) ) ;
#35861 = LINE ( 'NONE', #35653, #12974 ) ;
#35862 = CARTESIAN_POINT ( 'NONE',  ( -72.56464488860213180, 31.00000000000000711, -35.76892886290303863 ) ) ;
#35864 = CARTESIAN_POINT ( 'NONE',  ( 0.000000000000000000, -110.8621702203451065, 34.14058016547499363 ) ) ;
#35863 = FACE_OUTER_BOUND ( 'NONE', #28, .T. ) ;
#35865 = ADVANCED_FACE ( 'NONE', ( #20833 ), #17548, .T. ) ;
#35866 = ORIENTED_EDGE ( 'NONE', *, *, #13712, .T. ) ;
#35867 = ADVANCED_FACE ( 'NONE', ( #22745 ), #8759, .T. ) ;
#35868 =( NAMED_UNIT ( * ) SI_UNIT ( $, .STERADIAN. ) SOLID_ANGLE_UNIT ( ) );
#35869 = ORIENTED_EDGE ( 'NONE', *, *, #27266, .F. ) ;
#35870 = CARTESIAN_POINT ( 'NONE',  ( 10.50000000000000178, 0.000000000000000000, -1.199999999999999956 ) ) ;
#35871 = CARTESIAN_POINT ( 'NONE',  ( 0.000000000000000000, 0.000000000000000000, -4.000000000000000000 ) ) ;
#35872 = CARTESIAN_POINT ( 'NONE',  ( -26.02152878260477564, 31.00000000000000355, 96.68563202202810203 ) ) ;
#35873 = CARTESIAN_POINT ( 'NONE',  ( 25.57473013256711880, 40.00000000000000000, 95.94174708832935039 ) ) ;
#35874 = DIRECTION ( 'NONE',  ( -1.000000000000000000, -0.000000000000000000, -0.000000000000000000 ) ) ;
#35875 = CIRCLE ( 'NONE', #15039, 120.5010000000000190 ) ;
#35876 = CIRCLE ( 'NONE', #24832, 19.19999999999999574 ) ;
#35877 = EDGE_CURVE ( 'NONE', #10311, #35149, #35772, .T. ) ;
#35878 = VERTEX_POINT ( 'NONE', #32528 ) ;
#35879 = CARTESIAN_POINT ( 'NONE',  ( 17.99999999999999645, 115.9750404417044081, 2.406240749597859718 ) ) ;
#35880 = ORIENTED_EDGE ( 'NONE', *, *, #37002, .F. ) ;
#35881 = DIRECTION ( 'NONE',  ( 0.000000000000000000, 0.000000000000000000, 1.000000000000000000 ) ) ;
#35882 = CIRCLE ( 'NONE', #6615, 20.00000000000000711 ) ;
#35883 = EDGE_CURVE ( 'NONE', #28679, #35634, #22212, .T. ) ;
#35884 = AXIS2_PLACEMENT_3D ( 'NONE', #16495, #10356, #26720 ) ;
#35885 = DIRECTION ( 'NONE',  ( 0.000000000000000000, -0.5877852522924802425, 0.8090169943749422332 ) ) ;
#35886 = DIRECTION ( 'NONE',  ( 0.000000000000000000, -0.1253332335642905193, -0.9921147013144796523 ) ) ;
#35887 = EDGE_LOOP ( 'NONE', ( #3754, #30405 ) ) ;
#35888 = DIRECTION ( 'NONE',  ( -1.000000000000000000, -0.000000000000000000, 0.000000000000000000 ) ) ;
#35889 = CARTESIAN_POINT ( 'NONE',  ( 9.000000000000001776, 5.871425383722282731, -51.66745943012276143 ) ) ;
#35890 = CIRCLE ( 'NONE', #39375, 120.5010000000000190 ) ;
#35891 = DIRECTION ( 'NONE',  ( 0.000000000000000000, 0.000000000000000000, 1.000000000000000000 ) ) ;
#35893 = ORIENTED_EDGE ( 'NONE', *, *, #33329, .T. ) ;
#35892 = DIRECTION ( 'NONE',  ( 0.000000000000000000, 0.000000000000000000, 1.000000000000000000 ) ) ;
#35894 = CARTESIAN_POINT ( 'NONE',  ( -6.259644161404860030E-16, -4.618802153517027165, -3.433295621305388234 ) ) ;
#35895 = CARTESIAN_POINT ( 'NONE',  ( 18.00000000000000355, 0.000000000000000000, 0.000000000000000000 ) ) ;
#35897 = EDGE_LOOP ( 'NONE', ( #22716, #19595, #3267, #37636 ) ) ;
#35896 = DIRECTION ( 'NONE',  ( -1.000000000000000000, -0.000000000000000000, 0.000000000000000000 ) ) ;
#35898 = VERTEX_POINT ( 'NONE', #32110 ) ;
#35899 = CYLINDRICAL_SURFACE ( 'NONE', #11536, 59.00000000000000000 ) ;
#35900 = DIRECTION ( 'NONE',  ( 1.000000000000000000, 0.000000000000000000, 0.000000000000000000 ) ) ;
#35902 = AXIS2_PLACEMENT_3D ( 'NONE', #12720, #16428, #15789 ) ;
#35901 = CARTESIAN_POINT ( 'NONE',  ( 41.46880187714432253, 40.00000000000000000, 24.04226233541896107 ) ) ;
#35903 = DIRECTION ( 'NONE',  ( -1.000000000000000000, -0.000000000000000000, -0.000000000000000000 ) ) ;
#35904 = EDGE_CURVE ( 'NONE', #37232, #11603, #6833, .T. ) ;
#35905 = EDGE_CURVE ( 'NONE', #12448, #25238, #12486, .T. ) ;
#35906 = CARTESIAN_POINT ( 'NONE',  ( -1.747541505913277282, 3.837784562140256650, -3.503702292528906526 ) ) ;
#35907 = EDGE_CURVE ( 'NONE', #31256, #39874, #31923, .T. ) ;
#35908 = EDGE_CURVE ( 'NONE', #37599, #37475, #25597, .T. ) ;
#35909 = DIRECTION ( 'NONE',  ( -3.996523416598930318E-16, 2.658563593772947863E-15, 1.000000000000000000 ) ) ;
#35911 = ORIENTED_EDGE ( 'NONE', *, *, #8607, .F. ) ;
#35910 = AXIS2_PLACEMENT_3D ( 'NONE', #30785, #14003, #27301 ) ;
#35912 = DIRECTION ( 'NONE',  ( 0.000000000000000000, -0.8183027759081742403, 0.5747874102143992747 ) ) ;
#35913 = CIRCLE ( 'NONE', #26880, 20.00000000000000355 ) ;
#35914 = ORIENTED_EDGE ( 'NONE', *, *, #21848, .F. ) ;
#35915 = AXIS2_PLACEMENT_3D ( 'NONE', #24554, #923, #11012 ) ;
#35916 = DIRECTION ( 'NONE',  ( -1.000000000000000000, -0.000000000000000000, -0.000000000000000000 ) ) ;
#35917 = LINE ( 'NONE', #29618, #1764 ) ;
#35918 = AXIS2_PLACEMENT_3D ( 'NONE', #35074, #31825, #5187 ) ;
#35919 = CARTESIAN_POINT ( 'NONE',  ( -49.89583333467011528, 31.00000000000000355, 3.272492339034415831 ) ) ;
#35920 = DIRECTION ( 'NONE',  ( 1.000000000000000000, 0.000000000000000000, 0.000000000000000000 ) ) ;
#35922 = ORIENTED_EDGE ( 'NONE', *, *, #24149, .T. ) ;
#35921 = AXIS2_PLACEMENT_3D ( 'NONE', #24352, #37606, #7724 ) ;
#35923 = AXIS2_PLACEMENT_3D ( 'NONE', #26229, #6558, #19067 ) ;
#35925 = AXIS2_PLACEMENT_3D ( 'NONE', #40296, #33345, #37036 ) ;
#35924 = DIRECTION ( 'NONE',  ( -1.000000000000000000, -0.000000000000000000, -0.000000000000000000 ) ) ;
#35926 = ADVANCED_BREP_SHAPE_REPRESENTATION ( '', ( #28157, #13552 ), #41354 ) ;
#35927 = CARTESIAN_POINT ( 'NONE',  ( 84.73112319332513209, 31.00000000000000000, -41.78253223598262167 ) ) ;
#35928 = CARTESIAN_POINT ( 'NONE',  ( 1.598609366639573350E-14, -1.063425437509180407E-13, -40.00000000000000000 ) ) ;
#35929 = ORIENTED_EDGE ( 'NONE', *, *, #6908, .F. ) ;
#35930 = CARTESIAN_POINT ( 'NONE',  ( -28.16914340538000161, 31.00000000000000355, -57.36152490105312296 ) ) ;
#35931 = CARTESIAN_POINT ( 'NONE',  ( -64.10496366469683949, 40.00000000000000711, 31.48763712508877077 ) ) ;
#35932 = DIRECTION ( 'NONE',  ( 0.000000000000000000, 0.000000000000000000, 1.000000000000000000 ) ) ;
#35933 = ORIENTED_EDGE ( 'NONE', *, *, #27668, .F. ) ;
#35934 =( NAMED_UNIT ( * ) PLANE_ANGLE_UNIT ( ) SI_UNIT ( $, .RADIAN. ) );
#35935 = CARTESIAN_POINT ( 'NONE',  ( 0.000000000000000000, -52.19040376560366923, -99.31985817764231683 ) ) ;
#35936 = CARTESIAN_POINT ( 'NONE',  ( 17.99999999999999645, 25.46650492921924425, -19.29328419707757547 ) ) ;
#35938 = VERTEX_POINT ( 'NONE', #15979 ) ;
#35937 = DIRECTION ( 'NONE',  ( 1.000000000000000000, 0.000000000000000000, 0.000000000000000000 ) ) ;
#35939 = AXIS2_PLACEMENT_3D ( 'NONE', #17679, #6143, #10449 ) ;
#35940 = DIRECTION ( 'NONE',  ( 0.000000000000000000, -0.9574220383620081209, 0.2886919473396123981 ) ) ;
#35941 = AXIS2_PLACEMENT_3D ( 'NONE', #16598, #16357, #32705 ) ;
#35942 = DIRECTION ( 'NONE',  ( -1.000000000000000000, 0.000000000000000000, 0.000000000000000000 ) ) ;
#35943 = AXIS2_PLACEMENT_3D ( 'NONE', #19774, #36741, #43069 ) ;
#35944 = CARTESIAN_POINT ( 'NONE',  ( -5.072363130230006512, 40.00000000000000000, 77.60416666578095146 ) ) ;
#35945 = DIRECTION ( 'NONE',  ( -1.000000000000000000, 0.000000000000000000, 0.000000000000000000 ) ) ;
#35946 = COLOUR_RGB ( '', 0.31764706, 0.68627451, 0.89019608) ;
#35947 = ORIENTED_EDGE ( 'NONE', *, *, #7623, .T. ) ;
#35948 = CARTESIAN_POINT ( 'NONE',  ( 8.999999999999998224, -78.18175027177490222, 85.69488855492974722 ) ) ;
#35949 = LINE ( 'NONE', #29650, #37779 ) ;
#35950 = CIRCLE ( 'NONE', #14378, 19.99999999999999645 ) ;
#35951 = AXIS2_PLACEMENT_3D ( 'NONE', #17729, #10284, #14442 ) ;
#35952 = ORIENTED_EDGE ( 'NONE', *, *, #25257, .F. ) ;
#35953 = CIRCLE ( 'NONE', #35288, 51.99999999999999289 ) ;
#35954 = EDGE_LOOP ( 'NONE', ( #7176, #18396, #7265, #3522 ) ) ;
#35955 = CARTESIAN_POINT ( 'NONE',  ( 0.000000000000000000, 23.87611429743662939, 20.54551452399628531 ) ) ;
#35956 = ORIENTED_EDGE ( 'NONE', *, *, #18406, .F. ) ;
#35957 = DIRECTION ( 'NONE',  ( -1.000000000000000000, 0.000000000000000000, 0.000000000000000000 ) ) ;
#35958 = DIRECTION ( 'NONE',  ( -1.000000000000000000, 0.000000000000000000, 0.000000000000000000 ) ) ;
#35959 = DIRECTION ( 'NONE',  ( -1.000000000000000000, 3.469446951953614189E-17, 0.000000000000000000 ) ) ;
#35960 = EDGE_CURVE ( 'NONE', #21443, #4850, #32625, .T. ) ;
#35961 = EDGE_CURVE ( 'NONE', #16718, #12969, #42112, .T. ) ;
#35962 = CARTESIAN_POINT ( 'NONE',  ( 17.99999999999999645, -21.56073507908662634, 23.57770962728557151 ) ) ;
#35963 = VERTEX_POINT ( 'NONE', #22327 ) ;
#35964 = CARTESIAN_POINT ( 'NONE',  ( 18.00000000000000355, -37.91532898920899441, -28.61088654061679648 ) ) ;
#35965 = PRODUCT_DEFINITION_CONTEXT ( 'detailed design', #35625, 'design' ) ;
#35966 = EDGE_CURVE ( 'NONE', #5690, #35289, #5443, .T. ) ;
#35967 = ORIENTED_EDGE ( 'NONE', *, *, #12479, .T. ) ;
#35968 = DIRECTION ( 'NONE',  ( -1.000000000000000000, -0.000000000000000000, -0.000000000000000000 ) ) ;
#35970 = ORIENTED_EDGE ( 'NONE', *, *, #35907, .T. ) ;
#35969 = CIRCLE ( 'NONE', #25596, 2.649999999999985700 ) ;
#35971 = DIRECTION ( 'NONE',  ( 1.000000000000000000, -0.000000000000000000, -0.000000000000000000 ) ) ;
#35972 = AXIS2_PLACEMENT_3D ( 'NONE', #34926, #5038, #28187 ) ;
#35973 = DIRECTION ( 'NONE',  ( 0.000000000000000000, 0.000000000000000000, 1.000000000000000000 ) ) ;
#35974 = CIRCLE ( 'NONE', #21414, 116.0000000000000000 ) ;
#35975 = AXIS2_PLACEMENT_3D ( 'NONE', #31993, #21986, #19355 ) ;
#35976 = CONTEXT_DEPENDENT_SHAPE_REPRESENTATION ( #2735, #10618 ) ;
#35977 = CARTESIAN_POINT ( 'NONE',  ( 17.99999999999999645, -110.0562500189201955, 49.07252625220073838 ) ) ;
#35978 = CARTESIAN_POINT ( 'NONE',  ( -58.48566925783705983, 31.00000000000000711, -15.65830181327787862 ) ) ;
#35979 = PRESENTATION_LAYER_ASSIGNMENT (  '', '', ( #2525 ) ) ;
#35980 = CARTESIAN_POINT ( 'NONE',  ( 22.90854556226730310, -34.05525454449573175, -74.83297477053802993 ) ) ;
#35981 = EDGE_CURVE ( 'NONE', #29037, #189, #13846, .T. ) ;
#35982 = ORIENTED_EDGE ( 'NONE', *, *, #21305, .F. ) ;
#35983 = CARTESIAN_POINT ( 'NONE',  ( 36.20216622922067273, 31.00000000000000355, 9.761693653842600682 ) ) ;
#35984 = CARTESIAN_POINT ( 'NONE',  ( 8.815036365794538753, 40.00000000000000000, 66.85656860134390911 ) ) ;
#35985 = VECTOR ( 'NONE', #7150, 1000.000000000000000 ) ;
#35986 = VECTOR ( 'NONE', #22607, 1000.000000000000000 ) ;
#35987 = CYLINDRICAL_SURFACE ( 'NONE', #7434, 12.50000000000000000 ) ;
#35988 = CARTESIAN_POINT ( 'NONE',  ( 17.99999999999999645, 7.749090474611513457, 30.53094492177216068 ) ) ;
#35989 = DIRECTION ( 'NONE',  ( -1.000000000000000000, 0.000000000000000000, 0.000000000000000000 ) ) ;
#35990 = EDGE_CURVE ( 'NONE', #9735, #24321, #16622, .T. ) ;
#35991 = CARTESIAN_POINT ( 'NONE',  ( 17.99999999999999645, 0.000000000000000000, 0.000000000000000000 ) ) ;
#35992 = ORIENTED_EDGE ( 'NONE', *, *, #22850, .T. ) ;
#35993 = CARTESIAN_POINT ( 'NONE',  ( 5.583751958424166162, 40.00000000000000000, -42.43436172917101601 ) ) ;
#35994 = DIRECTION ( 'NONE',  ( 0.000000000000000000, 0.000000000000000000, 1.000000000000000000 ) ) ;
#35995 = DIRECTION ( 'NONE',  ( 1.000000000000000000, -0.000000000000000000, 0.000000000000000000 ) ) ;
#35996 = ORIENTED_EDGE ( 'NONE', *, *, #20205, .T. ) ;
#35997 = AXIS2_PLACEMENT_3D ( 'NONE', #36582, #20487, #4281 ) ;
#35998 = CARTESIAN_POINT ( 'NONE',  ( 0.000000000000000000, -94.52951811191606168, 67.23221107124869889 ) ) ;
#35999 = CARTESIAN_POINT ( 'NONE',  ( -8.920000000000003482, 0.000000000000000000, 0.000000000000000000 ) ) ;
#36000 = ORIENTED_EDGE ( 'NONE', *, *, #7845, .F. ) ;
#36001 = DIRECTION ( 'NONE',  ( 0.000000000000000000, 0.7164567402983164079, -0.6976315211349833900 ) ) ;
#36002 = ORIENTED_EDGE ( 'NONE', *, *, #41841, .T. ) ;
#36003 = CIRCLE ( 'NONE', #38784, 13.59999999999999787 ) ;
#36004 = CIRCLE ( 'NONE', #39489, 120.5010000000000332 ) ;
#36005 = ORIENTED_EDGE ( 'NONE', *, *, #9278, .F. ) ;
#36006 = AXIS2_PLACEMENT_3D ( 'NONE', #5260, #18627, #34934 ) ;
#36007 = FACE_OUTER_BOUND ( 'NONE', #31509, .T. ) ;
#36008 = CARTESIAN_POINT ( 'NONE',  ( 86.58052584568748955, 31.00000000000000000, -42.55516686010645344 ) ) ;
#36009 = ORIENTED_EDGE ( 'NONE', *, *, #14964, .F. ) ;
#36010 = CARTESIAN_POINT ( 'NONE',  ( 17.99999999999999645, 0.000000000000000000, 0.000000000000000000 ) ) ;
#36011 = CIRCLE ( 'NONE', #26336, 59.00000000000000000 ) ;
#36012 = CARTESIAN_POINT ( 'NONE',  ( 18.00000000000000355, 44.25018368420781201, -27.31155879685132959 ) ) ;
#36013 = EDGE_CURVE ( 'NONE', #29671, #33336, #25802, .T. ) ;
#36014 = DIRECTION ( 'NONE',  ( 0.000000000000000000, -0.2631025642275089393, -0.9647678688145192583 ) ) ;
#36015 = ORIENTED_EDGE ( 'NONE', *, *, #33439, .T. ) ;
#36016 = DIRECTION ( 'NONE',  ( -1.000000000000000000, -0.000000000000000000, 0.000000000000000000 ) ) ;
#36017 = CIRCLE ( 'NONE', #12979, 20.00000000000000355 ) ;
#36018 = PRODUCT_RELATED_PRODUCT_CATEGORY ( 'part', '', ( #16177 ) ) ;
#36019 = LINE ( 'NONE', #37264, #13681 ) ;
#36020 = DIRECTION ( 'NONE',  ( 0.000000000000000000, 0.000000000000000000, 1.000000000000000000 ) ) ;
#36022 = DIRECTION ( 'NONE',  ( -1.000000000000000000, -0.000000000000000000, -0.000000000000000000 ) ) ;
#36021 = CYLINDRICAL_SURFACE ( 'NONE', #17598, 13.60000000000000142 ) ;
#36023 = EDGE_CURVE ( 'NONE', #34509, #21207, #34713, .T. ) ;
#36024 = CARTESIAN_POINT ( 'NONE',  ( 0.000000000000000000, 0.000000000000000000, 0.000000000000000000 ) ) ;
#36025 = VERTEX_POINT ( 'NONE', #29066 ) ;
#36026 = EDGE_CURVE ( 'NONE', #33221, #25771, #40956, .T. ) ;
#36027 = CARTESIAN_POINT ( 'NONE',  ( 22.42277067908921850, 31.00000000000000355, 12.94072372014797701 ) ) ;
#36028 = ORIENTED_EDGE ( 'NONE', *, *, #5886, .T. ) ;
#36029 = CARTESIAN_POINT ( 'NONE',  ( 18.00000000000000355, 0.000000000000000000, 0.000000000000000000 ) ) ;
#36030 = ADVANCED_FACE ( 'NONE', ( #39059 ), #41706, .F. ) ;
#36031 = DIRECTION ( 'NONE',  ( -1.000000000000000000, -0.000000000000000000, 0.000000000000000000 ) ) ;
#36032 = AXIS2_PLACEMENT_3D ( 'NONE', #40449, #20655, #29814 ) ;
#36033 = ORIENTED_EDGE ( 'NONE', *, *, #20915, .T. ) ;
#36034 = DIRECTION ( 'NONE',  ( -1.000000000000000000, -0.000000000000000000, -0.000000000000000000 ) ) ;
#36035 = CARTESIAN_POINT ( 'NONE',  ( -25.53337963587170023, 40.00000000000000000, 29.12008199578403023 ) ) ;
#36036 = AXIS2_PLACEMENT_3D ( 'NONE', #9862, #461, #40385 ) ;
#36037 = CARTESIAN_POINT ( 'NONE',  ( -31.36635120280305955, 40.00000000000000000, -8.451140850655482595 ) ) ;
#36038 = AXIS2_PLACEMENT_3D ( 'NONE', #29724, #13153, #39506 ) ;
#36039 = CIRCLE ( 'NONE', #7498, 31.49899999999999878 ) ;
#36040 = ORIENTED_EDGE ( 'NONE', *, *, #5064, .T. ) ;
#36041 = AXIS2_PLACEMENT_3D ( 'NONE', #30455, #4017, #34139 ) ;
#36042 = ORIENTED_EDGE ( 'NONE', *, *, #17978, .F. ) ;
#36043 = CARTESIAN_POINT ( 'NONE',  ( 8.919999999999999929, 0.000000000000000000, 0.000000000000000000 ) ) ;
#36044 = FACE_OUTER_BOUND ( 'NONE', #2571, .T. ) ;
#36045 = CIRCLE ( 'NONE', #39528, 116.0000000000000000 ) ;
#36046 = CARTESIAN_POINT ( 'NONE',  ( 0.000000000000000000, 57.40245293794799153, -96.40140491896575270 ) ) ;
#36048 = EDGE_CURVE ( 'NONE', #14037, #28151, #27766, .T. ) ;
#36047 = CARTESIAN_POINT ( 'NONE',  ( 2.500000000000000000, -1.768423874527823569, 1.021000000000002350 ) ) ;
#36049 = DIRECTION ( 'NONE',  ( 1.000000000000000000, 0.000000000000000000, 0.000000000000000000 ) ) ;
#36050 = ORIENTED_EDGE ( 'NONE', *, *, #4701, .T. ) ;
#36051 = CARTESIAN_POINT ( 'NONE',  ( 0.000000000000000000, 40.37724737310070111, 104.6802291180868565 ) ) ;
#36052 = ORIENTED_EDGE ( 'NONE', *, *, #18500, .F. ) ;
#36053 = DIRECTION ( 'NONE',  ( 0.000000000000000000, 0.000000000000000000, 1.000000000000000000 ) ) ;
#36054 = EDGE_CURVE ( 'NONE', #34436, #23020, #31906, .T. ) ;
#36055 = DIRECTION ( 'NONE',  ( 0.000000000000000000, -0.3612416661871405976, -0.9324722294043605864 ) ) ;
#36056 = VECTOR ( 'NONE', #3802, 999.9999999999998863 ) ;
#36057 = FACE_OUTER_BOUND ( 'NONE', #2135, .T. ) ;
#36058 = DIRECTION ( 'NONE',  ( 0.000000000000000000, 0.000000000000000000, 1.000000000000000000 ) ) ;
#36059 = VERTEX_POINT ( 'NONE', #3677 ) ;
#36060 = DIRECTION ( 'NONE',  ( -1.000000000000000000, -0.000000000000000000, 0.000000000000000000 ) ) ;
#36061 = EDGE_LOOP ( 'NONE', ( #38668, #36614, #32109, #36900 ) ) ;
#36062 = LINE ( 'NONE', #12966, #20492 ) ;
#36063 = ORIENTED_EDGE ( 'NONE', *, *, #27625, .T. ) ;
#36065 = ORIENTED_EDGE ( 'NONE', *, *, #7276, .T. ) ;
#36064 = CARTESIAN_POINT ( 'NONE',  ( 0.000000000000000000, -114.1529630473452386, 38.59523323561398200 ) ) ;
#36066 = CARTESIAN_POINT ( 'NONE',  ( 3.665567271000699012, 31.00000000000000355, -54.59530427605618996 ) ) ;
#36067 = ORIENTED_EDGE ( 'NONE', *, *, #34347, .T. ) ;
#36068 = DIRECTION ( 'NONE',  ( 3.009274222672345096E-17, 1.000000000000000000, -2.455023325076455345E-18 ) ) ;
#36069 = AXIS2_PLACEMENT_3D ( 'NONE', #37131, #19956, #33869 ) ;
#36070 = AXIS2_PLACEMENT_3D ( 'NONE', #35142, #22314, #35563 ) ;
#36071 = EDGE_CURVE ( 'NONE', #32693, #30365, #4040, .T. ) ;
#36072 = VERTEX_POINT ( 'NONE', #33170 ) ;
#36073 = VECTOR ( 'NONE', #31134, 1000.000000000000000 ) ;
#36074 = DIRECTION ( 'NONE',  ( 0.000000000000000000, 0.000000000000000000, 1.000000000000000000 ) ) ;
#36075 = ORIENTED_EDGE ( 'NONE', *, *, #22986, .T. ) ;
#36076 = AXIS2_PLACEMENT_3D ( 'NONE', #18021, #24550, #4206 ) ;
#36077 = CARTESIAN_POINT ( 'NONE',  ( 37.84579180138899090, 40.00000000000000000, -65.31998993212283722 ) ) ;
#36078 = CIRCLE ( 'NONE', #538, 47.49900000000000233 ) ;
#36080 = CARTESIAN_POINT ( 'NONE',  ( 17.99999999999999645, -84.62908780824929522, 85.78116633471262276 ) ) ;
#36079 = DIRECTION ( 'NONE',  ( -1.000000000000000000, -0.000000000000000000, 0.000000000000000000 ) ) ;
#36081 = DIRECTION ( 'NONE',  ( 0.000000000000000000, 0.000000000000000000, 1.000000000000000000 ) ) ;
#36082 = ORIENTED_EDGE ( 'NONE', *, *, #20368, .F. ) ;
#36083 = CARTESIAN_POINT ( 'NONE',  ( 17.99999999999999645, -110.3490479609630910, -20.28201389785511211 ) ) ;
#36084 = VERTEX_POINT ( 'NONE', #19681 ) ;
#36085 = EDGE_CURVE ( 'NONE', #12374, #6899, #10262, .T. ) ;
#36086 = DIRECTION ( 'NONE',  ( 1.000000000000000000, 0.000000000000000000, 0.000000000000000000 ) ) ;
#36087 = CARTESIAN_POINT ( 'NONE',  ( 17.99999999999999645, -28.35267316522768155, -22.18391138608739155 ) ) ;
#36088 = CARTESIAN_POINT ( 'NONE',  ( -39.25113411183426848, 31.00000000000000355, 67.98392962655870519 ) ) ;
#36090 = DIRECTION ( 'NONE',  ( -1.000000000000000000, 0.000000000000000000, -0.000000000000000000 ) ) ;
#36089 = DIRECTION ( 'NONE',  ( -1.000000000000000000, 0.000000000000000000, -0.000000000000000000 ) ) ;
#36091 = CIRCLE ( 'NONE', #17244, 116.0000000000000000 ) ;
#36092 = ORIENTED_EDGE ( 'NONE', *, *, #2558, .F. ) ;
#36093 = EDGE_CURVE ( 'NONE', #38913, #17808, #15234, .T. ) ;
#36094 = FACE_OUTER_BOUND ( 'NONE', #16363, .T. ) ;
#36095 = ORIENTED_EDGE ( 'NONE', *, *, #35186, .T. ) ;
#36096 = CARTESIAN_POINT ( 'NONE',  ( 0.000000000000000000, -31.80866420683989304, -2.997093558041628025 ) ) ;
#36097 = CARTESIAN_POINT ( 'NONE',  ( 9.000000000000001776, -49.25004636492400323, 16.68630974939742018 ) ) ;
#36098 = AXIS2_PLACEMENT_3D ( 'NONE', #35999, #38422, #2393 ) ;
#36099 = CARTESIAN_POINT ( 'NONE',  ( -56.91377077966711084, 31.00000000000000355, -74.37798324515208037 ) ) ;
#36100 = AXIS2_PLACEMENT_3D ( 'NONE', #15303, #2569, #21642 ) ;
#36101 = CARTESIAN_POINT ( 'NONE',  ( 93.52153384685561832, 39.99999999999999289, -24.92737483788710762 ) ) ;
#36102 = DIRECTION ( 'NONE',  ( -1.000000000000000000, -0.000000000000000000, -0.000000000000000000 ) ) ;
#36103 = CIRCLE ( 'NONE', #43044, 59.00000000000000000 ) ;
#36104 = DIRECTION ( 'NONE',  ( 0.000000000000000000, 0.000000000000000000, 1.000000000000000000 ) ) ;
#36105 = ORIENTED_EDGE ( 'NONE', *, *, #35083, .F. ) ;
#36106 = FACE_OUTER_BOUND ( 'NONE', #30028, .T. ) ;
#36107 = EDGE_LOOP ( 'NONE', ( #13910, #19941, #19054, #36737 ) ) ;
#36108 = ADVANCED_FACE ( 'NONE', ( #26852 ), #6536, .T. ) ;
#36109 = VECTOR ( 'NONE', #5947, 1000.000000000000000 ) ;
#36110 = CARTESIAN_POINT ( 'NONE',  ( 18.00000000000000355, 1.836970198721029589E-15, -15.00000000000000000 ) ) ;
#36111 = EDGE_CURVE ( 'NONE', #990, #26550, #1939, .T. ) ;
#36112 = DIRECTION ( 'NONE',  ( 0.000000000000000000, 0.000000000000000000, 1.000000000000000000 ) ) ;
#36113 = DIRECTION ( 'NONE',  ( 0.000000000000000000, -0.2113826236296314776, 0.9774033898178651203 ) ) ;
#36114 = ORIENTED_EDGE ( 'NONE', *, *, #21622, .F. ) ;
#36115 = FACE_BOUND ( 'NONE', #7412, .T. ) ;
#36116 = DIRECTION ( 'NONE',  ( 0.000000000000000000, 0.9980267284282713369, 0.06279051952931692659 ) ) ;
#36117 = DIRECTION ( 'NONE',  ( -0.000000000000000000, -0.000000000000000000, 1.000000000000000000 ) ) ;
#36119 = EDGE_LOOP ( 'NONE', ( #32118, #39206, #29402, #40704 ) ) ;
#36118 = DIRECTION ( 'NONE',  ( 0.000000000000000000, -0.7525707698561308057, -0.6585113790650474197 ) ) ;
#36120 = CARTESIAN_POINT ( 'NONE',  ( -3.264650091097280831E-13, -4.796980096169642493, -3.721999068284424617 ) ) ;
#36121 = LINE ( 'NONE', #32647, #11366 ) ;
#36123 = ORIENTED_EDGE ( 'NONE', *, *, #6960, .F. ) ;
#36122 = DIRECTION ( 'NONE',  ( -1.000000000000000000, -0.000000000000000000, -0.000000000000000000 ) ) ;
#36124 = EDGE_LOOP ( 'NONE', ( #8565, #26912 ) ) ;
#36125 = CARTESIAN_POINT ( 'NONE',  ( 0.000000000000000000, -87.74575819880118388, -75.87280091124561920 ) ) ;
#36126 = CARTESIAN_POINT ( 'NONE',  ( 18.00000000000000355, 30.03615769709791650, -42.44795908868957923 ) ) ;
#36127 = CARTESIAN_POINT ( 'NONE',  ( -34.17541447290003020, 40.00000000000000000, -26.31327426976606887 ) ) ;
#36128 = DIRECTION ( 'NONE',  ( 0.000000000000000000, 1.000000000000000000, 0.000000000000000000 ) ) ;
#36129 = EDGE_CURVE ( 'NONE', #5117, #37475, #36820, .T. ) ;
#36130 = VECTOR ( 'NONE', #6442, 1000.000000000000000 ) ;
#36131 = DIRECTION ( 'NONE',  ( 0.000000000000000000, 0.000000000000000000, 1.000000000000000000 ) ) ;
#36132 = CARTESIAN_POINT ( 'NONE',  ( 18.00000000000000355, 51.93417535146740960, 2.615612846549358217 ) ) ;
#36133 = VERTEX_POINT ( 'NONE', #7187 ) ;
#36134 = AXIS2_PLACEMENT_3D ( 'NONE', #947, #14741, #40877 ) ;
#36135 = DIRECTION ( 'NONE',  ( -1.000000000000000000, 0.000000000000000000, 0.000000000000000000 ) ) ;
#36136 = ORIENTED_EDGE ( 'NONE', *, *, #41189, .F. ) ;
#36137 = ADVANCED_FACE ( 'NONE', ( #2822 ), #27081, .F. ) ;
#36138 = DIRECTION ( 'NONE',  ( -1.000000000000000000, -0.000000000000000000, -0.000000000000000000 ) ) ;
#36139 = CARTESIAN_POINT ( 'NONE',  ( -4.211140560182196957, -2.431303136016552013, -3.745885042887436178 ) ) ;
#36140 = EDGE_CURVE ( 'NONE', #26427, #16104, #41718, .T. ) ;
#36141 = CARTESIAN_POINT ( 'NONE',  ( 39.77940265867437120, 31.00000000000000355, 22.96373720238702276 ) ) ;
#36142 = DIRECTION ( 'NONE',  ( 1.000000000000000000, 0.000000000000000000, 0.000000000000000000 ) ) ;
#36143 = ORIENTED_EDGE ( 'NONE', *, *, #4244, .T. ) ;
#36144 = CARTESIAN_POINT ( 'NONE',  ( 155.7547826636224499, -2.055254544495727309, 15.74958860255448734 ) ) ;
#36145 = CARTESIAN_POINT ( 'NONE',  ( 94.17930118497612568, 31.00000000000000000, -12.41473344271720691 ) ) ;
#36146 = CARTESIAN_POINT ( 'NONE',  ( 0.000000000000000000, 115.9387338813862129, -3.769613505534868736 ) ) ;
#36147 = ORIENTED_EDGE ( 'NONE', *, *, #27805, .T. ) ;
#36148 = CARTESIAN_POINT ( 'NONE',  ( 41.67488199336423804, 31.00000000000000355, 54.49293397273885375 ) ) ;
#36149 = CARTESIAN_POINT ( 'NONE',  ( 59.60939625460783731, 39.99999999999999289, -29.27517545779414831 ) ) ;
#36150 = CARTESIAN_POINT ( 'NONE',  ( 17.99999999999999645, 8.827181066047508295, -120.1772519049558667 ) ) ;
#36151 = EDGE_LOOP ( 'NONE', ( #42033, #3789, #18683, #682 ) ) ;
#36152 = CARTESIAN_POINT ( 'NONE',  ( 0.000000000000000000, 0.000000000000000000, 0.000000000000000000 ) ) ;
#36153 = EDGE_CURVE ( 'NONE', #6816, #40515, #19455, .T. ) ;
#36154 = DIRECTION ( 'NONE',  ( -1.000000000000000000, -0.000000000000000000, -0.000000000000000000 ) ) ;
#36155 = CARTESIAN_POINT ( 'NONE',  ( 10.50000000000000178, 0.000000000000000000, 0.000000000000000000 ) ) ;
#36157 = EDGE_CURVE ( 'NONE', #40496, #27281, #3026, .T. ) ;
#36156 = CIRCLE ( 'NONE', #38256, 20.00000000000000711 ) ;
#36158 = AXIS2_PLACEMENT_3D ( 'NONE', #32213, #28104, #11751 ) ;
#36159 = EDGE_CURVE ( 'NONE', #23236, #9115, #33597, .T. ) ;
#36160 = EDGE_CURVE ( 'NONE', #6816, #9805, #16397, .T. ) ;
#36161 = EDGE_CURVE ( 'NONE', #29681, #4294, #8960, .T. ) ;
#36163 = ORIENTED_EDGE ( 'NONE', *, *, #11471, .F. ) ;
#36162 = DIRECTION ( 'NONE',  ( -1.000000000000000000, 0.000000000000000000, 0.000000000000000000 ) ) ;
#36164 = FACE_OUTER_BOUND ( 'NONE', #799, .T. ) ;
#36165 = DIRECTION ( 'NONE',  ( -1.000000000000000000, 0.000000000000000000, -0.000000000000000000 ) ) ;
#36166 = CIRCLE ( 'NONE', #18113, 11.00000000000000178 ) ;
#36167 = CARTESIAN_POINT ( 'NONE',  ( 32.44529481510334534, 40.00000000000000000, -65.82339768528792945 ) ) ;
#36168 = LINE ( 'NONE', #19847, #31273 ) ;
#36169 = EDGE_LOOP ( 'NONE', ( #12662, #27349, #13840, #7128 ) ) ;
#36170 = LINE ( 'NONE', #35948, #8785 ) ;
#36171 = LINE ( 'NONE', #29440, #27339 ) ;
#36172 = ORIENTED_EDGE ( 'NONE', *, *, #11676, .F. ) ;
#36173 = ORIENTED_EDGE ( 'NONE', *, *, #4725, .T. ) ;
#36174 = AXIS2_PLACEMENT_3D ( 'NONE', #14832, #37272, #23793 ) ;
#36175 = DIRECTION ( 'NONE',  ( 0.000000000000000000, -0.8443279255020087470, -0.5358267949790064266 ) ) ;
#36176 = ORIENTED_EDGE ( 'NONE', *, *, #41189, .T. ) ;
#36177 = CARTESIAN_POINT ( 'NONE',  ( 17.99999999999999645, 16.77566611177940104, -119.3275660838940553 ) ) ;
#36178 = DIRECTION ( 'NONE',  ( 1.000000000000000000, -1.373900992973641868E-15, -3.273063162220443081E-16 ) ) ;
#36179 = CARTESIAN_POINT ( 'NONE',  ( -100.6569797752917879, -2.055254544495720648, -8.979913733870429127 ) ) ;
#36180 = DIRECTION ( 'NONE',  ( -1.000000000000000000, 0.000000000000000000, 0.000000000000000000 ) ) ;
#36181 = ORIENTED_EDGE ( 'NONE', *, *, #24496, .F. ) ;
#36182 = LINE ( 'NONE', #2996, #7743 ) ;
#36183 = ORIENTED_EDGE ( 'NONE', *, *, #3884, .F. ) ;
#36184 = ADVANCED_FACE ( 'NONE', ( #30342 ), #40346, .F. ) ;
#36185 = AXIS2_PLACEMENT_3D ( 'NONE', #13468, #96, #22885 ) ;
#36186 = CARTESIAN_POINT ( 'NONE',  ( 0.000000000000000000, 23.10276247328100396, 118.2656051737070726 ) ) ;
#36187 = EDGE_CURVE ( 'NONE', #25951, #40496, #32658, .T. ) ;
#36188 = AXIS2_PLACEMENT_3D ( 'NONE', #36709, #33, #16907 ) ;
#36189 = VERTEX_POINT ( 'NONE', #23819 ) ;
#36190 = DIRECTION ( 'NONE',  ( -0.000000000000000000, -0.000000000000000000, 1.000000000000000000 ) ) ;
#36191 = EDGE_CURVE ( 'NONE', #33535, #39762, #42746, .T. ) ;
#36192 = CARTESIAN_POINT ( 'NONE',  ( -17.44537629401976631, 39.99999999999999289, -4.261559264950514958 ) ) ;
#36193 = CIRCLE ( 'NONE', #27067, 20.00000000000000000 ) ;
#36194 = APPLICATION_PROTOCOL_DEFINITION ( 'draft international standard', 'automotive_design', 1998, #767 ) ;
#36195 = CARTESIAN_POINT ( 'NONE',  ( 0.000000000000000000, 31.94619804602787738, -16.59639811537323340 ) ) ;
#36196 = CARTESIAN_POINT ( 'NONE',  ( 25.16436199730139123, 31.00000000000000355, 51.02488717759543135 ) ) ;
#36197 = ORIENTED_EDGE ( 'NONE', *, *, #40881, .F. ) ;
#36198 = CARTESIAN_POINT ( 'NONE',  ( -20.28213647682921206, 31.00000000000000355, 23.06128528321892546 ) ) ;
#36199 = CARTESIAN_POINT ( 'NONE',  ( -51.86900026051868196, 40.00000000000000000, 45.50549606403863123 ) ) ;
#36200 = DIRECTION ( 'NONE',  ( 0.000000000000000000, 0.6382441836448161654, 0.7698339834299094964 ) ) ;
#36201 = CYLINDRICAL_SURFACE ( 'NONE', #1944, 59.00000000000000000 ) ;
#36202 = EDGE_CURVE ( 'NONE', #28580, #26637, #39907, .T. ) ;
#36203 = ADVANCED_FACE ( 'NONE', ( #26212 ), #6336, .F. ) ;
#36204 = CYLINDRICAL_SURFACE ( 'NONE', #10687, 116.0000000000000000 ) ;
#36205 = CARTESIAN_POINT ( 'NONE',  ( 9.000000000000001776, -6.854627147197943415, -115.7972974066014018 ) ) ;
#36206 = EDGE_CURVE ( 'NONE', #7972, #6816, #23629, .T. ) ;
#36207 = ORIENTED_EDGE ( 'NONE', *, *, #32703, .T. ) ;
#36208 = CARTESIAN_POINT ( 'NONE',  ( 45.10416666515585860, 40.00000000000000000, 2.945243104263102651 ) ) ;
#36209 = DIRECTION ( 'NONE',  ( 0.000000000000000000, 0.000000000000000000, 1.000000000000000000 ) ) ;
#36211 = DIRECTION ( 'NONE',  ( 1.000000000000000000, 0.000000000000000000, 0.000000000000000000 ) ) ;
#36210 = AXIS2_PLACEMENT_3D ( 'NONE', #26467, #17482, #15 ) ;
#36212 = VERTEX_POINT ( 'NONE', #34040 ) ;
#36213 = VECTOR ( 'NONE', #196, 1000.000000000000000 ) ;
#36214 = CARTESIAN_POINT ( 'NONE',  ( 0.000000000000000000, 0.000000000000000000, 0.000000000000000000 ) ) ;
#36215 = DIRECTION ( 'NONE',  ( -1.000000000000000000, 0.000000000000000000, -0.000000000000000000 ) ) ;
#36216 = VERTEX_POINT ( 'NONE', #21434 ) ;
#36217 = DIRECTION ( 'NONE',  ( 1.000000000000000000, 0.000000000000000000, 0.000000000000000000 ) ) ;
#36218 = ORIENTED_EDGE ( 'NONE', *, *, #38470, .T. ) ;
#36219 = EDGE_LOOP ( 'NONE', ( #15472, #8502, #14352, #28324 ) ) ;
#36220 = CARTESIAN_POINT ( 'NONE',  ( 17.99999999999999645, 111.1352304691229733, -15.40237066878481720 ) ) ;
#36221 = EDGE_CURVE ( 'NONE', #26591, #14112, #22362, .T. ) ;
#36222 = CARTESIAN_POINT ( 'NONE',  ( 87.78546986788515483, 31.00000000000000000, 43.41392487578124104 ) ) ;
#36223 = ORIENTED_EDGE ( 'NONE', *, *, #28225, .F. ) ;
#36224 = DIRECTION ( 'NONE',  ( 0.000000000000000000, 0.000000000000000000, 1.000000000000000000 ) ) ;
#36225 = FACE_OUTER_BOUND ( 'NONE', #6130, .T. ) ;
#36226 = DIRECTION ( 'NONE',  ( 1.000000000000000000, 0.000000000000000000, 0.000000000000000000 ) ) ;
#36227 = VERTEX_POINT ( 'NONE', #38170 ) ;
#36228 = DIRECTION ( 'NONE',  ( 0.000000000000000000, 0.000000000000000000, 1.000000000000000000 ) ) ;
#36229 = CARTESIAN_POINT ( 'NONE',  ( 18.00000000000000355, 9.744342220503391161, 46.48873837489801275 ) ) ;
#36230 = AXIS2_PLACEMENT_3D ( 'NONE', #32504, #32083, #34919 ) ;
#36232 = LINE ( 'NONE', #26017, #20764 ) ;
#36231 = FACE_OUTER_BOUND ( 'NONE', #26807, .T. ) ;
#36233 = VECTOR ( 'NONE', #13472, 1000.000000000000000 ) ;
#36234 = CARTESIAN_POINT ( 'NONE',  ( 17.99999999999999645, -25.18647942089817349, 113.2326863338526977 ) ) ;
#36235 = ORIENTED_EDGE ( 'NONE', *, *, #17043, .F. ) ;
#36236 = CARTESIAN_POINT ( 'NONE',  ( 25.10416666396844576, 31.00000000000000355, 1.636246165087044124 ) ) ;
#36237 = AXIS2_PLACEMENT_3D ( 'NONE', #15664, #11307, #34850 ) ;
#36238 = EDGE_LOOP ( 'NONE', ( #337, #41234, #28570, #30159 ) ) ;
#36239 = DIRECTION ( 'NONE',  ( 0.000000000000000000, 0.9911528310040076395, -0.1327255272837190025 ) ) ;
#36240 = AXIS2_PLACEMENT_3D ( 'NONE', #38178, #11361, #30991 ) ;
#36241 = DIRECTION ( 'NONE',  ( -1.000000000000000000, 0.000000000000000000, 0.000000000000000000 ) ) ;
#36242 = EDGE_LOOP ( 'NONE', ( #15506, #16616, #25010, #39994 ) ) ;
#36243 = AXIS2_PLACEMENT_3D ( 'NONE', #35991, #22962, #29057 ) ;
#36244 = PLANE ( 'NONE',  #28553 ) ;
#36245 = CARTESIAN_POINT ( 'NONE',  ( 2.454369252093185239, 40.00000000000000000, 37.39583333513270702 ) ) ;
#36246 = CARTESIAN_POINT ( 'NONE',  ( 27.84166646521873645, 40.00000000000000000, -36.16032403486059366 ) ) ;
#36247 = ORIENTED_EDGE ( 'NONE', *, *, #980, .T. ) ;
#36248 = EDGE_LOOP ( 'NONE', ( #2779, #23784 ) ) ;
#36249 = DIRECTION ( 'NONE',  ( -1.000000000000000000, -0.000000000000000000, -0.000000000000000000 ) ) ;
#36250 = FACE_OUTER_BOUND ( 'NONE', #33555, .T. ) ;
#36251 = EDGE_CURVE ( 'NONE', #25329, #16, #6174, .T. ) ;
#36252 = CIRCLE ( 'NONE', #36289, 64.99999999999997158 ) ;
#36253 = CARTESIAN_POINT ( 'NONE',  ( 17.99999999999999645, 96.25468616236763353, -72.49500943364391503 ) ) ;
#36254 = CARTESIAN_POINT ( 'NONE',  ( 18.00000000000000355, -22.82995208772716467, 41.06517797613655318 ) ) ;
#36255 = DIRECTION ( 'NONE',  ( -1.000000000000000000, -0.000000000000000000, -0.000000000000000000 ) ) ;
#36256 = ORIENTED_EDGE ( 'NONE', *, *, #40266, .T. ) ;
#36257 = DIRECTION ( 'NONE',  ( 3.009274222672345096E-17, 1.000000000000000000, -2.455023325076454960E-18 ) ) ;
#36258 = ORIENTED_EDGE ( 'NONE', *, *, #8499, .F. ) ;
#36259 = DIRECTION ( 'NONE',  ( 0.000000000000000000, 0.000000000000000000, -1.000000000000000000 ) ) ;
#36260 = B_SPLINE_CURVE_WITH_KNOTS ( 'NONE', 3,
 ( #2660, #26898, #11190, #40172, #7232, #20827, #27331, #20375, #17757, #20592, #37772, #37564, #3951, #40821, #3719, #34502, #4170, #17104, #17335, #30610, #23860, #13604, #34289, #31030, #677, #14038, #24310, #34080, #30389, #27123, #16890, #7022, #23653, #1118, #14471, #893, #40598, #17541, #36913, #10310, #4385, #10974, #7675, #21040, #30172, #13829, #230, #10740, #37126, #33639, #27782, #33863, #24078, #466, #14244, #40391, #41038, #10524, #37343, #30816, #27549, #7889, #7462, #24521, #21252, #5051, #8328, #24732, #34939, #27996, #42105, #12054, #18410, #18200, #12264, #14688, #25169, #8534, #34732, #41701, #4839, #35148, #31469, #31673, #1772, #11621, #32105, #1555, #28840, #25371, #15545, #38628, #25591, #15125, #38417, #14902, #28204, #28429, #8112, #8754, #38849, #11841, #5267, #11399, #41254, #22109, #21893, #8972, #22318, #2184, #41472, #18634, #31897, #24963, #1983, #37989, #28633, #21479, #15341, #41905, #38212, #4612, #21686, #17988, #35368, #31257, #1339, #5485, #18843, #39902, #23171, #32522, #42331, #16179, #29476, #3019, #6530, #43181, #12481, #32306, #29695, #25994, #39252, #42966, #13338, #32731, #35993, #2388, #26421, #9178, #25793, #39478, #5896, #26634, #9384, #12898, #16630, #19892, #2815, #26206, #22740, #36208, #13128, #33165, #6118, #10029, #9616, #19469, #29061, #42740, #39053, #22530, #39685, #35765, #22964, #19253, #6330, #19676, #29268, #2612, #32943, #16389, #42536, #3249, #15974, #29921, #9819, #35570, #36417, #5689, #19044, #15755, #12685, #36865, #20539, #26845, #845, #4336, #7625, #24256, #30336, #33383, #40768, #23812, #30976, #40995, #20986, #17050, #3896, #10689, #3672, #37079, #16845, #4120, #13550, #40552, #627, #13773, #7413, #1064, #23604, #413, #34240, #17706, #30126, #23374, #27726, #10922, #20330, #183, #17280, #30564, #34033, #37518, #14417, #40121, #20123, #17488, #30769, #13983, #27282, #36638, #33809, #7182, #3467, #14198, #10254, #6970, #24026, #33592, #6762, #40341, #37293, #27072, #10472, #20772, #27495, #41420, #1719, #11140, #14640, #11570, #28798, #15074, #24913, #4557, #18363, #17935, #31206, #5214, #1293, #31623, #11350, #28382, #21641, #4795, #8058, #41651, #22059, #18152, #8286, #11800, #35320, #2141, #41202, #27947, #14853, #38164, #28152, #24681, #34890, #34451, #5438, #18581, #5007, #37938, #18803, #21199, #25126, #38371, #21428, #34678, #24468, #8489, #31420, #38579, #1504, #37722, #15503, #41860, #21854, #35100, #31851, #1936, #15302, #25327, #32057, #28590, #7840, #12010, #8701, #32476, #6281, #19846, #39211, #42493, #8929, #32900, #15707, #5643, #2768, #12436, #33110, #15927, #19425, #23127, #13083, #9339, #32691, #29224, #16131, #36167, #26380, #12639, #16580, #29433, #25952, #35525, #6073, #19006, #32262, #19630, #2341, #42697, #42283, #12850, #22693, #35726, #39007, #26158, #9775, #39433, #9570, #22921, #36376, #3199, #29015, #25755, #2568, #35944, #2976, #9131, #16340, #22278, #6487, #29645, #42924, #22485, #42060, #5852, #39647, #12219, #25542, #19208, #38800, #17228, #16793, #17002, #30288, #36816, #14153, #30079, #10865, #37243, #40718, #7357, #24203, #40293, #7138, #40064, #139, #36588, #30720, #796, #13938, #357, #30514, #6713, #39857, #4070, #13724, #37466, #4286, #27444, #23551, #10429, #586, #10202, #27026, #23332, #10643, #37030, #13502, #27232, #26796, #7579, #33341, #20938, #6925, #34190, #20077, #23762, #9982, #29878, #20716, #20493, #20281, #43142, #3425, #33759, #3841, #23977, #33545, #13290, #40504, #3630, #33982, #17444, #26587, #2451, #4505, #42395, #25653, #29122, #38911, #12538, #28103, #38111, #27895, #31154, #14802, #19105, #32367, #1667, #4740, #4955, #24420, #27675, #35631, #18102, #25853, #35832, #15815, #11299, #41366, #18310, #41150, #31367, #11092, #41597, #7791, #8236, #8007, #15021, #39119, #17877, #5747, #1012, #11517, #1242, #9240, #22589, #17660, #40945, #30926, #22381, #21594, #28328, #14362, #24631, #37673, #21151, #12328, #9028, #24857, #34840, #34400, #31575, #14589, #37884, #21372, #34622, #1449, #16902 ),
 .UNSPECIFIED., .F., .F.,
 ( 4, 2, 2, 2, 2, 2, 2, 2, 2, 2, 2, 2, 2, 2, 2, 2, 2, 2, 2, 2, 2, 2, 2, 2, 2, 2, 2, 2, 2, 2, 2, 2, 2, 2, 2, 2, 2, 2, 2, 2, 2, 2, 2, 2, 2, 2, 2, 2, 2, 2, 2, 2, 2, 2, 2, 2, 2, 2, 2, 2, 2, 2, 2, 2, 2, 2, 2, 2, 2, 2, 2, 2, 2, 2, 2, 2, 2, 2, 2, 2, 2, 2, 2, 2, 2, 2, 2, 2, 2, 2, 2, 2, 2, 2, 2, 2, 2, 2, 2, 2, 2, 2, 2, 2, 2, 2, 2, 2, 2, 2, 2, 2, 2, 2, 2, 2, 2, 2, 2, 2, 2, 2, 2, 2, 2, 2, 2, 2, 2, 2, 2, 2, 2, 2, 2, 2, 2, 2, 2, 2, 2, 2, 2, 2, 2, 2, 2, 2, 2, 2, 2, 2, 2, 2, 2, 2, 2, 2, 2, 2, 2, 2, 2, 2, 2, 2, 2, 2, 2, 2, 2, 2, 2, 2, 2, 2, 2, 2, 2, 2, 2, 2, 2, 2, 2, 2, 2, 2, 2, 2, 2, 2, 2, 2, 2, 2, 2, 2, 2, 2, 2, 2, 2, 2, 2, 2, 2, 2, 2, 2, 2, 2, 2, 2, 2, 2, 2, 2, 2, 2, 2, 2, 2, 2, 2, 2, 2, 2, 2, 2, 2, 2, 2, 2, 2, 2, 2, 2, 2, 2, 2, 2, 2, 2, 2, 2, 2, 2, 2, 2, 2, 2, 2, 2, 2, 2, 4 ),
 ( 0.000000000000000000, 0.003906250000000000000, 0.007812500000000000000, 0.01171875000000000000, 0.01562500000000000000, 0.01953125000000000000, 0.02343750000000000000, 0.02734375000000000000, 0.03125000000000000000, 0.03515625000000000000, 0.03906250000000000000, 0.04296875000000000000, 0.04687500000000000000, 0.05078125000000000000, 0.05468750000000000000, 0.05859375000000000000, 0.06250000000000000000, 0.06640625000000000000, 0.07031250000000000000, 0.07421875000000000000, 0.07812500000000000000, 0.08203125000000000000, 0.08593750000000000000, 0.08984375000000000000, 0.09375000000000000000, 0.09765625000000000000, 0.1015625000000000000, 0.1054687500000000000, 0.1093750000000000000, 0.1132812500000000000, 0.1171875000000000000, 0.1210937500000000000, 0.1250000000000000000, 0.1289062500000000000, 0.1328125000000000000, 0.1367187500000000000, 0.1406250000000000000, 0.1445312500000000000, 0.1484375000000000000, 0.1523437500000000000, 0.1562500000000000000, 0.1601562500000000000, 0.1640625000000000000, 0.1679687500000000000, 0.1718750000000000000, 0.1757812500000000000, 0.1796875000000000000, 0.1835937500000000000, 0.1875000000000000000, 0.1914062500000000000, 0.1953125000000000000, 0.1992187500000000000, 0.2031250000000000000, 0.2070312500000000000, 0.2109375000000000000, 0.2148437500000000000, 0.2187500000000000000, 0.2226562500000000000, 0.2265625000000000000, 0.2304687500000000000, 0.2343750000000000000, 0.2382812500000000000, 0.2421875000000000000, 0.2460937500000000000, 0.2500000000000000000, 0.2539062500000000000, 0.2578125000000000000, 0.2617187500000000000, 0.2656250000000000000, 0.2695312500000000000, 0.2734375000000000000, 0.2773437500000000000, 0.2812500000000000000, 0.2851562500000000000, 0.2890625000000000000, 0.2929687500000000000, 0.2968750000000000000, 0.3007812500000000000, 0.3046875000000000000, 0.3085937500000000000, 0.3125000000000000000, 0.3164062500000000000, 0.3203125000000000000, 0.3242187500000000000, 0.3281250000000000000, 0.3320312500000000000, 0.3359375000000000000, 0.3398437500000000000, 0.3437500000000000000, 0.3476562500000000000, 0.3515625000000000000, 0.3554687500000000000, 0.3593750000000000000, 0.3632812500000000000, 0.3671875000000000000, 0.3710937500000000000, 0.3750000000000000000, 0.3789062500000000000, 0.3828125000000000000, 0.3867187500000000000, 0.3906250000000000000, 0.3945312500000000000, 0.3984375000000000000, 0.4023437500000000000, 0.4062500000000000000, 0.4101562500000000000, 0.4140625000000000000, 0.4179687500000000000, 0.4218750000000000000, 0.4257812500000000000, 0.4296875000000000000, 0.4335937500000000000, 0.4375000000000000000, 0.4414062500000000000, 0.4453125000000000000, 0.4492187500000000000, 0.4531250000000000000, 0.4570312500000000000, 0.4609375000000000000, 0.4648437500000000000, 0.4687500000000000000, 0.4726562500000000000, 0.4765625000000000000, 0.4804687500000000000, 0.4843750000000000000, 0.4882812500000000000, 0.4921875000000000000, 0.4960937500000000000, 0.5000000000000000000, 0.5039062500000000000, 0.5078125000000000000, 0.5117187500000000000, 0.5156250000000000000, 0.5195312500000000000, 0.5234375000000000000, 0.5273437500000000000, 0.5312500000000000000, 0.5351562500000000000, 0.5390625000000000000, 0.5429687500000000000, 0.5468750000000000000, 0.5507812500000000000, 0.5546875000000000000, 0.5585937500000000000, 0.5625000000000000000, 0.5664062500000000000, 0.5703125000000000000, 0.5742187500000000000, 0.5781250000000000000, 0.5820312500000000000, 0.5859375000000000000, 0.5898437500000000000, 0.5937500000000000000, 0.5976562500000000000, 0.6015625000000000000, 0.6054687500000000000, 0.6093750000000000000, 0.6132812500000000000, 0.6171875000000000000, 0.6210937500000000000, 0.6250000000000000000, 0.6289062500000000000, 0.6328125000000000000, 0.6367187500000000000, 0.6406250000000000000, 0.6445312500000000000, 0.6484375000000000000, 0.6523437500000000000, 0.6562500000000000000, 0.6601562500000000000, 0.6640625000000000000, 0.6679687500000000000, 0.6718750000000000000, 0.6757812500000000000, 0.6796875000000000000, 0.6835937500000000000, 0.6875000000000000000, 0.6914062500000000000, 0.6953125000000000000, 0.6992187500000000000, 0.7031250000000000000, 0.7070312500000000000, 0.7109375000000000000, 0.7148437500000000000, 0.7187500000000000000, 0.7226562500000000000, 0.7265625000000000000, 0.7304687500000000000, 0.7343750000000000000, 0.7382812500000000000, 0.7421875000000000000, 0.7460937500000000000, 0.7500000000000000000, 0.7539062500000000000, 0.7578125000000000000, 0.7617187500000000000, 0.7656250000000000000, 0.7695312500000000000, 0.7734375000000000000, 0.7773437500000000000, 0.7812500000000000000, 0.7851562500000000000, 0.7890625000000000000, 0.7929687500000000000, 0.7968750000000000000, 0.8007812500000000000, 0.8046875000000000000, 0.8085937500000000000, 0.8125000000000000000, 0.8164062500000000000, 0.8203125000000000000, 0.8242187500000000000, 0.8281250000000000000, 0.8320312500000000000, 0.8359375000000000000, 0.8398437500000000000, 0.8437500000000000000, 0.8476562500000000000, 0.8515625000000000000, 0.8554687500000000000, 0.8593750000000000000, 0.8632812500000000000, 0.8671875000000000000, 0.8710937500000000000, 0.8750000000000000000, 0.8789062500000000000, 0.8828125000000000000, 0.8867187500000000000, 0.8906250000000000000, 0.8945312500000000000, 0.8984375000000000000, 0.9023437500000000000, 0.9062500000000000000, 0.9101562500000000000, 0.9140625000000000000, 0.9179687500000000000, 0.9218750000000000000, 0.9257812500000000000, 0.9296875000000000000, 0.9335937500000000000, 0.9375000000000000000, 0.9414062500000000000, 0.9453125000000000000, 0.9492187500000000000, 0.9531250000000000000, 0.9570312500000000000, 0.9609375000000000000, 0.9648437500000000000, 0.9687500000000000000, 0.9726562500000000000, 0.9765625000000000000, 0.9804687500000000000, 0.9843750000000000000, 0.9882812500000000000, 0.9921875000000000000, 0.9960937500000000000, 1.000000000000000000 ),
 .UNSPECIFIED. ) ;
#36261 = CARTESIAN_POINT ( 'NONE',  ( 0.000000000000000000, -29.36437154451922282, -116.8684075565139295 ) ) ;
#36262 = CIRCLE ( 'NONE', #11834, 58.99999999999998579 ) ;
#36263 = DIRECTION ( 'NONE',  ( 0.000000000000000000, 0.9957341762950341346, 0.09226835946330566585 ) ) ;
#36264 = CARTESIAN_POINT ( 'NONE',  ( 42.80287614962723808, -34.05525454449571754, 69.29271901957299917 ) ) ;
#36265 = ORIENTED_EDGE ( 'NONE', *, *, #11920, .T. ) ;
#36266 = FACE_BOUND ( 'NONE', #25076, .T. ) ;
#36267 = ORIENTED_EDGE ( 'NONE', *, *, #18002, .T. ) ;
#36268 = VECTOR ( 'NONE', #25248, 1000.000000000000000 ) ;
#36269 = CARTESIAN_POINT ( 'NONE',  ( -24.74979319748359785, 5.944745455504278020, 2.972870684497277427 ) ) ;
#36270 = EDGE_CURVE ( 'NONE', #38197, #17094, #15292, .T. ) ;
#36271 = AXIS2_PLACEMENT_3D ( 'NONE', #5602, #1674, #8657 ) ;
#36272 = ORIENTED_EDGE ( 'NONE', *, *, #10735, .F. ) ;
#36274 = ORIENTED_EDGE ( 'NONE', *, *, #23633, .T. ) ;
#36273 = CARTESIAN_POINT ( 'NONE',  ( 9.000000000000001776, -58.30069736313598128, -100.2847380560572930 ) ) ;
#36275 = CIRCLE ( 'NONE', #8420, 58.99999999999999289 ) ;
#36276 = EDGE_CURVE ( 'NONE', #18324, #21496, #26384, .T. ) ;
#36277 = CARTESIAN_POINT ( 'NONE',  ( -16.51797447735581059, 31.00000000000000355, -62.05742538355529803 ) ) ;
#36278 = ORIENTED_EDGE ( 'NONE', *, *, #32005, .F. ) ;
#36279 = FACE_OUTER_BOUND ( 'NONE', #27671, .T. ) ;
#36280 = AXIS2_PLACEMENT_3D ( 'NONE', #27442, #30719, #4069 ) ;
#36281 =( BOUNDED_SURFACE ( )  B_SPLINE_SURFACE ( 3, 2, ( 
 ( #10996, #1357, #38004 ),
 ( #21497, #4856, #37366 ),
 ( #20844, #1572, #28223 ),
 ( #15147, #28448, #14263 ),
 ( #35584, #5704, #22546 ),
 ( #19483, #18653, #8552 ) ),
 .UNSPECIFIED., .F., .F., .F. ) 
 B_SPLINE_SURFACE_WITH_KNOTS ( ( 4, 2, 4 ),
 ( 3, 3 ),
 ( 0.02027752710269158445, 0.02273781595091097299, 0.02519810479913036153 ),
 ( 0.000000000000000000, 1.000000000000000000 ),
 .UNSPECIFIED. ) 
 GEOMETRIC_REPRESENTATION_ITEM ( )  RATIONAL_B_SPLINE_SURFACE ( (
 ( 1.000000000000000000, 0.8047781431712808242, 1.000000000000000000),
 ( 1.000000000000000000, 0.8123773247083928561, 1.000000000000000000),
 ( 1.000000000000000000, 0.8190670192154906326, 1.000000000000000000),
 ( 1.000000000000000000, 0.8192353552912178261, 1.000000000000000000),
 ( 1.000000000000000000, 0.8126132098226825917, 1.000000000000000000),
 ( 1.000000000000000000, 0.8047712465856394770, 1.000000000000000000) ) ) 
 REPRESENTATION_ITEM ( '' )  SURFACE ( )  );
#36282 = VERTEX_POINT ( 'NONE', #14645 ) ;
#36283 = FACE_OUTER_BOUND ( 'NONE', #24379, .T. ) ;
#36284 = VERTEX_POINT ( 'NONE', #4799 ) ;
#36285 = CARTESIAN_POINT ( 'NONE',  ( 82.09539989320980169, 39.99999999999999289, -27.75477508813643723 ) ) ;
#36286 = AXIS2_PLACEMENT_3D ( 'NONE', #35543, #18603, #31870 ) ;
#36288 = DIRECTION ( 'NONE',  ( 1.000000000000000000, 0.000000000000000000, 0.000000000000000000 ) ) ;
#36287 = FACE_OUTER_BOUND ( 'NONE', #20170, .T. ) ;
#36289 = AXIS2_PLACEMENT_3D ( 'NONE', #43003, #26886, #36453 ) ;
#36290 = DIRECTION ( 'NONE',  ( 0.2140725878556618555, -0.9768177553304301375, -2.795573601670286284E-15 ) ) ;
#36291 = ORIENTED_EDGE ( 'NONE', *, *, #37350, .F. ) ;
#36292 = DIRECTION ( 'NONE',  ( -1.000000000000000000, 0.000000000000000000, -0.000000000000000000 ) ) ;
#36293 = ORIENTED_EDGE ( 'NONE', *, *, #31646, .T. ) ;
#36294 =( LENGTH_UNIT ( ) NAMED_UNIT ( * ) SI_UNIT ( .MILLI., .METRE. ) );
#36295 = ADVANCED_FACE ( 'NONE', ( #24476 ), #18156, .T. ) ;
#36296 = DIRECTION ( 'NONE',  ( 1.000000000000000000, 0.000000000000000000, 0.000000000000000000 ) ) ;
#36297 = CARTESIAN_POINT ( 'NONE',  ( 0.000000000000000000, 30.03615769709734451, 42.44795908868999135 ) ) ;
#36298 = CARTESIAN_POINT ( 'NONE',  ( -40.93297376624923345, 31.00000000000000355, -70.86912620794510076 ) ) ;
#36300 = CYLINDRICAL_SURFACE ( 'NONE', #22994, 31.49899999999999878 ) ;
#36299 = CARTESIAN_POINT ( 'NONE',  ( 17.99999999999999645, -47.58001226230612701, 110.7096808509482031 ) ) ;
#36301 = ORIENTED_EDGE ( 'NONE', *, *, #38986, .F. ) ;
#36302 = VECTOR ( 'NONE', #16262, 1000.000000000000000 ) ;
#36303 = AXIS2_PLACEMENT_3D ( 'NONE', #40251, #23721, #36984 ) ;
#36304 = CIRCLE ( 'NONE', #32157, 36.00000000000000000 ) ;
#36305 = ORIENTED_EDGE ( 'NONE', *, *, #35277, .T. ) ;
#36306 = DIRECTION ( 'NONE',  ( 0.000000000000000000, 0.000000000000000000, -1.000000000000000000 ) ) ;
#36307 = CARTESIAN_POINT ( 'NONE',  ( 17.99999999999999645, 2.418575551222434949, -120.4767259403368911 ) ) ;
#36308 = CARTESIAN_POINT ( 'NONE',  ( -41.44813913998980581, 31.00000000000000355, -84.33308812960441969 ) ) ;
#36309 = AXIS2_PLACEMENT_3D ( 'NONE', #2926, #39373, #16288 ) ;
#36310 = CARTESIAN_POINT ( 'NONE',  ( 17.99999999999999645, 0.000000000000000000, 0.000000000000000000 ) ) ;
#36311 = LINE ( 'NONE', #19780, #10245 ) ;
#36312 = VERTEX_POINT ( 'NONE', #37728 ) ;
#36313 = CARTESIAN_POINT ( 'NONE',  ( 9.000000000000001776, -114.8812324315176312, 16.07179003769107339 ) ) ;
#36314 = ORIENTED_EDGE ( 'NONE', *, *, #13535, .T. ) ;
#36315 = AXIS2_PLACEMENT_3D ( 'NONE', #8028, #21397, #22191 ) ;
#36316 = LINE ( 'NONE', #2711, #20069 ) ;
#36317 = DIRECTION ( 'NONE',  ( 1.000000000000000000, 0.000000000000000000, 0.000000000000000000 ) ) ;
#36318 = CARTESIAN_POINT ( 'NONE',  ( 0.000000000000000000, -0.6819280456820884240, -115.9979955608738607 ) ) ;
#36319 = VERTEX_POINT ( 'NONE', #14858 ) ;
#36320 = CARTESIAN_POINT ( 'NONE',  ( -10.00000000000000000, 0.000000000000000000, 0.000000000000000000 ) ) ;
#36321 = DIRECTION ( 'NONE',  ( 0.000000000000000000, 0.000000000000000000, 1.000000000000000000 ) ) ;
#36322 = ADVANCED_FACE ( 'NONE', ( #11575, #40558 ), #41208, .T. ) ;
#36323 = CARTESIAN_POINT ( 'NONE',  ( 0.000000000000000000, 0.000000000000000000, -0.3080913168122742518 ) ) ;
#36325 = ORIENTED_EDGE ( 'NONE', *, *, #5858, .T. ) ;
#36324 = FACE_OUTER_BOUND ( 'NONE', #14207, .T. ) ;
#36326 = ADVANCED_FACE ( 'NONE', ( #21204 ), #28156, .F. ) ;
#36327 = CARTESIAN_POINT ( 'NONE',  ( 37.09854380387523776, 31.00000000000000355, 2.490183985263670685 ) ) ;
#36328 = DIRECTION ( 'NONE',  ( 0.000000000000000000, 0.5963673585384969833, 0.8027116379309670036 ) ) ;
#36330 = ORIENTED_EDGE ( 'NONE', *, *, #10628, .F. ) ;
#36329 = CARTESIAN_POINT ( 'NONE',  ( 0.000000000000000000, -115.0622509503833442, 14.72000021165104755 ) ) ;
#36331 = ORIENTED_EDGE ( 'NONE', *, *, #28347, .T. ) ;
#36332 = DIRECTION ( 'NONE',  ( 0.000000000000000000, 0.000000000000000000, 1.000000000000000000 ) ) ;
#36333 = AXIS2_PLACEMENT_3D ( 'NONE', #32752, #2632, #5509 ) ;
#36334 = CARTESIAN_POINT ( 'NONE',  ( 0.000000000000000000, -6.109652351741465814, -46.58570277113515345 ) ) ;
#36335 = CARTESIAN_POINT ( 'NONE',  ( 44.54779904932823342, 40.00000000000000000, -34.05916983163054113 ) ) ;
#36336 = DIRECTION ( 'NONE',  ( -1.000000000000000000, 0.000000000000000000, 0.000000000000000000 ) ) ;
#36337 = CIRCLE ( 'NONE', #34953, 58.99999999999999289 ) ;
#36338 = CARTESIAN_POINT ( 'NONE',  ( -12.69999999999999929, 0.000000000000000000, 0.000000000000000000 ) ) ;
#36339 = VECTOR ( 'NONE', #2821, 1000.000000000000000 ) ;
#36340 = DIRECTION ( 'NONE',  ( 1.000000000000000000, -1.373900992973641277E-15, -5.551115123125812284E-16 ) ) ;
#36341 = ORIENTED_EDGE ( 'NONE', *, *, #11865, .F. ) ;
#36342 = LINE ( 'NONE', #2531, #5611 ) ;
#36343 = VERTEX_POINT ( 'NONE', #17940 ) ;
#36344 = ADVANCED_FACE ( 'NONE', ( #20995 ), #1298, .T. ) ;
#36345 = AXIS2_PLACEMENT_3D ( 'NONE', #17309, #20352, #40793 ) ;
#36346 = DIRECTION ( 'NONE',  ( 1.000000000000000000, 0.000000000000000000, 0.000000000000000000 ) ) ;
#36347 = CARTESIAN_POINT ( 'NONE',  ( 17.99999999999999645, 14.84191762912354839, -27.78316904333109960 ) ) ;
#36349 = EDGE_CURVE ( 'NONE', #31530, #27814, #27799, .T. ) ;
#36348 = CARTESIAN_POINT ( 'NONE',  ( -47.99616210117395099, 31.00000000000000355, 12.86278070621785119 ) ) ;
#36350 = DIRECTION ( 'NONE',  ( -1.000000000000000000, -0.000000000000000000, -0.000000000000000000 ) ) ;
#36351 = ORIENTED_EDGE ( 'NONE', *, *, #35966, .T. ) ;
#36352 = PRODUCT_DEFINITION_SHAPE ( 'NONE', 'NONE',  #43202 ) ;
#36353 = CARTESIAN_POINT ( 'NONE',  ( 18.00000000000000355, -11.90021268425586953, 45.45261810511210143 ) ) ;
#36354 = VERTEX_POINT ( 'NONE', #20545 ) ;
#36355 = CARTESIAN_POINT ( 'NONE',  ( -85.90019077458921970, 31.00000000000000711, -29.16093118951848240 ) ) ;
#36356 = EDGE_CURVE ( 'NONE', #12270, #4861, #20147, .T. ) ;
#36357 = CYLINDRICAL_SURFACE ( 'NONE', #41494, 20.00000000000000355 ) ;
#36358 = ORIENTED_EDGE ( 'NONE', *, *, #7350, .F. ) ;
#36359 = CARTESIAN_POINT ( 'NONE',  ( -50.06114249714176623, 31.00000000000000355, -38.53249520213265811 ) ) ;
#36360 = CARTESIAN_POINT ( 'NONE',  ( -41.78821403078462282, 40.00000000000000000, -47.79414628086202299 ) ) ;
#36361 = CARTESIAN_POINT ( 'NONE',  ( -49.27414759474276451, 40.00000000000000711, 85.34056160678568403 ) ) ;
#36362 = ADVANCED_FACE ( 'NONE', ( #13991 ), #7418, .T. ) ;
#36363 = ORIENTED_EDGE ( 'NONE', *, *, #31600, .T. ) ;
#36364 = ORIENTED_EDGE ( 'NONE', *, *, #39763, .T. ) ;
#36365 = FILL_AREA_STYLE_COLOUR ( '', #37367 ) ;
#36366 = AXIS2_PLACEMENT_3D ( 'NONE', #13173, #26680, #9437 ) ;
#36367 = CARTESIAN_POINT ( 'NONE',  ( 18.00000000000000355, 12.30077720129167318, -50.52416135122068397 ) ) ;
#36368 = CARTESIAN_POINT ( 'NONE',  ( 0.000000000000000000, -95.31344542257777164, 66.11616384574416827 ) ) ;
#36369 = AXIS2_PLACEMENT_3D ( 'NONE', #34455, #1069, #10478 ) ;
#36371 = VERTEX_POINT ( 'NONE', #40775 ) ;
#36370 = CARTESIAN_POINT ( 'NONE',  ( 4.101954839143060028, 2.368264730582927857, -3.681130640444267854 ) ) ;
#36372 = CARTESIAN_POINT ( 'NONE',  ( 0.000000000000000000, -100.8494052988166345, -65.95368414179012007 ) ) ;
#36373 = ORIENTED_EDGE ( 'NONE', *, *, #19420, .F. ) ;
#36374 = DIRECTION ( 'NONE',  ( 0.000000000000000000, 0.000000000000000000, -1.000000000000000000 ) ) ;
#36375 = EDGE_CURVE ( 'NONE', #22361, #710, #10927, .T. ) ;
#36376 = CARTESIAN_POINT ( 'NONE',  ( 34.02738612458995959, 40.00000000000000000, 69.00154638599002510 ) ) ;
#36377 = CARTESIAN_POINT ( 'NONE',  ( 18.00000000000000355, -45.78515115856033901, -12.64416602183713856 ) ) ;
#36378 = AXIS2_PLACEMENT_3D ( 'NONE', #27756, #7649, #41882 ) ;
#36379 = VERTEX_POINT ( 'NONE', #38378 ) ;
#36380 = CYLINDRICAL_SURFACE ( 'NONE', #9469, 31.49899999999999878 ) ;
#36381 = EDGE_CURVE ( 'NONE', #1564, #5006, #29595, .T. ) ;
#36382 = CARTESIAN_POINT ( 'NONE',  ( 18.00000000000000355, 0.000000000000000000, 0.000000000000000000 ) ) ;
#36383 = ORIENTED_EDGE ( 'NONE', *, *, #35205, .T. ) ;
#36384 = ORIENTED_EDGE ( 'NONE', *, *, #33042, .F. ) ;
#36385 = CARTESIAN_POINT ( 'NONE',  ( 0.000000000000000000, -0.6505223195679212811, -51.99593080916758936 ) ) ;
#36386 = ORIENTED_EDGE ( 'NONE', *, *, #42848, .F. ) ;
#36387 = DIRECTION ( 'NONE',  ( 0.000000000000000000, -0.9968120070307509017, 0.07978610555307336094 ) ) ;
#36388 = DIRECTION ( 'NONE',  ( -3.009274222672345096E-17, -1.000000000000000000, 2.455023325076454960E-18 ) ) ;
#36389 = DIRECTION ( 'NONE',  ( 1.000000000000000000, 0.000000000000000000, 0.000000000000000000 ) ) ;
#36390 = CARTESIAN_POINT ( 'NONE',  ( 9.000000000000001776, -5.492704054965900973, -115.8698847939556771 ) ) ;
#36391 = ORIENTED_EDGE ( 'NONE', *, *, #43102, .F. ) ;
#36392 = CARTESIAN_POINT ( 'NONE',  ( 17.99999999999999645, 0.000000000000000000, 0.000000000000000000 ) ) ;
#36393 = ORIENTED_EDGE ( 'NONE', *, *, #27625, .F. ) ;
#36394 = AXIS2_PLACEMENT_3D ( 'NONE', #14826, #37697, #24886 ) ;
#36395 = LINE ( 'NONE', #8950, #23858 ) ;
#36396 = EDGE_CURVE ( 'NONE', #18124, #35448, #39581, .T. ) ;
#36398 = EDGE_CURVE ( 'NONE', #42546, #36284, #22870, .T. ) ;
#36397 = CARTESIAN_POINT ( 'NONE',  ( -10.86393331615775892, 31.00000000000000355, -18.79923026442779843 ) ) ;
#36399 = EDGE_LOOP ( 'NONE', ( #35704, #34822, #6874, #22143 ) ) ;
#36400 = DIRECTION ( 'NONE',  ( -1.000000000000000000, 0.000000000000000000, -0.000000000000000000 ) ) ;
#36401 = EDGE_CURVE ( 'NONE', #2262, #28933, #18767, .T. ) ;
#36402 = EDGE_CURVE ( 'NONE', #7888, #31916, #40297, .T. ) ;
#36403 = AXIS2_PLACEMENT_3D ( 'NONE', #34196, #362, #20082 ) ;
#36404 = DIRECTION ( 'NONE',  ( 0.000000000000000000, 0.000000000000000000, 1.000000000000000000 ) ) ;
#36405 = APPLICATION_PROTOCOL_DEFINITION ( 'draft international standard', 'automotive_design', 1998, #10016 ) ;
#36406 = FACE_OUTER_BOUND ( 'NONE', #26430, .T. ) ;
#36407 = CARTESIAN_POINT ( 'NONE',  ( -44.33513214241411760, 31.00000000000000355, 38.89722855811361768 ) ) ;
#36408 = ORIENTED_EDGE ( 'NONE', *, *, #27058, .T. ) ;
#36409 = CARTESIAN_POINT ( 'NONE',  ( -12.95950413119362743, 31.00000000000000355, 37.95406330259781669 ) ) ;
#36410 = CARTESIAN_POINT ( 'NONE',  ( 64.37268382102905662, 39.99999999999999289, -8.487791176987355968 ) ) ;
#36411 = DIRECTION ( 'NONE',  ( -1.000000000000000000, 0.000000000000000000, -0.000000000000000000 ) ) ;
#36412 = FACE_OUTER_BOUND ( 'NONE', #3837, .T. ) ;
#36413 = FACE_OUTER_BOUND ( 'NONE', #24988, .T. ) ;
#36414 = ADVANCED_FACE ( 'NONE', ( #36324 ), #26534, .T. ) ;
#36415 = CIRCLE ( 'NONE', #6467, 59.00000000000000000 ) ;
#36416 = ORIENTED_EDGE ( 'NONE', *, *, #5542, .T. ) ;
#36417 = CARTESIAN_POINT ( 'NONE',  ( -44.28363997456384737, 40.00000000000000000, 21.84072794957603492 ) ) ;
#36418 = FACE_OUTER_BOUND ( 'NONE', #22181, .T. ) ;
#36419 = CARTESIAN_POINT ( 'NONE',  ( 4.000000000000000000, 0.3987449864460005378, -0.01220643443059817035 ) ) ;
#36420 = ORIENTED_EDGE ( 'NONE', *, *, #29979, .T. ) ;
#36421 = EDGE_CURVE ( 'NONE', #22420, #26402, #29882, .T. ) ;
#36422 = CYLINDRICAL_SURFACE ( 'NONE', #29399, 13.59999999999999787 ) ;
#36423 = DIRECTION ( 'NONE',  ( -1.000000000000000000, 0.000000000000000000, 0.000000000000000000 ) ) ;
#36424 = ORIENTED_EDGE ( 'NONE', *, *, #29362, .F. ) ;
#36425 = CARTESIAN_POINT ( 'NONE',  ( -4.000000000000000000, -2.309401076758512694, -5.000000000000000000 ) ) ;
#36426 = ORIENTED_EDGE ( 'NONE', *, *, #19349, .T. ) ;
#36427 = CIRCLE ( 'NONE', #21896, 58.99999999999998579 ) ;
#36428 = ORIENTED_EDGE ( 'NONE', *, *, #32316, .F. ) ;
#36429 = DIRECTION ( 'NONE',  ( 0.000000000000000000, 0.000000000000000000, 1.000000000000000000 ) ) ;
#36430 = CARTESIAN_POINT ( 'NONE',  ( -91.90012763196533285, 31.00000000000000711, 5.898218105444796855 ) ) ;
#36431 = EDGE_LOOP ( 'NONE', ( #30780, #20562, #32777, #12193 ) ) ;
#36432 = DIRECTION ( 'NONE',  ( 0.000000000000000000, -0.9714298932647074114, -0.2373266998711250908 ) ) ;
#36433 = CARTESIAN_POINT ( 'NONE',  ( 0.000000000000000000, -20.99948489194393275, -42.60488980472802467 ) ) ;
#36434 = CARTESIAN_POINT ( 'NONE',  ( 0.000000000000000000, -114.1157422997281969, -20.82300072953048442 ) ) ;
#36435 = VERTEX_POINT ( 'NONE', #26331 ) ;
#36436 = CARTESIAN_POINT ( 'NONE',  ( 0.000000000000000000, -109.1131968883996848, -26.12628443612003437 ) ) ;
#36437 = CARTESIAN_POINT ( 'NONE',  ( 6.199999999999993960, 18.77999999999999758, 0.000000000000000000 ) ) ;
#36438 = ADVANCED_FACE ( 'NONE', ( #39599 ), #8494, .F. ) ;
#36439 = ADVANCED_FACE ( 'NONE', ( #21858 ), #34897, .F. ) ;
#36441 = CARTESIAN_POINT ( 'NONE',  ( 17.99999999999999645, 34.03109950475885626, -115.5957406979046596 ) ) ;
#36440 = DIRECTION ( 'NONE',  ( -1.836909530733573776E-16, 1.000000000000000000, 0.000000000000000000 ) ) ;
#36442 = ADVANCED_FACE ( 'NONE', ( #29385 ), #16521, .T. ) ;
#36443 = EDGE_CURVE ( 'NONE', #28496, #41098, #31272, .T. ) ;
#36444 = VECTOR ( 'NONE', #34271, 1000.000000000000000 ) ;
#36445 = CYLINDRICAL_SURFACE ( 'NONE', #31899, 59.00000000000000000 ) ;
#36446 = ORIENTED_EDGE ( 'NONE', *, *, #28032, .F. ) ;
#36447 =( LENGTH_UNIT ( ) NAMED_UNIT ( * ) SI_UNIT ( .MILLI., .METRE. ) );
#36448 = ADVANCED_FACE ( 'NONE', ( #6235 ), #22064, .F. ) ;
#36449 = AXIS2_PLACEMENT_3D ( 'NONE', #40117, #23599, #40548 ) ;
#36450 = CARTESIAN_POINT ( 'NONE',  ( 30.80114556864472775, 31.00000000000000355, -15.19345985420777190 ) ) ;
#36451 = ORIENTED_EDGE ( 'NONE', *, *, #31650, .F. ) ;
#36452 = CARTESIAN_POINT ( 'NONE',  ( 9.000000000000001776, -7.162210897275388177, -51.50439529848834042 ) ) ;
#36453 = DIRECTION ( 'NONE',  ( -1.000000000000000000, 3.336006684570784581E-17, 0.000000000000000000 ) ) ;
#36454 = ORIENTED_EDGE ( 'NONE', *, *, #23962, .T. ) ;
#36455 = ADVANCED_FACE ( 'NONE', ( #43090 ), #13239, .T. ) ;
#36456 = CARTESIAN_POINT ( 'NONE',  ( -10.00000000000000000, 0.000000000000000000, 0.000000000000000000 ) ) ;
#36457 = CARTESIAN_POINT ( 'NONE',  ( -13.53264355869793967, 40.00000000000000000, -39.83251807627727459 ) ) ;
#36458 = CARTESIAN_POINT ( 'NONE',  ( -51.89982240185989326, 40.00000000000000000, 3.308651922604956219 ) ) ;
#36459 = VERTEX_POINT ( 'NONE', #5012 ) ;
#36460 = ORIENTED_EDGE ( 'NONE', *, *, #1853, .T. ) ;
#36461 = DIRECTION ( 'NONE',  ( 0.000000000000000000, 0.000000000000000000, 1.000000000000000000 ) ) ;
#36462 = DIRECTION ( 'NONE',  ( -1.000000000000000000, -0.000000000000000000, -0.000000000000000000 ) ) ;
#36463 = DIRECTION ( 'NONE',  ( -1.000000000000000000, 1.084202172485505174E-16, 0.000000000000000000 ) ) ;
#36464 = CIRCLE ( 'NONE', #227, 58.99999999999998579 ) ;
#36465 = DIRECTION ( 'NONE',  ( 1.000000000000000000, 0.000000000000000000, -0.000000000000000000 ) ) ;
#36466 = DIRECTION ( 'NONE',  ( 1.000000000000000000, 0.000000000000000000, 0.000000000000000000 ) ) ;
#36467 = ORIENTED_EDGE ( 'NONE', *, *, #32961, .T. ) ;
#36468 = CARTESIAN_POINT ( 'NONE',  ( 18.00000000000000355, 0.000000000000000000, 0.000000000000000000 ) ) ;
#36469 = ORIENTED_EDGE ( 'NONE', *, *, #25310, .F. ) ;
#36470 = DIRECTION ( 'NONE',  ( -1.000000000000000000, -0.000000000000000000, 0.000000000000000000 ) ) ;
#36471 = DIRECTION ( 'NONE',  ( -1.000000000000000000, 0.000000000000000000, -0.000000000000000000 ) ) ;
#36472 = VERTEX_POINT ( 'NONE', #18367 ) ;
#36473 = DIRECTION ( 'NONE',  ( -1.000000000000000000, 0.000000000000000000, 0.000000000000000000 ) ) ;
#36474 = CIRCLE ( 'NONE', #28178, 59.00000000000000711 ) ;
#36475 = CARTESIAN_POINT ( 'NONE',  ( 17.99999999999999645, 29.02167576844250618, -108.3790330702166926 ) ) ;
#36476 = ORIENTED_EDGE ( 'NONE', *, *, #36643, .F. ) ;
#36477 = DIRECTION ( 'NONE',  ( -1.000000000000000000, -0.000000000000000000, -0.000000000000000000 ) ) ;
#36478 = VERTEX_POINT ( 'NONE', #25130 ) ;
#36479 = EDGE_CURVE ( 'NONE', #25511, #27790, #35104, .T. ) ;
#36480 = DIRECTION ( 'NONE',  ( 0.000000000000000000, 0.000000000000000000, 1.000000000000000000 ) ) ;
#36481 = AXIS2_PLACEMENT_3D ( 'NONE', #34886, #1933, #37719 ) ;
#36482 = ORIENTED_EDGE ( 'NONE', *, *, #6960, .T. ) ;
#36484 = ORIENTED_EDGE ( 'NONE', *, *, #16437, .F. ) ;
#36483 = FACE_OUTER_BOUND ( 'NONE', #6835, .T. ) ;
#36485 = CARTESIAN_POINT ( 'NONE',  ( -15.62887661520211857, 31.00000000000000355, 57.97203279869351888 ) ) ;
#36486 = VERTEX_POINT ( 'NONE', #38583 ) ;
#36487 = DIRECTION ( 'NONE',  ( 0.000000000000000000, 0.000000000000000000, 1.000000000000000000 ) ) ;
#36488 = PRODUCT_DEFINITION_FORMATION_WITH_SPECIFIED_SOURCE ( 'ANY', '', #9892, .NOT_KNOWN. ) ;
#36489 = ORIENTED_EDGE ( 'NONE', *, *, #7961, .F. ) ;
#36490 = FACE_OUTER_BOUND ( 'NONE', #14266, .T. ) ;
#36491 = ORIENTED_EDGE ( 'NONE', *, *, #3820, .T. ) ;
#36493 = CARTESIAN_POINT ( 'NONE',  ( 64.75392801420538547, 39.99999999999999289, -56.64582372546511380 ) ) ;
#36492 = CIRCLE ( 'NONE', #39285, 10.99999999999999645 ) ;
#36495 = DIRECTION ( 'NONE',  ( 0.000000000000000000, -0.3681245526846654847, -0.9297764858882564543 ) ) ;
#36494 = CARTESIAN_POINT ( 'NONE',  ( 9.000000000000001776, -46.77034588191288123, -22.72740077717278595 ) ) ;
#36496 = EDGE_CURVE ( 'NONE', #27343, #14260, #36156, .T. ) ;
#36497 = EDGE_CURVE ( 'NONE', #16254, #36354, #23923, .T. ) ;
#36498 = LINE ( 'NONE', #13417, #21378 ) ;
#36499 = EDGE_LOOP ( 'NONE', ( #15437, #5678, #24688, #11146 ) ) ;
#36500 = CARTESIAN_POINT ( 'NONE',  ( 0.000000000000000000, 0.000000000000000000, 0.000000000000000000 ) ) ;
#36501 = ORIENTED_EDGE ( 'NONE', *, *, #19034, .F. ) ;
#36502 = EDGE_CURVE ( 'NONE', #3853, #38171, #11820, .T. ) ;
#36503 = VECTOR ( 'NONE', #39663, 1000.000000000000000 ) ;
#36504 = AXIS2_PLACEMENT_3D ( 'NONE', #12150, #15860, #32629 ) ;
#36505 = CARTESIAN_POINT ( 'NONE',  ( 18.00000000000000355, -41.20225022064653331, 23.63323037071389621 ) ) ;
#36506 = CARTESIAN_POINT ( 'NONE',  ( 38.42722039544141666, 31.00000000000000355, 66.52996821281629991 ) ) ;
#36508 = FACE_OUTER_BOUND ( 'NONE', #3653, .T. ) ;
#36507 = CYLINDRICAL_SURFACE ( 'NONE', #10004, 116.0000000000000000 ) ;
#36509 = VERTEX_POINT ( 'NONE', #26746 ) ;
#36510 = VECTOR ( 'NONE', #3817, 1000.000000000000000 ) ;
#36511 = ADVANCED_FACE ( 'NONE', ( #30671 ), #20441, .F. ) ;
#36512 = DIRECTION ( 'NONE',  ( 0.000000000000000000, 0.000000000000000000, -1.000000000000000000 ) ) ;
#36513 = AXIS2_PLACEMENT_3D ( 'NONE', #4283, #18307, #10862 ) ;
#36514 = EDGE_CURVE ( 'NONE', #3796, #27725, #6206, .T. ) ;
#36515 = ORIENTED_EDGE ( 'NONE', *, *, #7103, .F. ) ;
#36516 = DIRECTION ( 'NONE',  ( 0.000000000000000000, -0.1062934856473523731, -0.9943348002101385363 ) ) ;
#36517 = DIRECTION ( 'NONE',  ( 0.000000000000000000, 0.3681245526846719240, 0.9297764858882537897 ) ) ;
#36518 = CYLINDRICAL_SURFACE ( 'NONE', #6543, 120.5010000000000190 ) ;
#36519 = CYLINDRICAL_SURFACE ( 'NONE', #378, 13.60000000000000142 ) ;
#36520 = ORIENTED_EDGE ( 'NONE', *, *, #26578, .T. ) ;
#36521 = DIRECTION ( 'NONE',  ( 0.000000000000000000, 0.000000000000000000, 1.000000000000000000 ) ) ;
#36522 = ORIENTED_EDGE ( 'NONE', *, *, #14633, .T. ) ;
#36523 = CARTESIAN_POINT ( 'NONE',  ( 18.00000000000000355, 0.000000000000000000, 0.000000000000000000 ) ) ;
#36524 = DIRECTION ( 'NONE',  ( -1.000000000000000000, -0.000000000000000000, -0.000000000000000000 ) ) ;
#36525 = CARTESIAN_POINT ( 'NONE',  ( 8.999999999999998224, 112.5220807139884016, 28.19186676675879255 ) ) ;
#36526 = EDGE_LOOP ( 'NONE', ( #30243, #292, #29297, #1272 ) ) ;
#36527 = ADVANCED_FACE ( 'NONE', ( #7532 ), #3788, .T. ) ;
#36528 = VERTEX_POINT ( 'NONE', #4240 ) ;
#36529 = LINE ( 'NONE', #43087, #13333 ) ;
#36530 = CIRCLE ( 'NONE', #14976, 52.00000000000000000 ) ;
#36531 = CARTESIAN_POINT ( 'NONE',  ( 2.500000000000000000, 1.178949249685212974, -2.042000000000001148 ) ) ;
#36532 = FACE_OUTER_BOUND ( 'NONE', #59, .T. ) ;
#36533 = AXIS2_PLACEMENT_3D ( 'NONE', #30968, #1284, #20766 ) ;
#36535 = VERTEX_POINT ( 'NONE', #36763 ) ;
#36534 = DIRECTION ( 'NONE',  ( 1.000000000000000000, 0.000000000000000000, 0.000000000000000000 ) ) ;
#36536 = CARTESIAN_POINT ( 'NONE',  ( 7.507699080471219588, 31.00000000000000355, 28.16210111025598195 ) ) ;
#36537 = DIRECTION ( 'NONE',  ( 0.000000000000000000, 0.000000000000000000, 1.000000000000000000 ) ) ;
#36538 = CIRCLE ( 'NONE', #16398, 120.5010000000000190 ) ;
#36540 = ORIENTED_EDGE ( 'NONE', *, *, #24339, .T. ) ;
#36539 = CARTESIAN_POINT ( 'NONE',  ( 17.99999999999999645, -18.25486108452643208, 25.66996392254267079 ) ) ;
#36541 = AXIS2_PLACEMENT_3D ( 'NONE', #25482, #39371, #36113 ) ;
#36542 = ORIENTED_EDGE ( 'NONE', *, *, #14758, .F. ) ;
#36543 = LINE ( 'NONE', #9088, #20551 ) ;
#36544 = DIRECTION ( 'NONE',  ( -1.000000000000000000, 0.000000000000000000, 0.000000000000000000 ) ) ;
#36545 = CARTESIAN_POINT ( 'NONE',  ( 27.80911911934546055, 40.00000000000000000, -47.97225535894359894 ) ) ;
#36546 = CYLINDRICAL_SURFACE ( 'NONE', #22321, 120.5010000000000190 ) ;
#36547 = DIRECTION ( 'NONE',  ( 0.000000000000000000, -0.7525707698561308057, -0.6585113790650474197 ) ) ;
#36548 = EDGE_CURVE ( 'NONE', #40777, #5141, #39806, .T. ) ;
#36549 = CARTESIAN_POINT ( 'NONE',  ( 1.798435537469519230E-14, -1.196353617197826191E-13, -44.99999999999999289 ) ) ;
#36550 = ORIENTED_EDGE ( 'NONE', *, *, #19494, .T. ) ;
#36551 = CARTESIAN_POINT ( 'NONE',  ( 0.000000000000000000, 0.000000000000000000, -4.000000000000000000 ) ) ;
#36552 = CIRCLE ( 'NONE', #27527, 13.60000000000000320 ) ;
#36553 = VERTEX_POINT ( 'NONE', #17612 ) ;
#36554 = FACE_OUTER_BOUND ( 'NONE', #26854, .T. ) ;
#36555 = FACE_OUTER_BOUND ( 'NONE', #6719, .T. ) ;
#36556 = CARTESIAN_POINT ( 'NONE',  ( -6.238242335983215092, 31.00000000000000355, 47.40213128959678102 ) ) ;
#36557 = FACE_OUTER_BOUND ( 'NONE', #32132, .T. ) ;
#36558 = VERTEX_POINT ( 'NONE', #26967 ) ;
#36559 = ADVANCED_FACE ( 'NONE', ( #17172 ), #14106, .F. ) ;
#36560 = VECTOR ( 'NONE', #16861, 1000.000000000000000 ) ;
#36561 = CIRCLE ( 'NONE', #8709, 47.49900000000000233 ) ;
#36562 = EDGE_CURVE ( 'NONE', #14260, #15934, #23282, .T. ) ;
#36563 = CARTESIAN_POINT ( 'NONE',  ( 17.99999999999999645, -69.72480978689985420, -92.70626138606085931 ) ) ;
#36564 = ORIENTED_EDGE ( 'NONE', *, *, #11378, .F. ) ;
#36565 = CARTESIAN_POINT ( 'NONE',  ( 90.64482129758324902, 31.00000000000000000, 30.77200948131585889 ) ) ;
#36566 = CIRCLE ( 'NONE', #18517, 59.00000000000000711 ) ;
#36567 = ADVANCED_FACE ( 'NONE', ( #960 ), #36852, .T. ) ;
#36568 = EDGE_LOOP ( 'NONE', ( #28435, #42217, #39136, #7038 ) ) ;
#36569 = VECTOR ( 'NONE', #14614, 1000.000000000000000 ) ;
#36570 = CARTESIAN_POINT ( 'NONE',  ( 17.99999999999999645, 0.000000000000000000, 0.000000000000000000 ) ) ;
#36571 = ORIENTED_EDGE ( 'NONE', *, *, #35593, .T. ) ;
#36572 = CARTESIAN_POINT ( 'NONE',  ( 59.60939625460783731, 31.00000000000000000, -29.27517545780145269 ) ) ;
#36574 = CARTESIAN_POINT ( 'NONE',  ( -20.51812799677388455, 40.00000000000000000, -60.74091093256832607 ) ) ;
#36573 = CIRCLE ( 'NONE', #12940, 59.00000000000000000 ) ;
#36575 = FACE_OUTER_BOUND ( 'NONE', #22488, .T. ) ;
#36576 = CIRCLE ( 'NONE', #8723, 14.99999999999999822 ) ;
#36577 = VERTEX_POINT ( 'NONE', #9932 ) ;
#36578 = ORIENTED_EDGE ( 'NONE', *, *, #17656, .F. ) ;
#36579 = CARTESIAN_POINT ( 'NONE',  ( -3.453038570459499024, -2.625189405340453419, -3.535263753545272891 ) ) ;
#36580 = DIRECTION ( 'NONE',  ( 0.000000000000000000, 0.000000000000000000, 1.000000000000000000 ) ) ;
#36581 = DIRECTION ( 'NONE',  ( 0.000000000000000000, -0.9980267284282722251, 0.06279051952930256308 ) ) ;
#36583 = VERTEX_POINT ( 'NONE', #10378 ) ;
#36582 = CARTESIAN_POINT ( 'NONE',  ( 0.000000000000000000, 0.000000000000000000, 0.000000000000000000 ) ) ;
#36584 = CARTESIAN_POINT ( 'NONE',  ( 17.99999999999999645, 2.007101075699966763, 31.43498920425970411 ) ) ;
#36585 = ORIENTED_EDGE ( 'NONE', *, *, #20312, .F. ) ;
#36586 = FACE_OUTER_BOUND ( 'NONE', #3261, .T. ) ;
#36587 = ADVANCED_FACE ( 'NONE', ( #7300 ), #3373, .T. ) ;
#36588 = CARTESIAN_POINT ( 'NONE',  ( 5.399612364985509672, 40.00000000000000000, -82.60416666586320389 ) ) ;
#36589 = CARTESIAN_POINT ( 'NONE',  ( 18.00000000000000355, -41.20225022064620646, -23.63323037071445043 ) ) ;
#36590 = EDGE_CURVE ( 'NONE', #29580, #2582, #31301, .T. ) ;
#36591 = CIRCLE ( 'NONE', #42160, 120.5010000000000332 ) ;
#36592 = VERTEX_POINT ( 'NONE', #33931 ) ;
#36593 = CARTESIAN_POINT ( 'NONE',  ( 0.000000000000000000, 24.47917365150008706, -45.87777302070908547 ) ) ;
#36594 = EDGE_CURVE ( 'NONE', #7115, #501, #4815, .T. ) ;
#36595 = CARTESIAN_POINT ( 'NONE',  ( 5.991980000000000750, 1.836970198721029983E-15, -15.00000000000000355 ) ) ;
#36596 = AXIS2_PLACEMENT_3D ( 'NONE', #15419, #28294, #31760 ) ;
#36597 = ORIENTED_EDGE ( 'NONE', *, *, #40540, .T. ) ;
#36598 = AXIS2_PLACEMENT_3D ( 'NONE', #40361, #13358, #13572 ) ;
#36599 = AXIS2_PLACEMENT_3D ( 'NONE', #12831, #38199, #6055 ) ;
#36600 = ORIENTED_EDGE ( 'NONE', *, *, #8796, .F. ) ;
#36601 = DIRECTION ( 'NONE',  ( -1.000000000000000000, -0.000000000000000000, -0.000000000000000000 ) ) ;
#36602 = EDGE_LOOP ( 'NONE', ( #11901, #4683, #24462, #42965 ) ) ;
#36603 = CARTESIAN_POINT ( 'NONE',  ( 3.245924575715140481, 40.00000000000000000, -24.54795925723446359 ) ) ;
#36604 = CIRCLE ( 'NONE', #1762, 59.00000000000000711 ) ;
#36605 = CYLINDRICAL_SURFACE ( 'NONE', #34174, 120.5010000000000190 ) ;
#36606 = CARTESIAN_POINT ( 'NONE',  ( -8.749793197483594298, -2.055254544495723756, 2.972870684497274762 ) ) ;
#36607 = AXIS2_PLACEMENT_3D ( 'NONE', #28356, #41833, #41623 ) ;
#36608 = DIRECTION ( 'NONE',  ( 1.000000000000000000, 0.000000000000000000, 0.000000000000000000 ) ) ;
#36609 = CARTESIAN_POINT ( 'NONE',  ( 20.00000000000001066, -1.127613248556854817E-13, -25.99999999999999645 ) ) ;
#36610 = ORIENTED_EDGE ( 'NONE', *, *, #11590, .F. ) ;
#36611 = DIRECTION ( 'NONE',  ( 0.000000000000000000, -0.6736956436465478815, -0.7390089172206675272 ) ) ;
#36612 = ADVANCED_FACE ( 'NONE', ( #20233 ), #23715, .T. ) ;
#36614 = ORIENTED_EDGE ( 'NONE', *, *, #35678, .F. ) ;
#36613 = AXIS2_PLACEMENT_3D ( 'NONE', #4847, #687, #17342 ) ;
#36615 = DIRECTION ( 'NONE',  ( 0.000000000000000000, 0.000000000000000000, 1.000000000000000000 ) ) ;
#36616 = CARTESIAN_POINT ( 'NONE',  ( 18.00000000000000355, 0.000000000000000000, 0.000000000000000000 ) ) ;
#36617 = VERTEX_POINT ( 'NONE', #6658 ) ;
#36618 = PLANE ( 'NONE',  #13466 ) ;
#36619 = CARTESIAN_POINT ( 'NONE',  ( 0.000000000000000000, 105.3681574666264282, 38.54638589714925700 ) ) ;
#36620 = CONTEXT_DEPENDENT_SHAPE_REPRESENTATION ( #39818, #40200 ) ;
#36621 = EDGE_CURVE ( 'NONE', #3514, #18580, #13181, .T. ) ;
#36622 = DIRECTION ( 'NONE',  ( -1.000000000000000000, 0.000000000000000000, 0.000000000000000000 ) ) ;
#36623 = CARTESIAN_POINT ( 'NONE',  ( 64.36038921521112854, 31.00000000000000000, -37.17434371002195803 ) ) ;
#36624 = ORIENTED_EDGE ( 'NONE', *, *, #6788, .F. ) ;
#36625 = CARTESIAN_POINT ( 'NONE',  ( -4.434938641671373638, 31.00000000000000355, -34.07637162043106116 ) ) ;
#36626 = EDGE_CURVE ( 'NONE', #5699, #23465, #21598, .T. ) ;
#36627 = CARTESIAN_POINT ( 'NONE',  ( 29.59587406094124873, 40.00000000000000000, 60.01321678176139329 ) ) ;
#36628 = AXIS2_PLACEMENT_3D ( 'NONE', #33357, #3439, #23568 ) ;
#36629 = VECTOR ( 'NONE', #5143, 1000.000000000000000 ) ;
#36630 = DIRECTION ( 'NONE',  ( -1.000000000000000000, 0.000000000000000000, 0.000000000000000000 ) ) ;
#36631 = VECTOR ( 'NONE', #21978, 1000.000000000000000 ) ;
#36632 = DIRECTION ( 'NONE',  ( 0.000000000000000000, 0.000000000000000000, 1.000000000000000000 ) ) ;
#36633 = AXIS2_PLACEMENT_3D ( 'NONE', #37538, #10709, #4145 ) ;
#36634 = ORIENTED_EDGE ( 'NONE', *, *, #3683, .F. ) ;
#36635 = DIRECTION ( 'NONE',  ( -0.000000000000000000, -0.000000000000000000, 1.000000000000000000 ) ) ;
#36636 = DIRECTION ( 'NONE',  ( 1.000000000000000000, -0.000000000000000000, -0.000000000000000000 ) ) ;
#36637 = VERTEX_POINT ( 'NONE', #24583 ) ;
#36638 = CARTESIAN_POINT ( 'NONE',  ( -3.763366191185464782, 40.00000000000000000, 57.60416666550938203 ) ) ;
#36639 = DIRECTION ( 'NONE',  ( 1.000000000000000000, 0.000000000000000000, 0.000000000000000000 ) ) ;
#36641 = EDGE_CURVE ( 'NONE', #3331, #38633, #18107, .T. ) ;
#36640 = DIRECTION ( 'NONE',  ( 0.000000000000000000, 0.000000000000000000, 1.000000000000000000 ) ) ;
#36642 = VERTEX_POINT ( 'NONE', #15201 ) ;
#36643 = EDGE_CURVE ( 'NONE', #27712, #27725, #7957, .T. ) ;
#36644 = CARTESIAN_POINT ( 'NONE',  ( 17.99999999999999645, 51.98489025774302519, 108.7109110710163549 ) ) ;
#36645 = CARTESIAN_POINT ( 'NONE',  ( 17.99999999999999645, -31.80866420683992857, 2.997093558041182160 ) ) ;
#36646 = EDGE_LOOP ( 'NONE', ( #28477, #40252, #36708, #32312 ) ) ;
#36647 = DIRECTION ( 'NONE',  ( -1.000000000000000000, 0.000000000000000000, -0.000000000000000000 ) ) ;
#36648 = EDGE_LOOP ( 'NONE', ( #23859, #42953, #34483, #35515 ) ) ;
#36649 = EDGE_LOOP ( 'NONE', ( #42115, #20781, #34971, #31261 ) ) ;
#36650 = DIRECTION ( 'NONE',  ( -1.000000000000000000, 2.668805347656626987E-17, 0.000000000000000000 ) ) ;
#36651 = CARTESIAN_POINT ( 'NONE',  ( -30.16842255227261660, 31.00000000000000355, -89.21315370691763746 ) ) ;
#36652 = ORIENTED_EDGE ( 'NONE', *, *, #38876, .F. ) ;
#36653 = DIRECTION ( 'NONE',  ( 0.000000000000000000, 0.000000000000000000, 1.000000000000000000 ) ) ;
#36654 = VECTOR ( 'NONE', #8145, 1000.000000000000000 ) ;
#36655 = DIRECTION ( 'NONE',  ( -1.000000000000000000, -0.000000000000000000, 0.000000000000000000 ) ) ;
#36656 = AXIS2_PLACEMENT_3D ( 'NONE', #19065, #28453, #12286 ) ;
#36658 = CARTESIAN_POINT ( 'NONE',  ( 0.000000000000000000, 69.72480978690046527, 92.70626138606037614 ) ) ;
#36657 = VECTOR ( 'NONE', #22023, 1000.000000000000000 ) ;
#36659 = ORIENTED_EDGE ( 'NONE', *, *, #35496, .T. ) ;
#36660 = AXIS2_PLACEMENT_3D ( 'NONE', #26948, #10574, #20001 ) ;
#36661 = DIRECTION ( 'NONE',  ( 1.000000000000000000, 0.000000000000000000, 0.000000000000000000 ) ) ;
#36662 = ADVANCED_FACE ( 'NONE', ( #17824 ), #1840, .F. ) ;
#36663 = DIRECTION ( 'NONE',  ( 3.009274222672345096E-17, 1.000000000000000000, -2.455023325076455345E-18 ) ) ;
#36665 = DIRECTION ( 'NONE',  ( -1.000000000000000000, -0.000000000000000000, -0.000000000000000000 ) ) ;
#36664 = CARTESIAN_POINT ( 'NONE',  ( 8.999999999999998224, -24.70533337038204635, -26.18485254986720179 ) ) ;
#36666 = DIRECTION ( 'NONE',  ( 0.000000000000000000, 0.000000000000000000, 1.000000000000000000 ) ) ;
#36667 = ORIENTED_EDGE ( 'NONE', *, *, #2413, .F. ) ;
#36668 =( LENGTH_UNIT ( ) NAMED_UNIT ( * ) SI_UNIT ( .MILLI., .METRE. ) );
#36669 = EDGE_CURVE ( 'NONE', #32336, #40198, #34086, .T. ) ;
#36670 = CARTESIAN_POINT ( 'NONE',  ( 32.71557229150619861, 31.00000000000000355, -11.11602612089219910 ) ) ;
#36671 = ORIENTED_EDGE ( 'NONE', *, *, #19066, .T. ) ;
#36672 = DIRECTION ( 'NONE',  ( 1.000000000000000000, 0.000000000000000000, 0.000000000000000000 ) ) ;
#36673 = ADVANCED_FACE ( 'NONE', ( #38480 ), #1618, .F. ) ;
#36674 = CARTESIAN_POINT ( 'NONE',  ( 26.80287614962791309, -12.05525454449571932, 69.29271901957253021 ) ) ;
#36675 = ORIENTED_EDGE ( 'NONE', *, *, #39352, .T. ) ;
#36676 = AXIS2_PLACEMENT_3D ( 'NONE', #14727, #24774, #14510 ) ;
#36677 = CARTESIAN_POINT ( 'NONE',  ( 0.000000000000000000, 0.000000000000000000, 0.000000000000000000 ) ) ;
#36678 = CARTESIAN_POINT ( 'NONE',  ( -30.97228021248666607, 40.00000000000000000, 23.76985434021725041 ) ) ;
#36679 = CARTESIAN_POINT ( 'NONE',  ( -49.95450512539639476, 40.00000000000000000, 13.28959769214884545 ) ) ;
#36680 = ORIENTED_EDGE ( 'NONE', *, *, #13407, .T. ) ;
#36681 = VERTEX_POINT ( 'NONE', #5339 ) ;
#36682 = DIRECTION ( 'NONE',  ( 1.000000000000000000, 0.000000000000000000, 0.000000000000000000 ) ) ;
#36683 = CARTESIAN_POINT ( 'NONE',  ( 17.99999999999999645, -97.89532456239460601, -54.81585448086294576 ) ) ;
#36684 = ADVANCED_FACE ( 'NONE', ( #34357 ), #4453, .F. ) ;
#36685 = AXIS2_PLACEMENT_3D ( 'NONE', #10860, #6918, #37237 ) ;
#36686 = DIRECTION ( 'NONE',  ( 0.000000000000000000, 0.9980267284282712259, 0.06279051952931682945 ) ) ;
#36687 = VECTOR ( 'NONE', #7723, 1000.000000000000000 ) ;
#36688 = ORIENTED_EDGE ( 'NONE', *, *, #20310, .F. ) ;
#36689 = CARTESIAN_POINT ( 'NONE',  ( 0.000000000000000000, 16.77566611177774902, 119.3275660838943111 ) ) ;
#36690 = ORIENTED_EDGE ( 'NONE', *, *, #34243, .F. ) ;
#36691 = DIRECTION ( 'NONE',  ( 0.9247238835424299586, 4.035472873002398249E-16, 0.3806385939525924744 ) ) ;
#36692 = DIRECTION ( 'NONE',  ( -1.000000000000000000, 2.668805347656626370E-17, 0.000000000000000000 ) ) ;
#36693 = CIRCLE ( 'NONE', #41599, 10.49999999999998934 ) ;
#36694 = CIRCLE ( 'NONE', #9561, 20.00000000000000000 ) ;
#36695 = EDGE_CURVE ( 'NONE', #34974, #20768, #34777, .T. ) ;
#36696 = ORIENTED_EDGE ( 'NONE', *, *, #12562, .T. ) ;
#36697 = EDGE_CURVE ( 'NONE', #1103, #640, #27129, .T. ) ;
#36698 = AXIS2_PLACEMENT_3D ( 'NONE', #17385, #36748, #37181 ) ;
#36699 = CARTESIAN_POINT ( 'NONE',  ( 0.000000000000000000, -27.43636312076294814, -38.14186064215179073 ) ) ;
#36700 = ADVANCED_FACE ( 'NONE', ( #5113, #41099 ), #35005, .F. ) ;
#36701 = EDGE_CURVE ( 'NONE', #4217, #4058, #8303, .T. ) ;
#36702 = CYLINDRICAL_SURFACE ( 'NONE', #345, 116.0000000000000000 ) ;
#36703 = EDGE_LOOP ( 'NONE', ( #9011, #33736, #3702, #22430 ) ) ;
#36704 = CARTESIAN_POINT ( 'NONE',  ( 17.99999999999999645, -42.87700105098536341, -107.7847984684009219 ) ) ;
#36705 = EDGE_LOOP ( 'NONE', ( #4320, #31270, #1721, #42600 ) ) ;
#36706 = DIRECTION ( 'NONE',  ( -1.000000000000000000, 0.000000000000000000, 0.000000000000000000 ) ) ;
#36707 = CIRCLE ( 'NONE', #8066, 0.08000000000000020983 ) ;
#36708 = ORIENTED_EDGE ( 'NONE', *, *, #31235, .T. ) ;
#36710 = ORIENTED_EDGE ( 'NONE', *, *, #41082, .F. ) ;
#36709 = CARTESIAN_POINT ( 'NONE',  ( 0.000000000000000000, 0.000000000000000000, 0.000000000000000000 ) ) ;
#36711 = CIRCLE ( 'NONE', #38837, 120.5010000000000332 ) ;
#36712 = CARTESIAN_POINT ( 'NONE',  ( 66.75914267695947046, 31.00000000000000000, 8.899205196610871837 ) ) ;
#36713 = EDGE_LOOP ( 'NONE', ( #21640, #42031, #33792, #29491 ) ) ;
#36714 = DIRECTION ( 'NONE',  ( -1.000000000000000000, 0.000000000000000000, 0.000000000000000000 ) ) ;
#36715 = EDGE_CURVE ( 'NONE', #35838, #31678, #28551, .T. ) ;
#36716 = ORIENTED_EDGE ( 'NONE', *, *, #10010, .T. ) ;
#36717 = CARTESIAN_POINT ( 'NONE',  ( 18.00000000000000355, -0.6505223195679212811, -51.99593080916758936 ) ) ;
#36718 = B_SPLINE_SURFACE_WITH_KNOTS ( 'NONE', 1, 3, ( 
 ( #21890, #5264, #11838, #25368, #38844, #35145, #34499, #4609, #17984, #31255, #18632, #8109, #34730, #8325, #4837, #25167, #21684, #18198, #28426, #31465, #1552, #41470, #11619, #31893, #24958, #1981, #31669, #38209, #34937, #5047, #1769, #15123, #19709, #36236, #954, #23409, #19285, #35799, #36027, #32761, #6152, #9209, #19498, #12512, #26664, #39719, #2849, #42365, #25824, #29728, #32555, #6359, #2643, #26239, #16002, #29506, #16662, #9419, #19930, #12931, #23200, #29091, #6564, #3281, #16210, #42773, #9849, #32973, #29300, #42570, #32338, #22558, #39087, #33201, #29948, #16425, #39510, #3053, #5927, #12718, #13370, #9648, #39931, #6793, #10065, #26022, #22995, #43000, #39284, #13157, #22775, #26450, #36450, #36670, #2421, #15787, #4151, #27761, #20360, #7657, #3497, #17316, #7003, #1096, #14452, #21020, #30158, #41021, #24288, #33621, #24058, #3705, #14016, #17083, #30595, #4366, #40374, #34272, #659, #10957, #16875, #37545, #17737, #3930, #7216, #27529, #37327, #30368, #450, #20154, #10291, #26881, #31008, #11167, #17521, #20572, #7443, #40154, #213, #24503, #33841, #37754, #33414, #13584, #13810, #27313, #20803, #27108, #40582, #23638, #873, #36894, #34066, #10720, #10505, #30798, #23845, #37110, #14227, #40801, #5034, #37969, #32086, #2169, #38610, #17967, #28826, #12042, #11827, #18616, #18831, #1533, #15530, #25357, #8731, #31656, #41451, #11602, #15327, #42092, #18390, #8312, #35352, #25150, #28184, #5470, #38403, #21460, #12244, #24943, #28413, #25572, #22095, #1750, #41682, #38192, #8521, #7871, #11381, #4591, #8091, #21231, #21669, #28616, #15108, #34708, #41887, #21877, #35129, #34481, #31238, #5247, #14885, #31881, #1968, #1325, #14668, #34922, #27975, #41237, #24712, #4824, #18182, #31447, #42311, #42521, #39238, #12669, #15735, #25980, #19029, #33148, #3007, #9368, #5671, #32288, #36196, #9803, #19879, #16614, #2373, #43170, #6517, #26187, #22952, #16161, #29678, #13324, #39463, #36407, #39677, #32929, #29907, #9601, #16375, #23154, #22724, #38834, #29463, #35978, #29045, #2799, #12467, #25781, #42952, #39035, #42726, #9160, #12881, #6105, #32507, #35749, #6311, #3233, #2597, #19453, #19662, #13112, #22514, #8957, #15957, #22306, #35552, #29257, #5881, #19235, #32717, #26410, #30546, #37063, #3455, #20314, #13969, #40101, #4102, #13756, #7390, #13534, #1047, #27265, #26830, #27060, #40326, #33576, #10902, #10238, #7609, #34016, #37499, #17475, #20970, #7168, #3877, #36850, #23586, #23795, #30110, #30752, #34225, #24236, #27478, #3661, #17033, #614, #26617, #20751, #827, #14180, #39886, #6957, #10015, #20525, #30320, #168, #40752, #393, #33791, #10460, #10673, #17263, #4318, #40534, #17689, #24010, #30958, #23361, #33368, #36623, #6745, #20109, #37275, #16828, #38144, #8270, #25109, #28573, #22043, #21182, #11122, #8472, #21834, #21624, #18342, #34434, #34874, #31604, #4988, #1918, #40976, #1700, #21408, #15057, #38357, #35080, #24451, #14835, #28363, #41631, #11782, #25312, #5420, #1277, #17915, #18136, #28133, #31400, #4538, #1484, #37705, #8681, #5194, #41401, #7825, #31190, #18561, #14621, #31832, #27928, #15284, #41184, #11551, #41843, #34660, #11993, #38557, #35299, #11332, #18786, #32040, #24893, #14397, #27709, #24663, #37920, #8041, #4779, #35507, #8909, #2957, #16320, #29414, #32457, #32671, #22261, #12198, #19610, #2545, #9754, #19824, #29626, #38988, #25934, #2749, #25737, #15907, #38779, #26138, #5626, #19406, #22674, #35706, #42680, #23108, #2323, #32878, #28783, #42474, #32245, #26362, #39628, #42901, #25523, #36355, #6261, #6054, #12829, #13062, #9113, #6468, #2124, #15487, #39194, #5833, #19189, #9550, #42043, #12621, #29206, #18988, #16114, #22466, #15688, #39413, #28994, #42260, #9317, #35927, #12417, #22903, #36145, #10406, #20261, #23739, #33091, #36565, #29858, #33318, #10845, #23530, #10622, #335, #3404, #40483, #17422, #10181, #20694, #13701, #23953, #43121, #7332, #4048, #16982, #33526, #37220, #7118, #16772, #116, #3179, #23310, #39836, #33961, #30700, #17205, #3611 ),
 ( #36796, #40274, #30061, #30489, #13482, #24178, #6693, #776, #6902, #14131, #27425, #9961, #16553, #37440, #40693, #26773, #20053, #27002, #37011, #567, #7560, #13268, #40044, #26565, #27213, #30265, #20472, #33734, #3819, #13918, #35606, #2429, #42374, #14341, #25832, #32344, #8794, #5525, #41942, #12303, #39094, #22152, #19080, #22359, #15580, #12518, #35410, #28879, #5725, #7985, #20918, #12092, #21348, #27653, #28675, #40920, #11072, #42146, #24400, #25410, #21132, #38670, #31941, #14570, #17856, #18882, #15792, #27871, #18679, #32141, #2221, #37651, #29097, #41128, #34168, #4268, #11278, #30904, #17640, #991, #24611, #25627, #2018, #7772, #37864, #38892, #34380, #9008, #34601, #4480, #31132, #1219, #4716, #15382, #3289, #19291, #9656, #39729, #9856, #13164, #20162, #219, #39293, #12725, #12942, #23001, #26246, #29308, #39517, #32561, #3506, #16668, #36245, #2649, #16009, #6572, #9428, #26457, #22782, #3061, #36035, #6368, #36678, #29513, #39939, #32979, #8, #5933, #26670, #23417, #19716, #16433, #29954, #23208, #6159, #19504, #9214, #42576, #26028, #10071, #6800, #36457, #29737, #19938, #32773, #2856, #33420, #43007, #16883, #26891, #30165, #16216, #33207, #13378, #42780, #13592, #22565, #35805, #30379, #14234, #17532, #30601, #24296, #4602, #40380, #27770, #23644, #37335, #27116, #21238, #34491, #41028, #7013, #17976, #1108, #882, #7664, #7881, #33851, #31246, #14461, #11177, #20813, #666, #14027, #4373, #1332, #7449, #40588, #24513, #27538, #17323, #37762, #40813, #10516, #14675, #27322, #30806, #40161, #10299, #34073, #10965, #10726, #37555, #36902, #457, #20366, #23851, #33629, #24066, #17746, #4157, #37116, #31016, #21030, #34281, #3711, #17089, #13817, #3939, #7224, #20579, #34718, #4832, #22101, #18189, #35138, #28190, #31888, #38411, #21675, #24952, #15334, #38839, #34931, #25157, #28622, #1975, #31457, #28832, #5040, #35557, #19035, #18400, #37976, #22312, #8103, #31661, #41896, #8527, #1544, #1757, #12048, #41460, #5478, #15117, #8741, #14892, #2378, #25363, #11611, #28418, #41691, #11832, #12250, #38200, #8963, #35357, #5680, #18835, #32295, #21883, #5256, #8318, #18624, #38614, #32093, #2175, #27987, #25582, #42098, #15536, #41245, #11388, #24721, #21467, #23164, #36410, #33373, #12677, #42320, #39468, #22729, #19241, #6522, #19459, #22957, #42525, #42957, #25985, #36627, #32514, #43174, #35984, #26621, #13328, #22522, #15743, #20113, #3239, #39245, #35756, #9606, #36199, #26415, #29911, #23364, #5885, #12472, #9807, #19884, #6319, #19668, #2601, #32933, #39894, #10020, #6750, #9168, #29049, #25785, #3011, #13117, #16378, #33153, #39042, #29683, #15967, #16619, #29261, #9373, #39680, #6109, #32725, #2804, #16169, #29469, #42730, #12886, #26193, #20762, #17038, #13762, #3458, #36856, #10244, #4323, #17693, #30755, #33794, #34019, #23590, #13541, #20973, #3886, #11130, #21186, #30963, #40331, #27269, #4107, #27063, #17269, #40105, #27483, #6961, #17478, #24016, #37069, #834, #24455, #3664, #34229, #30117, #618, #33582, #27716, #40979, #1050, #26833, #37708, #7613, #7395, #14184, #14403, #10464, #7830, #16832, #172, #40541, #7173, #20530, #10908, #20317, #13972, #30550, #30327, #40756, #23799, #397, #24242, #10677, #37279, #37506, #11786, #15490, #5427, #31607, #25114, #21629, #38360, #34439, #37924, #31195, #34666, #12204, #24897, #11996, #1704, #4782, #41847, #8476, #21839, #22046, #17920, #35088, #41408, #41638, #1924, #28579, #1281, #34878, #5200, #18564, #31837, #2128, #25528, #21413, #8044, #38152, #4992, #8273, #11337, #18351, #14626, #28787, #25316, #15061, #27936, #41188, #15287, #18141, #38561, #31404, #28367, #1491, #8689, #18789, #11554, #35303, #32044, #42047, #24668, #38783, #8916, #4542, #14840, #28136, #2758, #29211, #25742, #13068, #25939, #29420, #5839, #6270, #19196, #43127, #38996, #6473, #42482, #33098, #19831, #28998, #22266, #26572, #9761, #32463, #42267, #16120, #42686, #32884, #36361, #29866, #12424, #18993, #16326, #29633, #12835, #26146, #9118, #39419, #3184, #16562 ) ),
 .UNSPECIFIED., .F., .F., .F.,
 ( 2, 2 ),
 ( 4, 2, 2, 2, 2, 2, 2, 2, 2, 2, 2, 2, 2, 2, 2, 2, 2, 2, 2, 2, 2, 2, 2, 2, 2, 2, 2, 2, 2, 2, 2, 2, 2, 2, 2, 2, 2, 2, 2, 2, 2, 2, 2, 2, 2, 2, 2, 2, 2, 2, 2, 2, 2, 2, 2, 2, 2, 2, 2, 2, 2, 2, 2, 2, 2, 2, 2, 2, 2, 2, 2, 2, 2, 2, 2, 2, 2, 2, 2, 2, 2, 2, 2, 2, 2, 2, 2, 2, 2, 2, 2, 2, 2, 2, 2, 2, 2, 2, 2, 2, 2, 2, 2, 2, 2, 2, 2, 2, 2, 2, 2, 2, 2, 2, 2, 2, 2, 2, 2, 2, 2, 2, 2, 2, 2, 2, 2, 2, 2, 2, 2, 2, 2, 2, 2, 2, 2, 2, 2, 2, 2, 2, 2, 2, 2, 2, 2, 2, 2, 2, 2, 2, 2, 2, 2, 2, 2, 2, 2, 2, 2, 2, 2, 2, 2, 2, 2, 2, 2, 2, 2, 2, 2, 2, 2, 2, 2, 2, 2, 2, 2, 2, 2, 2, 2, 2, 2, 2, 2, 2, 2, 2, 2, 2, 2, 2, 2, 2, 2, 2, 2, 2, 2, 2, 2, 2, 2, 2, 2, 2, 2, 2, 2, 2, 2, 2, 2, 2, 2, 2, 2, 2, 2, 2, 2, 2, 2, 2, 2, 2, 2, 2, 2, 2, 2, 2, 2, 2, 2, 2, 2, 2, 2, 2, 2, 2, 2, 2, 2, 2, 2, 2, 2, 2, 2, 2, 4 ),
 ( 0.000000000000000000, 0.4090909090909088941 ),
 ( 0.000000000000000000, 0.003906250000000000000, 0.007812500000000000000, 0.01171875000000000000, 0.01562500000000000000, 0.01953125000000000000, 0.02343750000000000000, 0.02734375000000000000, 0.03125000000000000000, 0.03515625000000000000, 0.03906250000000000000, 0.04296875000000000000, 0.04687500000000000000, 0.05078125000000000000, 0.05468750000000000000, 0.05859375000000000000, 0.06250000000000000000, 0.06640625000000000000, 0.07031250000000000000, 0.07421875000000000000, 0.07812500000000000000, 0.08203125000000000000, 0.08593750000000000000, 0.08984375000000000000, 0.09375000000000000000, 0.09765625000000000000, 0.1015625000000000000, 0.1054687500000000000, 0.1093750000000000000, 0.1132812500000000000, 0.1171875000000000000, 0.1210937500000000000, 0.1250000000000000000, 0.1289062500000000000, 0.1328125000000000000, 0.1367187500000000000, 0.1406250000000000000, 0.1445312500000000000, 0.1484375000000000000, 0.1523437500000000000, 0.1562500000000000000, 0.1601562500000000000, 0.1640625000000000000, 0.1679687500000000000, 0.1718750000000000000, 0.1757812500000000000, 0.1796875000000000000, 0.1835937500000000000, 0.1875000000000000000, 0.1914062500000000000, 0.1953125000000000000, 0.1992187500000000000, 0.2031250000000000000, 0.2070312500000000000, 0.2109375000000000000, 0.2148437500000000000, 0.2187500000000000000, 0.2226562500000000000, 0.2265625000000000000, 0.2304687500000000000, 0.2343750000000000000, 0.2382812500000000000, 0.2421875000000000000, 0.2460937500000000000, 0.2500000000000000000, 0.2539062500000000000, 0.2578125000000000000, 0.2617187500000000000, 0.2656250000000000000, 0.2695312500000000000, 0.2734375000000000000, 0.2773437500000000000, 0.2812500000000000000, 0.2851562500000000000, 0.2890625000000000000, 0.2929687500000000000, 0.2968750000000000000, 0.3007812500000000000, 0.3046875000000000000, 0.3085937500000000000, 0.3125000000000000000, 0.3164062500000000000, 0.3203125000000000000, 0.3242187500000000000, 0.3281250000000000000, 0.3320312500000000000, 0.3359375000000000000, 0.3398437500000000000, 0.3437500000000000000, 0.3476562500000000000, 0.3515625000000000000, 0.3554687500000000000, 0.3593750000000000000, 0.3632812500000000000, 0.3671875000000000000, 0.3710937500000000000, 0.3750000000000000000, 0.3789062500000000000, 0.3828125000000000000, 0.3867187500000000000, 0.3906250000000000000, 0.3945312500000000000, 0.3984375000000000000, 0.4023437500000000000, 0.4062500000000000000, 0.4101562500000000000, 0.4140625000000000000, 0.4179687500000000000, 0.4218750000000000000, 0.4257812500000000000, 0.4296875000000000000, 0.4335937500000000000, 0.4375000000000000000, 0.4414062500000000000, 0.4453125000000000000, 0.4492187500000000000, 0.4531250000000000000, 0.4570312500000000000, 0.4609375000000000000, 0.4648437500000000000, 0.4687500000000000000, 0.4726562500000000000, 0.4765625000000000000, 0.4804687500000000000, 0.4843750000000000000, 0.4882812500000000000, 0.4921875000000000000, 0.4960937500000000000, 0.5000000000000000000, 0.5039062500000000000, 0.5078125000000000000, 0.5117187500000000000, 0.5156250000000000000, 0.5195312500000000000, 0.5234375000000000000, 0.5273437500000000000, 0.5312500000000000000, 0.5351562500000000000, 0.5390625000000000000, 0.5429687500000000000, 0.5468750000000000000, 0.5507812500000000000, 0.5546875000000000000, 0.5585937500000000000, 0.5625000000000000000, 0.5664062500000000000, 0.5703125000000000000, 0.5742187500000000000, 0.5781250000000000000, 0.5820312500000000000, 0.5859375000000000000, 0.5898437500000000000, 0.5937500000000000000, 0.5976562500000000000, 0.6015625000000000000, 0.6054687500000000000, 0.6093750000000000000, 0.6132812500000000000, 0.6171875000000000000, 0.6210937500000000000, 0.6250000000000000000, 0.6289062500000000000, 0.6328125000000000000, 0.6367187500000000000, 0.6406250000000000000, 0.6445312500000000000, 0.6484375000000000000, 0.6523437500000000000, 0.6562500000000000000, 0.6601562500000000000, 0.6640625000000000000, 0.6679687500000000000, 0.6718750000000000000, 0.6757812500000000000, 0.6796875000000000000, 0.6835937500000000000, 0.6875000000000000000, 0.6914062500000000000, 0.6953125000000000000, 0.6992187500000000000, 0.7031250000000000000, 0.7070312500000000000, 0.7109375000000000000, 0.7148437500000000000, 0.7187500000000000000, 0.7226562500000000000, 0.7265625000000000000, 0.7304687500000000000, 0.7343750000000000000, 0.7382812500000000000, 0.7421875000000000000, 0.7460937500000000000, 0.7500000000000000000, 0.7539062500000000000, 0.7578125000000000000, 0.7617187500000000000, 0.7656250000000000000, 0.7695312500000000000, 0.7734375000000000000, 0.7773437500000000000, 0.7812500000000000000, 0.7851562500000000000, 0.7890625000000000000, 0.7929687500000000000, 0.7968750000000000000, 0.8007812500000000000, 0.8046875000000000000, 0.8085937500000000000, 0.8125000000000000000, 0.8164062500000000000, 0.8203125000000000000, 0.8242187500000000000, 0.8281250000000000000, 0.8320312500000000000, 0.8359375000000000000, 0.8398437500000000000, 0.8437500000000000000, 0.8476562500000000000, 0.8515625000000000000, 0.8554687500000000000, 0.8593750000000000000, 0.8632812500000000000, 0.8671875000000000000, 0.8710937500000000000, 0.8750000000000000000, 0.8789062500000000000, 0.8828125000000000000, 0.8867187500000000000, 0.8906250000000000000, 0.8945312500000000000, 0.8984375000000000000, 0.9023437500000000000, 0.9062500000000000000, 0.9101562500000000000, 0.9140625000000000000, 0.9179687500000000000, 0.9218750000000000000, 0.9257812500000000000, 0.9296875000000000000, 0.9335937500000000000, 0.9375000000000000000, 0.9414062500000000000, 0.9453125000000000000, 0.9492187500000000000, 0.9531250000000000000, 0.9570312500000000000, 0.9609375000000000000, 0.9648437500000000000, 0.9687500000000000000, 0.9726562500000000000, 0.9765625000000000000, 0.9804687500000000000, 0.9843750000000000000, 0.9882812500000000000, 0.9921875000000000000, 0.9960937500000000000, 1.000000000000000000 ),
 .UNSPECIFIED. ) ;
#36719 = ORIENTED_EDGE ( 'NONE', *, *, #25333, .T. ) ;
#36720 = CARTESIAN_POINT ( 'NONE',  ( -25.88810397297939403, 40.00000000000000000, 75.89534075015936310 ) ) ;
#36721 = AXIS2_PLACEMENT_3D ( 'NONE', #33923, #16944, #40234 ) ;
#36723 = CARTESIAN_POINT ( 'NONE',  ( -105.9879088449591933, 31.00000000000000000, -4.880719929157669945 ) ) ;
#36722 = FACE_OUTER_BOUND ( 'NONE', #6057, .T. ) ;
#36724 = CARTESIAN_POINT ( 'NONE',  ( 0.000000000000000000, -34.03109950475653989, -115.5957406979053133 ) ) ;
#36725 = ORIENTED_EDGE ( 'NONE', *, *, #22577, .F. ) ;
#36726 = CYLINDRICAL_SURFACE ( 'NONE', #43049, 116.0000000000000000 ) ;
#36727 = ORIENTED_EDGE ( 'NONE', *, *, #30085, .F. ) ;
#36728 = CIRCLE ( 'NONE', #24234, 20.00000000000000355 ) ;
#36729 = VECTOR ( 'NONE', #13656, 1000.000000000000000 ) ;
#36730 = DIRECTION ( 'NONE',  ( 0.000000000000000000, 0.000000000000000000, 1.000000000000000000 ) ) ;
#36731 = CIRCLE ( 'NONE', #36041, 51.99999999999999289 ) ;
#36732 = CARTESIAN_POINT ( 'NONE',  ( 74.89583333416871369, 31.00000000000000000, -4.908738512848213276 ) ) ;
#36733 = ADVANCED_FACE ( 'NONE', ( #25235 ), #11467, .F. ) ;
#36735 = CARTESIAN_POINT ( 'NONE',  ( 0.6810597143197052450, 4.461075778259290914, -3.598441714920602053 ) ) ;
#36734 = FACE_OUTER_BOUND ( 'NONE', #3305, .T. ) ;
#36737 = ORIENTED_EDGE ( 'NONE', *, *, #38344, .T. ) ;
#36736 = VECTOR ( 'NONE', #23864, 1000.000000000000000 ) ;
#36738 = DIRECTION ( 'NONE',  ( 1.000000000000000000, 0.000000000000000000, 0.000000000000000000 ) ) ;
#36739 = AXIS2_PLACEMENT_3D ( 'NONE', #9946, #23295, #38973 ) ;
#36740 = EDGE_LOOP ( 'NONE', ( #37881, #28242, #39442, #27548 ) ) ;
#36741 = DIRECTION ( 'NONE',  ( -1.000000000000000000, -0.000000000000000000, -0.000000000000000000 ) ) ;
#36742 = CARTESIAN_POINT ( 'NONE',  ( 17.99999999999999645, 5.822172717930716779, -31.41458249383134671 ) ) ;
#36743 = CARTESIAN_POINT ( 'NONE',  ( 18.00000000000000355, -44.61570720899084819, -14.73072383765613047 ) ) ;
#36744 = FACE_OUTER_BOUND ( 'NONE', #8327, .T. ) ;
#36745 = VERTEX_POINT ( 'NONE', #41548 ) ;
#36746 = CARTESIAN_POINT ( 'NONE',  ( 17.99999999999999645, -23.10276247328181398, 118.2656051737069021 ) ) ;
#36747 = VERTEX_POINT ( 'NONE', #11693 ) ;
#36748 = DIRECTION ( 'NONE',  ( -1.000000000000000000, -0.000000000000000000, -0.000000000000000000 ) ) ;
#36749 = AXIS2_PLACEMENT_3D ( 'NONE', #2239, #15811, #28695 ) ;
#36750 = DIRECTION ( 'NONE',  ( 0.000000000000000000, 0.000000000000000000, 1.000000000000000000 ) ) ;
#36751 = EDGE_CURVE ( 'NONE', #38331, #19229, #31985, .T. ) ;
#36752 = EDGE_CURVE ( 'NONE', #4179, #5962, #43103, .T. ) ;
#36753 = DIRECTION ( 'NONE',  ( -1.000000000000000000, -0.000000000000000000, -0.000000000000000000 ) ) ;
#36754 = VERTEX_POINT ( 'NONE', #11046 ) ;
#36755 = VERTEX_POINT ( 'NONE', #24371 ) ;
#36756 = DIRECTION ( 'NONE',  ( 0.000000000000000000, -7.709882115452474222E-16, -1.000000000000000000 ) ) ;
#36757 = VECTOR ( 'NONE', #43176, 1000.000000000000000 ) ;
#36758 = CARTESIAN_POINT ( 'NONE',  ( 0.000000000000000000, 0.000000000000000000, 0.000000000000000000 ) ) ;
#36759 = AXIS2_PLACEMENT_3D ( 'NONE', #37654, #21134, #11075 ) ;
#36760 = EDGE_CURVE ( 'NONE', #35963, #23893, #37623, .T. ) ;
#36761 = LINE ( 'NONE', #42869, #18796 ) ;
#36762 = AXIS2_PLACEMENT_3D ( 'NONE', #11892, #32152, #12103 ) ;
#36764 = ORIENTED_EDGE ( 'NONE', *, *, #15602, .F. ) ;
#36763 = CARTESIAN_POINT ( 'NONE',  ( 17.99999999999999645, 51.98489025774302519, 108.7109110710163549 ) ) ;
#36765 = CARTESIAN_POINT ( 'NONE',  ( -3.925388345519843725, 31.00000000000000355, 29.51202942214661462 ) ) ;
#36766 = FACE_OUTER_BOUND ( 'NONE', #11275, .T. ) ;
#36767 = CIRCLE ( 'NONE', #39561, 116.0000000000000000 ) ;
#36768 = EDGE_CURVE ( 'NONE', #17054, #40002, #8987, .T. ) ;
#36770 = ORIENTED_EDGE ( 'NONE', *, *, #38570, .F. ) ;
#36769 = CARTESIAN_POINT ( 'NONE',  ( 18.00000000000000355, -37.91532898920940653, 28.61088654061626357 ) ) ;
#36771 = ORIENTED_EDGE ( 'NONE', *, *, #8955, .T. ) ;
#36772 = DIRECTION ( 'NONE',  ( 1.000000000000000000, 0.000000000000000000, 0.000000000000000000 ) ) ;
#36773 = CARTESIAN_POINT ( 'NONE',  ( 17.99999999999999645, -118.8387007424469601, -19.94628303336605768 ) ) ;
#36774 = CARTESIAN_POINT ( 'NONE',  ( 33.95200755731382714, 40.00000000000000000, -44.10258293181757949 ) ) ;
#36775 = CARTESIAN_POINT ( 'NONE',  ( 9.000000000000001776, 51.93417535146740960, -2.615612846549368431 ) ) ;
#36776 =( REPRESENTATION_RELATIONSHIP ('NONE','NONE', #330, #37437 ) REPRESENTATION_RELATIONSHIP_WITH_TRANSFORMATION ( #15053 )SHAPE_REPRESENTATION_RELATIONSHIP( ) );
#36777 = VECTOR ( 'NONE', #17406, 1000.000000000000000 ) ;
#36778 = EDGE_CURVE ( 'NONE', #19328, #39201, #2458, .T. ) ;
#36779 = EDGE_CURVE ( 'NONE', #40725, #2052, #5531, .T. ) ;
#36780 = DIRECTION ( 'NONE',  ( -1.000000000000000000, -0.000000000000000000, 0.000000000000000000 ) ) ;
#36781 = DIRECTION ( 'NONE',  ( 1.000000000000000000, 0.000000000000000000, 0.000000000000000000 ) ) ;
#36782 = ORIENTED_EDGE ( 'NONE', *, *, #13414, .T. ) ;
#36783 = DIRECTION ( 'NONE',  ( 1.000000000000000000, 0.000000000000000000, 0.000000000000000000 ) ) ;
#36784 = VERTEX_POINT ( 'NONE', #29127 ) ;
#36785 = DIRECTION ( 'NONE',  ( 1.000000000000000000, 0.000000000000000000, 0.000000000000000000 ) ) ;
#36786 = CARTESIAN_POINT ( 'NONE',  ( 0.000000000000000000, 64.69195966010022403, -96.28577441832183581 ) ) ;
#36787 = CARTESIAN_POINT ( 'NONE',  ( -42.66459923921424036, 31.00000000000000355, 24.64557685607233140 ) ) ;
#36788 = CIRCLE ( 'NONE', #29159, 59.00000000000000711 ) ;
#36789 = CARTESIAN_POINT ( 'NONE',  ( 0.000000000000000000, -73.51007459736489125, 89.73443560133338792 ) ) ;
#36790 = ORIENTED_EDGE ( 'NONE', *, *, #36085, .F. ) ;
#36791 = EDGE_CURVE ( 'NONE', #25336, #31117, #26464, .T. ) ;
#36792 = AXIS2_PLACEMENT_3D ( 'NONE', #15064, #28142, #41642 ) ;
#36793 = CIRCLE ( 'NONE', #18741, 116.0000000000000000 ) ;
#36794 = DIRECTION ( 'NONE',  ( -1.000000000000000000, -0.000000000000000000, 0.000000000000000000 ) ) ;
#36795 = EDGE_LOOP ( 'NONE', ( #34852, #23025, #39775, #17374 ) ) ;
#36796 = CARTESIAN_POINT ( 'NONE',  ( -19.99999999999999645, 40.00000000000000000, 0.000000000000000000 ) ) ;
#36797 = VECTOR ( 'NONE', #14721, 1000.000000000000000 ) ;
#36798 = VECTOR ( 'NONE', #24087, 1000.000000000000000 ) ;
#36799 = ORIENTED_EDGE ( 'NONE', *, *, #28168, .F. ) ;
#36800 = DIRECTION ( 'NONE',  ( 0.000000000000000000, 0.7980172272802408262, -0.6026346363792547400 ) ) ;
#36802 = CARTESIAN_POINT ( 'NONE',  ( 34.80713033128647993, 31.00000000000000355, 70.84796410819511436 ) ) ;
#36801 = AXIS2_PLACEMENT_3D ( 'NONE', #16738, #26742, #39164 ) ;
#36803 = CARTESIAN_POINT ( 'NONE',  ( -40.35386350238497499, 40.00000000000000000, 69.65762217234959053 ) ) ;
#36804 = DIRECTION ( 'NONE',  ( 0.000000000000000000, -0.5877852522924802425, 0.8090169943749422332 ) ) ;
#36805 = EDGE_LOOP ( 'NONE', ( #1119, #24745, #3486, #14950 ) ) ;
#36806 = ORIENTED_EDGE ( 'NONE', *, *, #41424, .T. ) ;
#36807 = CARTESIAN_POINT ( 'NONE',  ( 2.500000000000000000, 1.178949249685212974, -2.042000000000001148 ) ) ;
#36808 = CARTESIAN_POINT ( 'NONE',  ( 0.000000000000000000, 0.000000000000000000, 0.000000000000000000 ) ) ;
#36809 = CARTESIAN_POINT ( 'NONE',  ( -4.154094228333456762, 2.398367420968013253, -3.721909803043220055 ) ) ;
#36811 = EDGE_LOOP ( 'NONE', ( #14517, #3432, #41551, #23362 ) ) ;
#36810 = DIRECTION ( 'NONE',  ( -1.000000000000000000, -0.000000000000000000, -0.000000000000000000 ) ) ;
#36812 = EDGE_CURVE ( 'NONE', #29181, #42330, #6395, .T. ) ;
#36813 = CARTESIAN_POINT ( 'NONE',  ( 0.000000000000000000, 19.12429268481714928, 114.4126803693779948 ) ) ;
#36814 = VERTEX_POINT ( 'NONE', #5553 ) ;
#36815 = CYLINDRICAL_SURFACE ( 'NONE', #7011, 13.59999999999999964 ) ;
#36816 = CARTESIAN_POINT ( 'NONE',  ( -72.56464488860213180, 40.00000000000000711, -35.76892886290303863 ) ) ;
#36817 = FACE_OUTER_BOUND ( 'NONE', #30571, .T. ) ;
#36818 = VERTEX_POINT ( 'NONE', #12117 ) ;
#36819 = CARTESIAN_POINT ( 'NONE',  ( -20.39032260654148132, 40.00000000000000000, 1.150830359615497844 ) ) ;
#36820 = CIRCLE ( 'NONE', #24327, 142.4999999999992610 ) ;
#36821 = LINE ( 'NONE', #6930, #15551 ) ;
#36822 = AXIS2_PLACEMENT_3D ( 'NONE', #27233, #17878, #30721 ) ;
#36823 = EDGE_CURVE ( 'NONE', #28231, #22633, #29543, .T. ) ;
#36824 = ORIENTED_EDGE ( 'NONE', *, *, #10275, .T. ) ;
#36825 = CIRCLE ( 'NONE', #11797, 20.00000000000000355 ) ;
#36826 = EDGE_CURVE ( 'NONE', #35293, #25440, #38287, .T. ) ;
#36827 = FACE_OUTER_BOUND ( 'NONE', #13342, .T. ) ;
#36828 = ORIENTED_EDGE ( 'NONE', *, *, #16565, .T. ) ;
#36829 = CYLINDRICAL_SURFACE ( 'NONE', #28200, 120.5010000000000190 ) ;
#36830 = ORIENTED_EDGE ( 'NONE', *, *, #39422, .F. ) ;
#36831 = CARTESIAN_POINT ( 'NONE',  ( 22.71825314374767402, 40.00000000000000000, -13.09499307598873941 ) ) ;
#36832 = DIRECTION ( 'NONE',  ( 0.000000000000000000, 1.331914804436429787E-14, -1.000000000000000000 ) ) ;
#36833 = DIRECTION ( 'NONE',  ( 0.000000000000000000, 0.000000000000000000, 1.000000000000000000 ) ) ;
#36834 = EDGE_CURVE ( 'NONE', #35069, #7867, #32591, .T. ) ;
#36835 = DIRECTION ( 'NONE',  ( 1.000000000000000000, 0.000000000000000000, 0.000000000000000000 ) ) ;
#36836 = LINE ( 'NONE', #36390, #27602 ) ;
#36837 = VERTEX_POINT ( 'NONE', #12544 ) ;
#36839 = DIRECTION ( 'NONE',  ( -1.000000000000000000, 0.000000000000000000, 0.000000000000000000 ) ) ;
#36838 = DIRECTION ( 'NONE',  ( -1.000000000000000000, 0.000000000000000000, 0.000000000000000000 ) ) ;
#36840 = ORIENTED_EDGE ( 'NONE', *, *, #20212, .T. ) ;
#36841 = FILL_AREA_STYLE ('',( #27641 ) ) ;
#36842 = DIRECTION ( 'NONE',  ( -1.000000000000000000, 0.000000000000000000, 0.000000000000000000 ) ) ;
#36843 = CARTESIAN_POINT ( 'NONE',  ( -18.08361268445098347, 31.00000000000000355, -10.43497034982449456 ) ) ;
#36844 = ORIENTED_EDGE ( 'NONE', *, *, #4922, .F. ) ;
#36845 = CARTESIAN_POINT ( 'NONE',  ( 0.000000000000000000, 0.000000000000000000, 0.000000000000000000 ) ) ;
#36846 = DIRECTION ( 'NONE',  ( -1.000000000000000000, -0.000000000000000000, 0.000000000000000000 ) ) ;
#36847 = ADVANCED_FACE ( 'NONE', ( #8822 ), #22387, .T. ) ;
#36848 = CONTEXT_DEPENDENT_SHAPE_REPRESENTATION ( #26474, #20050 ) ;
#36849 = DIRECTION ( 'NONE',  ( 1.000000000000000000, 0.000000000000000000, 0.000000000000000000 ) ) ;
#36850 = CARTESIAN_POINT ( 'NONE',  ( -51.86900026051868196, 31.00000000000000355, 45.50549606403863123 ) ) ;
#36851 = ADVANCED_FACE ( 'NONE', ( #35635 ), #2673, .F. ) ;
#36852 = CONICAL_SURFACE ( 'NONE', #24351, 4.000000000000000000, 0.8911886515913786111 ) ;
#36853 = VERTEX_POINT ( 'NONE', #19742 ) ;
#36854 = AXIS2_PLACEMENT_3D ( 'NONE', #8876, #28960, #21595 ) ;
#36855 = CARTESIAN_POINT ( 'NONE',  ( 45.06603723660748528, 31.00000000000000355, 15.38899812203272788 ) ) ;
#36856 = CARTESIAN_POINT ( 'NONE',  ( 74.72486387243833406, 39.99999999999999289, 9.837939412698395003 ) ) ;
#36857 = CIRCLE ( 'NONE', #5507, 31.49900000000000588 ) ;
#36858 = CARTESIAN_POINT ( 'NONE',  ( 17.99999999999999645, 31.81777574834305966, -2.898764365605425830 ) ) ;
#36859 = DIRECTION ( 'NONE',  ( -1.000000000000000000, 0.000000000000000000, -0.000000000000000000 ) ) ;
#36860 = ORIENTED_EDGE ( 'NONE', *, *, #7384, .T. ) ;
#36861 = LINE ( 'NONE', #30332, #14926 ) ;
#36862 = CARTESIAN_POINT ( 'NONE',  ( 17.99999999999999645, 0.000000000000000000, 0.000000000000000000 ) ) ;
#36863 = EDGE_CURVE ( 'NONE', #16214, #13292, #16714, .T. ) ;
#36864 = VERTEX_POINT ( 'NONE', #32166 ) ;
#36865 = CARTESIAN_POINT ( 'NONE',  ( -50.10416666532988472, 40.00000000000000000, -3.272492339034341224 ) ) ;
#36866 = DIRECTION ( 'NONE',  ( -0.000000000000000000, -0.000000000000000000, -1.000000000000000000 ) ) ;
#36867 = CARTESIAN_POINT ( 'NONE',  ( 17.99999999999999645, 105.3681574666264282, 38.54638589714925700 ) ) ;
#36868 = ORIENTED_EDGE ( 'NONE', *, *, #20371, .T. ) ;
#36869 = DIRECTION ( 'NONE',  ( 0.000000000000000000, 0.5264321628773568351, -0.8502171357296134380 ) ) ;
#36870 = DIRECTION ( 'NONE',  ( -1.807003620809174385E-16, 1.000000000000000000, 0.000000000000000000 ) ) ;
#36871 = ORIENTED_EDGE ( 'NONE', *, *, #36950, .T. ) ;
#36872 = DIRECTION ( 'NONE',  ( -1.000000000000000000, -0.000000000000000000, 0.000000000000000000 ) ) ;
#36873 = ORIENTED_EDGE ( 'NONE', *, *, #3740, .F. ) ;
#36874 = ADVANCED_FACE ( 'NONE', ( #32798 ), #22813, .F. ) ;
#36875 = ORIENTED_EDGE ( 'NONE', *, *, #40859, .F. ) ;
#36876 = CARTESIAN_POINT ( 'NONE',  ( -8.749793197483594298, -12.05525454449572464, 2.972870684497274762 ) ) ;
#36877 = CARTESIAN_POINT ( 'NONE',  ( 28.55926749297819711, 31.00000000000000355, 84.46800049165048563 ) ) ;
#36878 = VERTEX_POINT ( 'NONE', #35837 ) ;
#36879 = CARTESIAN_POINT ( 'NONE',  ( 17.99999999999999645, 96.25468616236763353, -72.49500943364391503 ) ) ;
#36880 = CIRCLE ( 'NONE', #36188, 116.0000000000000000 ) ;
#36881 = VECTOR ( 'NONE', #33930, 1000.000000000000000 ) ;
#36882 = CARTESIAN_POINT ( 'NONE',  ( 0.000000000000000000, 0.000000000000000000, 0.000000000000000000 ) ) ;
#36883 = EDGE_CURVE ( 'NONE', #4444, #24289, #6238, .T. ) ;
#36884 = CARTESIAN_POINT ( 'NONE',  ( 17.99999999999999645, 0.000000000000000000, 0.000000000000000000 ) ) ;
#36885 = AXIS2_PLACEMENT_3D ( 'NONE', #20773, #628, #34452 ) ;
#36886 = VERTEX_POINT ( 'NONE', #36064 ) ;
#36887 = CARTESIAN_POINT ( 'NONE',  ( 18.00000000000000355, 25.61928775981106554, -45.25098998563449726 ) ) ;
#36888 = DIRECTION ( 'NONE',  ( 0.000000000000000000, -0.7980172272802448230, 0.6026346363792494110 ) ) ;
#36890 = CARTESIAN_POINT ( 'NONE',  ( -21.03271207055027503, 40.00000000000000000, 3.044856699593507354 ) ) ;
#36889 = CARTESIAN_POINT ( 'NONE',  ( -153.1500000000000057, -5.251434100941175950E-13, 10.00000000000000000 ) ) ;
#36891 = DIRECTION ( 'NONE',  ( -1.000000000000000000, 0.000000000000000000, 0.000000000000000000 ) ) ;
#36892 = ORIENTED_EDGE ( 'NONE', *, *, #17637, .T. ) ;
#36893 = DIRECTION ( 'NONE',  ( 1.000000000000000000, 0.000000000000000000, 0.000000000000000000 ) ) ;
#36894 = CARTESIAN_POINT ( 'NONE',  ( 26.55430347651023837, 31.00000000000000355, -34.62409890758566178 ) ) ;
#36895 = EDGE_CURVE ( 'NONE', #2394, #41147, #40358, .T. ) ;
#36896 = ORIENTED_EDGE ( 'NONE', *, *, #22139, .T. ) ;
#36897 = DIRECTION ( 'NONE',  ( 1.000000000000000000, 0.000000000000000000, 0.000000000000000000 ) ) ;
#36898 = ADVANCED_FACE ( 'NONE', ( #19530 ), #12971, .F. ) ;
#36899 = CARTESIAN_POINT ( 'NONE',  ( 17.99999999999999645, 73.78980555658606022, 95.26571049922013401 ) ) ;
#36900 = ORIENTED_EDGE ( 'NONE', *, *, #16811, .T. ) ;
#36901 = CARTESIAN_POINT ( 'NONE',  ( 0.000000000000000000, 0.000000000000000000, 0.000000000000000000 ) ) ;
#36902 = CARTESIAN_POINT ( 'NONE',  ( -22.94860596549062848, 40.00000000000000000, -46.53072237555588231 ) ) ;
#36903 = CARTESIAN_POINT ( 'NONE',  ( 11.72132095739929625, 40.00000000000000000, -43.45763713125776917 ) ) ;
#36904 = AXIS2_PLACEMENT_3D ( 'NONE', #18766, #32025, #23294 ) ;
#36905 = AXIS2_PLACEMENT_3D ( 'NONE', #25069, #15443, #37870 ) ;
#36906 = ORIENTED_EDGE ( 'NONE', *, *, #4248, .F. ) ;
#36907 = DIRECTION ( 'NONE',  ( -1.000000000000000000, -0.000000000000000000, -0.000000000000000000 ) ) ;
#36908 = FACE_OUTER_BOUND ( 'NONE', #28720, .T. ) ;
#36909 = CIRCLE ( 'NONE', #35510, 59.00000000000000000 ) ;
#36910 = DIRECTION ( 'NONE',  ( -1.000000000000000000, -0.000000000000000000, -0.000000000000000000 ) ) ;
#36911 = EDGE_CURVE ( 'NONE', #31565, #16155, #28908, .T. ) ;
#36912 = VERTEX_POINT ( 'NONE', #20840 ) ;
#36913 = CARTESIAN_POINT ( 'NONE',  ( 22.42277067908921850, 40.00000000000000000, 12.94072372014797701 ) ) ;
#36914 = ORIENTED_EDGE ( 'NONE', *, *, #28225, .T. ) ;
#36915 = CARTESIAN_POINT ( 'NONE',  ( 0.000000000000000000, -59.47573314508800735, 99.59235496188593117 ) ) ;
#36916 = CARTESIAN_POINT ( 'NONE',  ( 0.000000000000000000, 44.61570720899096898, -14.73072383765582671 ) ) ;
#36917 = EDGE_LOOP ( 'NONE', ( #13557, #23204 ) ) ;
#36918 = CARTESIAN_POINT ( 'NONE',  ( 0.000000000000000000, 46.77034588191303754, 22.72740077717245910 ) ) ;
#36919 = CARTESIAN_POINT ( 'NONE',  ( 17.99999999999999645, -17.33727698085101565, -110.8498592715975519 ) ) ;
#36920 = VERTEX_POINT ( 'NONE', #3092 ) ;
#36921 = CYLINDRICAL_SURFACE ( 'NONE', #16564, 20.00000000000000355 ) ;
#36922 = ORIENTED_EDGE ( 'NONE', *, *, #15042, .T. ) ;
#36923 = LINE ( 'NONE', #10534, #22611 ) ;
#36924 = EDGE_CURVE ( 'NONE', #21205, #28718, #12524, .T. ) ;
#36925 = VERTEX_POINT ( 'NONE', #13618 ) ;
#36927 = VERTEX_POINT ( 'NONE', #26697 ) ;
#36926 = DIRECTION ( 'NONE',  ( -1.000000000000000000, -0.000000000000000000, -0.000000000000000000 ) ) ;
#36928 = CARTESIAN_POINT ( 'NONE',  ( 49.67886955982877595, 31.00000000000000355, -43.43868092391004865 ) ) ;
#36929 = EDGE_CURVE ( 'NONE', #38864, #22351, #36880, .T. ) ;
#36930 = ORIENTED_EDGE ( 'NONE', *, *, #17258, .T. ) ;
#36931 = CARTESIAN_POINT ( 'NONE',  ( 17.99999999999999645, 119.7318547011703629, -13.59315897125608430 ) ) ;
#36932 = ADVANCED_FACE ( 'NONE', ( #36483 ), #37140, .F. ) ;
#36933 = VERTEX_POINT ( 'NONE', #40611 ) ;
#36934 = CARTESIAN_POINT ( 'NONE',  ( -10.00000000000000000, 0.000000000000000000, 0.000000000000000000 ) ) ;
#36935 = ORIENTED_EDGE ( 'NONE', *, *, #40806, .F. ) ;
#36936 = CARTESIAN_POINT ( 'NONE',  ( 5.650912336215121456, 40.00000000000000000, -84.59266001511657862 ) ) ;
#36937 = VECTOR ( 'NONE', #34360, 1000.000000000000000 ) ;
#36938 = VECTOR ( 'NONE', #1516, 1000.000000000000000 ) ;
#36940 = CARTESIAN_POINT ( 'NONE',  ( 17.99999999999999645, 0.000000000000000000, 0.000000000000000000 ) ) ;
#36939 = CARTESIAN_POINT ( 'NONE',  ( -10.00000000000000000, 0.000000000000000000, 0.000000000000000000 ) ) ;
#36941 = AXIS2_PLACEMENT_3D ( 'NONE', #28149, #7838, #21196 ) ;
#36942 = FACE_OUTER_BOUND ( 'NONE', #8173, .T. ) ;
#36943 = ORIENTED_EDGE ( 'NONE', *, *, #4004, .F. ) ;
#36944 = CARTESIAN_POINT ( 'NONE',  ( 0.000000000000000000, 0.000000000000000000, 0.000000000000000000 ) ) ;
#36945 = ORIENTED_EDGE ( 'NONE', *, *, #33619, .T. ) ;
#36946 = CARTESIAN_POINT ( 'NONE',  ( 17.99999999999999645, -48.55277268144259040, -105.3500273609084843 ) ) ;
#36947 = CARTESIAN_POINT ( 'NONE',  ( 12.40854556226731198, -34.05525454449573175, -74.83297477053802993 ) ) ;
#36948 = EDGE_CURVE ( 'NONE', #26032, #41807, #11848, .T. ) ;
#36949 = CARTESIAN_POINT ( 'NONE',  ( 75.74279358916429317, 31.00000000000000000, -37.35102017232331661 ) ) ;
#36950 = EDGE_CURVE ( 'NONE', #21320, #22368, #1344, .T. ) ;
#36951 = CARTESIAN_POINT ( 'NONE',  ( 17.99999999999999645, 62.45178862086345362, -93.20969140437443912 ) ) ;
#36952 = VERTEX_POINT ( 'NONE', #3735 ) ;
#36953 = EDGE_CURVE ( 'NONE', #4169, #11582, #6600, .T. ) ;
#36954 = EDGE_CURVE ( 'NONE', #2814, #40741, #35479, .T. ) ;
#36955 = CARTESIAN_POINT ( 'NONE',  ( 17.99999999999999645, 97.19627249181095863, 71.22763238166520239 ) ) ;
#36956 = AXIS2_PLACEMENT_3D ( 'NONE', #15527, #29040, #25568 ) ;
#36957 = ORIENTED_EDGE ( 'NONE', *, *, #11710, .F. ) ;
#36958 = CARTESIAN_POINT ( 'NONE',  ( 1.411581201560190495E-15, 4.862606272033091592, -3.745885042887436622 ) ) ;
#36959 = DIRECTION ( 'NONE',  ( -1.000000000000000000, 0.000000000000000000, -0.000000000000000000 ) ) ;
#36960 = DIRECTION ( 'NONE',  ( 0.000000000000000000, 0.000000000000000000, -1.000000000000000000 ) ) ;
#36961 = CIRCLE ( 'NONE', #42526, 58.99999999999997868 ) ;
#36962 = ORIENTED_EDGE ( 'NONE', *, *, #27894, .F. ) ;
#36963 = DIRECTION ( 'NONE',  ( 1.000000000000000000, 0.000000000000000000, 0.000000000000000000 ) ) ;
#36964 = ORIENTED_EDGE ( 'NONE', *, *, #24852, .T. ) ;
#36965 = AXIS2_PLACEMENT_3D ( 'NONE', #24867, #18760, #8243 ) ;
#36966 = DIRECTION ( 'NONE',  ( -1.000000000000000000, -0.000000000000000000, -0.000000000000000000 ) ) ;
#36967 = CIRCLE ( 'NONE', #6322, 20.00000000000001066 ) ;
#36968 = CIRCLE ( 'NONE', #29338, 58.99999999999999289 ) ;
#36969 = DIRECTION ( 'NONE',  ( -1.000000000000000000, 3.469446951953615421E-17, 0.000000000000000000 ) ) ;
#36970 = AXIS2_PLACEMENT_3D ( 'NONE', #2766, #2338, #2565 ) ;
#36971 = LINE ( 'NONE', #30451, #22682 ) ;
#36972 = ORIENTED_EDGE ( 'NONE', *, *, #41992, .T. ) ;
#36973 = EDGE_LOOP ( 'NONE', ( #8535, #21856, #16006, #29927 ) ) ;
#36974 = CARTESIAN_POINT ( 'NONE',  ( 17.99999999999999645, 116.4607004671428570, 30.94182036827244531 ) ) ;
#36975 = DIRECTION ( 'NONE',  ( -1.000000000000000000, 0.000000000000000000, 0.000000000000000000 ) ) ;
#36976 = EDGE_CURVE ( 'NONE', #12248, #2530, #33237, .T. ) ;
#36977 = CARTESIAN_POINT ( 'NONE',  ( 4.000000000000000000, -1.677850389431204459, -3.535268758346977513 ) ) ;
#36979 = VERTEX_POINT ( 'NONE', #19969 ) ;
#36978 = DIRECTION ( 'NONE',  ( 0.000000000000000000, 0.000000000000000000, 1.000000000000000000 ) ) ;
#36980 = CARTESIAN_POINT ( 'NONE',  ( 35.58384423644163519, 31.00000000000000355, 12.14845634898874138 ) ) ;
#36981 = EDGE_CURVE ( 'NONE', #25282, #17781, #31331, .T. ) ;
#36982 = DIRECTION ( 'NONE',  ( -1.000000000000000000, -0.000000000000000000, -0.000000000000000000 ) ) ;
#36983 = AXIS2_PLACEMENT_3D ( 'NONE', #19712, #33417, #9853 ) ;
#36985 = ORIENTED_EDGE ( 'NONE', *, *, #36349, .F. ) ;
#36984 = DIRECTION ( 'NONE',  ( 0.000000000000000000, 0.000000000000000000, 1.000000000000000000 ) ) ;
#36986 = ORIENTED_EDGE ( 'NONE', *, *, #2752, .F. ) ;
#36987 = LINE ( 'NONE', #20451, #33088 ) ;
#36988 = CARTESIAN_POINT ( 'NONE',  ( 158.5000000000000284, 0.000000000000000000, 9.999999999999998224 ) ) ;
#36989 = CARTESIAN_POINT ( 'NONE',  ( -23.74678488968044832, 40.00000000000000000, -48.36925102894097961 ) ) ;
#36990 = LINE ( 'NONE', #98, #24218 ) ;
#36991 = PRODUCT_DEFINITION_CONTEXT ( 'detailed design', #25675, 'design' ) ;
#36992 = FACE_OUTER_BOUND ( 'NONE', #22258, .T. ) ;
#36993 = AXIS2_PLACEMENT_3D ( 'NONE', #12768, #26074, #28924 ) ;
#36994 = ORIENTED_EDGE ( 'NONE', *, *, #28593, .F. ) ;
#36995 = FACE_OUTER_BOUND ( 'NONE', #23853, .T. ) ;
#36996 = ORIENTED_EDGE ( 'NONE', *, *, #19701, .T. ) ;
#36997 = CIRCLE ( 'NONE', #14742, 5.560781378645573980 ) ;
#36998 = DIRECTION ( 'NONE',  ( 0.000000000000000000, 0.7705132427757903635, -0.6374239897486881912 ) ) ;
#36999 = DIRECTION ( 'NONE',  ( 0.000000000000000000, 1.000000000000000000, 0.000000000000000000 ) ) ;
#37000 = AXIS2_PLACEMENT_3D ( 'NONE', #31917, #1997, #5913 ) ;
#37001 = CARTESIAN_POINT ( 'NONE',  ( -4.090615425948576522, 31.00000000000000355, -62.39583333438447710 ) ) ;
#37002 = EDGE_CURVE ( 'NONE', #34548, #39812, #34807, .T. ) ;
#37003 = DIRECTION ( 'NONE',  ( 0.000000000000000000, 0.000000000000000000, 1.000000000000000000 ) ) ;
#37004 = ORIENTED_EDGE ( 'NONE', *, *, #22702, .F. ) ;
#37005 = EDGE_CURVE ( 'NONE', #34092, #12884, #3530, .T. ) ;
#37006 = EDGE_CURVE ( 'NONE', #28359, #19368, #23008, .T. ) ;
#37007 = AXIS2_PLACEMENT_3D ( 'NONE', #16737, #19788, #4016 ) ;
#37008 = ADVANCED_FACE ( 'NONE', ( #43039, #13192 ), #17117, .T. ) ;
#37009 = DIRECTION ( 'NONE',  ( 1.000000000000000000, 0.000000000000000000, 0.000000000000000000 ) ) ;
#37010 = ORIENTED_EDGE ( 'NONE', *, *, #13241, .T. ) ;
#37011 = CARTESIAN_POINT ( 'NONE',  ( 2.965790448435745574, 40.00000000000000000, -22.56328348808469997 ) ) ;
#37012 = AXIS2_PLACEMENT_3D ( 'NONE', #18818, #33777, #37051 ) ;
#37013 = VERTEX_POINT ( 'NONE', #26483 ) ;
#37014 = CARTESIAN_POINT ( 'NONE',  ( 0.000000000000000000, -27.79676263918213763, 37.88001506494759241 ) ) ;
#37015 = DIRECTION ( 'NONE',  ( 0.000000000000000000, 0.000000000000000000, 1.000000000000000000 ) ) ;
#37016 = CARTESIAN_POINT ( 'NONE',  ( 74.90833963775308746, 31.00000000000000000, 20.17845691862754975 ) ) ;
#37017 = CARTESIAN_POINT ( 'NONE',  ( 76.90008882636699639, 39.99999999999999289, -4.923574515426283327 ) ) ;
#37018 = EDGE_CURVE ( 'NONE', #3310, #252, #4137, .T. ) ;
#37019 = CARTESIAN_POINT ( 'NONE',  ( 0.000000000000000000, 0.000000000000000000, 0.000000000000000000 ) ) ;
#37020 = ORIENTED_EDGE ( 'NONE', *, *, #13430, .T. ) ;
#37021 = CARTESIAN_POINT ( 'NONE',  ( 9.000000000000001776, 51.93417535146740960, 2.615612846549358217 ) ) ;
#37022 = ORIENTED_EDGE ( 'NONE', *, *, #15054, .T. ) ;
#37023 = CARTESIAN_POINT ( 'NONE',  ( 17.99999999999999645, 0.000000000000000000, 0.000000000000000000 ) ) ;
#37024 = DIRECTION ( 'NONE',  ( 0.000000000000000000, 0.000000000000000000, 1.000000000000000000 ) ) ;
#37026 = EDGE_LOOP ( 'NONE', ( #9773, #2599 ) ) ;
#37025 = DIRECTION ( 'NONE',  ( -1.000000000000000000, 0.000000000000000000, 0.000000000000000000 ) ) ;
#37027 = CARTESIAN_POINT ( 'NONE',  ( 17.99999999999999645, -40.37724737310141165, 104.6802291180865865 ) ) ;
#37028 = ORIENTED_EDGE ( 'NONE', *, *, #8648, .F. ) ;
#37029 = CARTESIAN_POINT ( 'NONE',  ( 17.99999999999999645, -7.749090474611287860, -30.53094492177221397 ) ) ;
#37030 = CARTESIAN_POINT ( 'NONE',  ( 77.05880969081472642, 39.99999999999999289, 37.98468489477117771 ) ) ;
#37031 = FACE_OUTER_BOUND ( 'NONE', #16092, .T. ) ;
#37032 = VECTOR ( 'NONE', #37147, 1000.000000000000000 ) ;
#37033 =( REPRESENTATION_RELATIONSHIP ('NONE','NONE', #330, #18009 ) REPRESENTATION_RELATIONSHIP_WITH_TRANSFORMATION ( #7821 )SHAPE_REPRESENTATION_RELATIONSHIP( ) );
#37034 = CIRCLE ( 'NONE', #3592, 120.5010000000000190 ) ;
#37035 = ORIENTED_EDGE ( 'NONE', *, *, #5601, .T. ) ;
#37036 = DIRECTION ( 'NONE',  ( 1.000000000000000000, 0.000000000000000000, 0.000000000000000000 ) ) ;
#37037 = DIRECTION ( 'NONE',  ( -1.000000000000000000, 0.000000000000000000, 0.000000000000000000 ) ) ;
#37038 = AXIS2_PLACEMENT_3D ( 'NONE', #37727, #17497, #10926 ) ;
#37039 = EDGE_LOOP ( 'NONE', ( #20728, #420, #28024, #16422 ) ) ;
#37040 = ADVANCED_FACE ( 'NONE', ( #20606, #10757 ), #24091, .F. ) ;
#37041 = ORIENTED_EDGE ( 'NONE', *, *, #10034, .T. ) ;
#37042 = DIRECTION ( 'NONE',  ( -0.000000000000000000, -0.000000000000000000, 1.000000000000000000 ) ) ;
#37043 = ORIENTED_EDGE ( 'NONE', *, *, #20695, .T. ) ;
#37045 = CARTESIAN_POINT ( 'NONE',  ( 11.19416946702162718, 40.00000000000000000, -22.66942529387992522 ) ) ;
#37044 = CIRCLE ( 'NONE', #7078, 13.59999999999999787 ) ;
#37046 = CARTESIAN_POINT ( 'NONE',  ( -12.69999999999999929, 0.000000000000000000, 0.000000000000000000 ) ) ;
#37047 = CARTESIAN_POINT ( 'NONE',  ( 18.00000000000000355, 0.000000000000000000, 0.000000000000000000 ) ) ;
#37048 = DIRECTION ( 'NONE',  ( -1.000000000000000000, 0.000000000000000000, 0.000000000000000000 ) ) ;
#37049 = LINE ( 'NONE', #20512, #15140 ) ;
#37050 = ORIENTED_EDGE ( 'NONE', *, *, #2254, .F. ) ;
#37052 = DIRECTION ( 'NONE',  ( 0.000000000000000000, 0.000000000000000000, 1.000000000000000000 ) ) ;
#37051 = DIRECTION ( 'NONE',  ( 0.000000000000000000, 0.000000000000000000, -1.000000000000000000 ) ) ;
#37053 = ORIENTED_EDGE ( 'NONE', *, *, #4204, .T. ) ;
#37054 = FACE_OUTER_BOUND ( 'NONE', #28566, .T. ) ;
#37055 = CYLINDRICAL_SURFACE ( 'NONE', #3880, 120.5010000000000190 ) ;
#37056 = ORIENTED_EDGE ( 'NONE', *, *, #36976, .T. ) ;
#37057 = CYLINDRICAL_SURFACE ( 'NONE', #7863, 120.5010000000000190 ) ;
#37058 = ADVANCED_FACE ( 'NONE', ( #693 ), #7478, .F. ) ;
#37059 = CARTESIAN_POINT ( 'NONE',  ( 17.99999999999999645, 34.78944633786291973, -9.257128253673256424 ) ) ;
#37060 = EDGE_CURVE ( 'NONE', #3682, #9021, #21697, .T. ) ;
#37061 = CYLINDRICAL_SURFACE ( 'NONE', #5846, 2.649999999999971934 ) ;
#37062 = CIRCLE ( 'NONE', #41945, 20.00000000000000355 ) ;
#37063 = CARTESIAN_POINT ( 'NONE',  ( 65.10416666562252885, 31.00000000000000000, 4.254240043327690124 ) ) ;
#37064 = AXIS2_PLACEMENT_3D ( 'NONE', #19273, #12920, #41925 ) ;
#37065 = VECTOR ( 'NONE', #37124, 1000.000000000000000 ) ;
#37066 = ORIENTED_EDGE ( 'NONE', *, *, #22377, .T. ) ;
#37067 = CARTESIAN_POINT ( 'NONE',  ( 15.70068437845899290, 31.00000000000000355, 46.50252577710988078 ) ) ;
#37068 = CIRCLE ( 'NONE', #13429, 13.59999999999999787 ) ;
#37069 = CARTESIAN_POINT ( 'NONE',  ( -62.77658523491555798, 40.00000000000000711, 48.16944601536268777 ) ) ;
#37070 = ADVANCED_FACE ( 'NONE', ( #28007 ), #18822, .T. ) ;
#37071 = AXIS2_PLACEMENT_3D ( 'NONE', #38653, #8778, #35396 ) ;
#37072 = CARTESIAN_POINT ( 'NONE',  ( 17.99999999999999645, -108.8880088604273766, -39.99251838046071583 ) ) ;
#37073 = EDGE_CURVE ( 'NONE', #14824, #23300, #34952, .T. ) ;
#37074 = CARTESIAN_POINT ( 'NONE',  ( 11.90854556226686789, -14.05525454449572820, -74.83297477053821467 ) ) ;
#37075 = EDGE_LOOP ( 'NONE', ( #38891, #37053, #36690, #33871 ) ) ;
#37076 = DIRECTION ( 'NONE',  ( -1.000000000000000000, 0.000000000000000000, -0.000000000000000000 ) ) ;
#37077 = CARTESIAN_POINT ( 'NONE',  ( -109.0695705685741643, -106.4195705685773135, 9.999999999999753086 ) ) ;
#37078 = ORIENTED_EDGE ( 'NONE', *, *, #16474, .T. ) ;
#37079 = CARTESIAN_POINT ( 'NONE',  ( 13.71368254939966036, 40.00000000000000000, -51.22554439249349656 ) ) ;
#37080 = CARTESIAN_POINT ( 'NONE',  ( -4.943662031389838196E-16, -1.828353205453026285E-14, 6.938893903907228378E-15 ) ) ;
#37081 = DIRECTION ( 'NONE',  ( -1.000000000000000000, -0.000000000000000000, -0.000000000000000000 ) ) ;
#37082 = ORIENTED_EDGE ( 'NONE', *, *, #25283, .T. ) ;
#37083 = CARTESIAN_POINT ( 'NONE',  ( 17.99999999999999645, -101.8011932243944386, -55.61040422519432980 ) ) ;
#37084 = DIRECTION ( 'NONE',  ( 0.000000000000000000, 0.2113826236296184047, 0.9774033898178678959 ) ) ;
#37085 = VERTEX_POINT ( 'NONE', #11412 ) ;
#37086 = CARTESIAN_POINT ( 'NONE',  ( 17.99999999999999645, -16.77727049691090500, -27.19001440037564166 ) ) ;
#37087 = ORIENTED_EDGE ( 'NONE', *, *, #37600, .F. ) ;
#37088 = AXIS2_PLACEMENT_3D ( 'NONE', #1961, #24491, #8082 ) ;
#37089 = FACE_OUTER_BOUND ( 'NONE', #32674, .T. ) ;
#37090 = ORIENTED_EDGE ( 'NONE', *, *, #20397, .F. ) ;
#37091 = DIRECTION ( 'NONE',  ( -1.000000000000000000, -0.000000000000000000, 0.000000000000000000 ) ) ;
#37092 = AXIS2_PLACEMENT_3D ( 'NONE', #24729, #37986, #18841 ) ;
#37093 = CARTESIAN_POINT ( 'NONE',  ( 18.00000000000000355, 36.06787431788731624, -37.45808914225448660 ) ) ;
#37094 = ORIENTED_EDGE ( 'NONE', *, *, #21503, .T. ) ;
#37095 = AXIS2_PLACEMENT_3D ( 'NONE', #15458, #22011, #41603 ) ;
#37096 = DIRECTION ( 'NONE',  ( 1.000000000000000000, -1.373900992973641868E-15, -3.994789077170585140E-16 ) ) ;
#37097 = DIRECTION ( 'NONE',  ( -1.000000000000000000, -0.000000000000000000, 0.000000000000000000 ) ) ;
#37098 = EDGE_LOOP ( 'NONE', ( #23289, #35933, #24325, #14416 ) ) ;
#37099 = DIRECTION ( 'NONE',  ( 0.000000000000000000, -0.7865515558026355825, -0.6175246149462008116 ) ) ;
#37100 = CIRCLE ( 'NONE', #12043, 59.00000000000000711 ) ;
#37101 = DIRECTION ( 'NONE',  ( -1.000000000000000000, 0.000000000000000000, -0.000000000000000000 ) ) ;
#37103 = CARTESIAN_POINT ( 'NONE',  ( 0.000000000000000000, 120.4984140710909202, 0.7894348306988416830 ) ) ;
#37102 = CARTESIAN_POINT ( 'NONE',  ( 17.99999999999999645, 0.000000000000000000, 0.000000000000000000 ) ) ;
#37104 = EDGE_CURVE ( 'NONE', #24364, #34048, #43134, .T. ) ;
#37105 = PLANE ( 'NONE',  #38145 ) ;
#37106 = ADVANCED_FACE ( 'NONE', ( #31481 ), #1569, .F. ) ;
#37107 = ORIENTED_EDGE ( 'NONE', *, *, #20866, .T. ) ;
#37108 = DIRECTION ( 'NONE',  ( -0.7071067811865536790, 0.000000000000000000, -0.7071067811865413555 ) ) ;
#37109 = DIRECTION ( 'NONE',  ( -1.000000000000000000, -0.000000000000000000, 0.000000000000000000 ) ) ;
#37110 = CARTESIAN_POINT ( 'NONE',  ( 42.20483333784007840, 31.00000000000000355, -14.33818270462009359 ) ) ;
#37111 = ORIENTED_EDGE ( 'NONE', *, *, #9173, .T. ) ;
#37112 = CYLINDRICAL_SURFACE ( 'NONE', #987, 13.59999999999999964 ) ;
#37113 = DIRECTION ( 'NONE',  ( -1.000000000000000000, 0.000000000000000000, 0.000000000000000000 ) ) ;
#37114 = EDGE_LOOP ( 'NONE', ( #36725, #14956, #5916, #8030 ) ) ;
#37115 = FACE_OUTER_BOUND ( 'NONE', #22205, .T. ) ;
#37116 = CARTESIAN_POINT ( 'NONE',  ( 17.07784400123870938, 40.00000000000000000, -50.31546185293520779 ) ) ;
#37117 = CARTESIAN_POINT ( 'NONE',  ( 24.31498657911848227, 40.00000000000000000, 42.27453502171530175 ) ) ;
#37118 = ADVANCED_FACE ( 'NONE', ( #21268 ), #34745, .T. ) ;
#37119 = VECTOR ( 'NONE', #21401, 1000.000000000000000 ) ;
#37120 = ORIENTED_EDGE ( 'NONE', *, *, #11073, .T. ) ;
#37121 = FACE_OUTER_BOUND ( 'NONE', #36219, .T. ) ;
#37122 = ADVANCED_FACE ( 'NONE', ( #40837 ), #7687, .F. ) ;
#37123 = DIRECTION ( 'NONE',  ( -1.000000000000000000, -0.000000000000000000, 0.000000000000000000 ) ) ;
#37124 = DIRECTION ( 'NONE',  ( 1.000000000000000000, -0.000000000000000000, 0.000000000000000000 ) ) ;
#37125 = VERTEX_POINT ( 'NONE', #24750 ) ;
#37126 = CARTESIAN_POINT ( 'NONE',  ( 1.799870782497353439, 40.00000000000000000, 27.39583333577991908 ) ) ;
#37127 = ORIENTED_EDGE ( 'NONE', *, *, #13539, .F. ) ;
#37128 = DIRECTION ( 'NONE',  ( -1.000000000000000000, -0.000000000000000000, -0.000000000000000000 ) ) ;
#37129 = DIRECTION ( 'NONE',  ( -1.000000000000000000, -0.000000000000000000, -0.000000000000000000 ) ) ;
#37130 = EDGE_LOOP ( 'NONE', ( #27396, #18151, #32289, #11089 ) ) ;
#37131 = CARTESIAN_POINT ( 'NONE',  ( 0.000000000000000000, 0.000000000000000000, 0.000000000000000000 ) ) ;
#37132 = CARTESIAN_POINT ( 'NONE',  ( 17.99999999999999645, -99.97660604680010010, 67.26937820704857529 ) ) ;
#37133 = VERTEX_POINT ( 'NONE', #8549 ) ;
#37134 = CARTESIAN_POINT ( 'NONE',  ( 0.000000000000000000, 0.000000000000000000, 0.000000000000000000 ) ) ;
#37135 = VERTEX_POINT ( 'NONE', #38225 ) ;
#37136 = CARTESIAN_POINT ( 'NONE',  ( 0.000000000000000000, 112.8457601792519256, -26.86697618949260402 ) ) ;
#37137 = EDGE_CURVE ( 'NONE', #35367, #11424, #29245, .T. ) ;
#37138 = EDGE_CURVE ( 'NONE', #36558, #9440, #13243, .T. ) ;
#37139 = ORIENTED_EDGE ( 'NONE', *, *, #34171, .F. ) ;
#37141 = ORIENTED_EDGE ( 'NONE', *, *, #5491, .T. ) ;
#37140 = CYLINDRICAL_SURFACE ( 'NONE', #30649, 59.00000000000000000 ) ;
#37142 = CARTESIAN_POINT ( 'NONE',  ( 40.05902963217418744, 31.00000000000000355, -52.04757428483648596 ) ) ;
#37144 = ADVANCED_FACE ( 'NONE', ( #4182 ), #30833, .T. ) ;
#37143 = VERTEX_POINT ( 'NONE', #34096 ) ;
#37145 = DIRECTION ( 'NONE',  ( 0.000000000000000000, 0.9826841245925201918, 0.1852887240871181063 ) ) ;
#37146 = ORIENTED_EDGE ( 'NONE', *, *, #25524, .F. ) ;
#37147 = DIRECTION ( 'NONE',  ( -1.000000000000000000, 0.000000000000000000, 0.000000000000000000 ) ) ;
#37148 = VERTEX_POINT ( 'NONE', #4853 ) ;
#37149 = AXIS2_PLACEMENT_3D ( 'NONE', #28519, #41569, #8410 ) ;
#37150 = CARTESIAN_POINT ( 'NONE',  ( 22.12670472277728706, 40.00000000000000000, -82.16725659058069198 ) ) ;
#37152 = DIRECTION ( 'NONE',  ( 0.000000000000000000, -0.9826841245925190815, -0.1852887240871243235 ) ) ;
#37151 = DIRECTION ( 'NONE',  ( 0.000000000000000000, 0.000000000000000000, 1.000000000000000000 ) ) ;
#37153 = CARTESIAN_POINT ( 'NONE',  ( -10.00000000000000000, 0.000000000000000000, 0.000000000000000000 ) ) ;
#37154 = ORIENTED_EDGE ( 'NONE', *, *, #37278, .F. ) ;
#37155 = CARTESIAN_POINT ( 'NONE',  ( 9.000000000000000000, -32.49609705003715732, 15.49205204337262920 ) ) ;
#37156 =( GEOMETRIC_REPRESENTATION_CONTEXT ( 3 ) GLOBAL_UNCERTAINTY_ASSIGNED_CONTEXT ( ( #15949 ) ) GLOBAL_UNIT_ASSIGNED_CONTEXT ( ( #20629, #7709, #711 ) ) REPRESENTATION_CONTEXT ( 'NONE', 'WORKASPACE' ) );
#37157 = EDGE_CURVE ( 'NONE', #42604, #11582, #25799, .T. ) ;
#37158 = VERTEX_POINT ( 'NONE', #17772 ) ;
#37159 = LINE ( 'NONE', #14073, #40771 ) ;
#37160 = CIRCLE ( 'NONE', #22567, 120.5010000000000474 ) ;
#37161 = CARTESIAN_POINT ( 'NONE',  ( 18.00000000000000355, 46.90537658765334328, -2.727856614653797251 ) ) ;
#37162 = CARTESIAN_POINT ( 'NONE',  ( -12.08748825390017068, 31.00000000000000355, -91.69541640458645304 ) ) ;
#37163 = CARTESIAN_POINT ( 'NONE',  ( 1.390230914382191596, 4.043987460488659202, -3.502507215260488582 ) ) ;
#37164 = EDGE_LOOP ( 'NONE', ( #31516, #15546, #22947, #39951 ) ) ;
#37165 = AXIS2_PLACEMENT_3D ( 'NONE', #21000, #30779, #34252 ) ;
#37166 = CARTESIAN_POINT ( 'NONE',  ( 17.99999999999999645, -93.26762629039475883, 76.29967815892324268 ) ) ;
#37167 = EDGE_CURVE ( 'NONE', #20374, #3430, #28219, .T. ) ;
#37168 = ORIENTED_EDGE ( 'NONE', *, *, #25467, .F. ) ;
#37169 =( NAMED_UNIT ( * ) SI_UNIT ( $, .STERADIAN. ) SOLID_ANGLE_UNIT ( ) );
#37170 = EDGE_CURVE ( 'NONE', #22504, #28053, #16047, .T. ) ;
#37171 = DIRECTION ( 'NONE',  ( -1.000000000000000000, -0.000000000000000000, -0.000000000000000000 ) ) ;
#37172 = CARTESIAN_POINT ( 'NONE',  ( 17.99999999999999645, 57.69704296431184787, 105.7900857083231472 ) ) ;
#37173 = AXIS2_PLACEMENT_3D ( 'NONE', #38609, #42091, #8730 ) ;
#37174 = EDGE_CURVE ( 'NONE', #32990, #21041, #42477, .T. ) ;
#37175 =( BOUNDED_SURFACE ( )  B_SPLINE_SURFACE ( 3, 2, ( 
 ( #9514, #22867, #39598 ),
 ( #4019, #36977, #744 ),
 ( #37407, #20890, #297 ),
 ( #27395, #40661, #14104 ),
 ( #21102, #7087, #10377 ),
 ( #27620, #23713, #34355 ) ),
 .UNSPECIFIED., .F., .F., .F. ) 
 B_SPLINE_SURFACE_WITH_KNOTS ( ( 4, 2, 4 ),
 ( 3, 3 ),
 ( 0.02027065861071770947, 0.02273072267836921331, 0.02519078674602071716 ),
 ( 0.000000000000000000, 1.000000000000000000 ),
 .UNSPECIFIED. ) 
 GEOMETRIC_REPRESENTATION_ITEM ( )  RATIONAL_B_SPLINE_SURFACE ( (
 ( 1.000000000000000000, 0.8047781708337304885, 1.000000000000000000),
 ( 1.000000000000000000, 0.8123765190705307671, 1.000000000000000000),
 ( 1.000000000000000000, 0.8190656277163975707, 1.000000000000000000),
 ( 1.000000000000000000, 0.8192366903512159348, 1.000000000000000000),
 ( 1.000000000000000000, 0.8126138454302893610, 1.000000000000000000),
 ( 1.000000000000000000, 0.8047712246031417660, 1.000000000000000000) ) ) 
 REPRESENTATION_ITEM ( '' )  SURFACE ( )  );
#37176 = DIRECTION ( 'NONE',  ( 0.000000000000000000, 0.000000000000000000, 1.000000000000000000 ) ) ;
#37177 = CIRCLE ( 'NONE', #7215, 10.49999999999999467 ) ;
#37178 = ORIENTED_EDGE ( 'NONE', *, *, #18891, .F. ) ;
#37179 = DIRECTION ( 'NONE',  ( 0.000000000000000000, -0.1253332335642905471, -0.9921147013144795412 ) ) ;
#37180 = ORIENTED_EDGE ( 'NONE', *, *, #26445, .T. ) ;
#37181 = DIRECTION ( 'NONE',  ( 0.000000000000000000, 0.000000000000000000, 1.000000000000000000 ) ) ;
#37182 = CARTESIAN_POINT ( 'NONE',  ( -10.00000000000000000, 0.000000000000000000, 0.000000000000000000 ) ) ;
#37183 = DIRECTION ( 'NONE',  ( 0.000000000000000000, 0.9407002666710341243, -0.3392388661180279485 ) ) ;
#37184 = VERTEX_POINT ( 'NONE', #11637 ) ;
#37185 = VERTEX_POINT ( 'NONE', #8342 ) ;
#37186 = CARTESIAN_POINT ( 'NONE',  ( 0.000000000000000000, -47.58001226230464908, -110.7096808509488284 ) ) ;
#37187 = DIRECTION ( 'NONE',  ( -3.996523416598930318E-16, 2.658563593772947863E-15, 1.000000000000000000 ) ) ;
#37188 = DIRECTION ( 'NONE',  ( 1.058513553088275437E-16, 1.000000000000000000, -8.813324511995299047E-17 ) ) ;
#37189 = AXIS2_PLACEMENT_3D ( 'NONE', #9703, #6852, #29567 ) ;
#37191 = ORIENTED_EDGE ( 'NONE', *, *, #17270, .F. ) ;
#37190 = DIRECTION ( 'NONE',  ( -1.000000000000000000, 0.000000000000000000, 0.000000000000000000 ) ) ;
#37192 = CARTESIAN_POINT ( 'NONE',  ( 23.59836588145513048, 31.00000000000000355, -26.81698947917456266 ) ) ;
#37193 = EDGE_CURVE ( 'NONE', #25554, #6179, #8764, .T. ) ;
#37194 = CYLINDRICAL_SURFACE ( 'NONE', #8393, 59.00000000000000000 ) ;
#37195 = EDGE_CURVE ( 'NONE', #11794, #8918, #36909, .T. ) ;
#37196 = AXIS2_PLACEMENT_3D ( 'NONE', #2349, #41663, #19013 ) ;
#37198 = ORIENTED_EDGE ( 'NONE', *, *, #27345, .F. ) ;
#37197 = DIRECTION ( 'NONE',  ( 1.000000000000000000, 0.000000000000000000, 0.000000000000000000 ) ) ;
#37199 = ORIENTED_EDGE ( 'NONE', *, *, #34966, .T. ) ;
#37200 = DIRECTION ( 'NONE',  ( 0.000000000000000000, 1.000000000000000000, -1.060184893785364939E-15 ) ) ;
#37201 = CARTESIAN_POINT ( 'NONE',  ( -38.36856355434107968, 40.00000000000000000, 33.53830235993100217 ) ) ;
#37202 = AXIS2_PLACEMENT_3D ( 'NONE', #522, #37395, #68 ) ;
#37203 = DIRECTION ( 'NONE',  ( -1.000000000000000000, 0.000000000000000000, -0.000000000000000000 ) ) ;
#37204 = AXIS2_PLACEMENT_3D ( 'NONE', #42310, #19877, #42520 ) ;
#37205 = CARTESIAN_POINT ( 'NONE',  ( 0.000000000000000000, 0.000000000000000000, -1.199999999999999956 ) ) ;
#37206 = VERTEX_POINT ( 'NONE', #22333 ) ;
#37207 = CARTESIAN_POINT ( 'NONE',  ( 0.000000000000000000, 6.109652351742432153, -46.58570277113501845 ) ) ;
#37208 = EDGE_CURVE ( 'NONE', #41141, #1487, #8364, .T. ) ;
#37209 = VERTEX_POINT ( 'NONE', #32319 ) ;
#37210 = CIRCLE ( 'NONE', #7938, 13.59999999999999964 ) ;
#37211 = DIRECTION ( 'NONE',  ( 0.000000000000000000, 0.000000000000000000, 1.000000000000000000 ) ) ;
#37212 = DIRECTION ( 'NONE',  ( -1.000000000000000000, 0.000000000000000000, -0.000000000000000000 ) ) ;
#37213 = CARTESIAN_POINT ( 'NONE',  ( -51.34291522965900612, 31.00000000000000355, 29.65708359768123970 ) ) ;
#37214 = DIRECTION ( 'NONE',  ( 0.000000000000000000, 0.7525707698561399095, -0.6585113790650372056 ) ) ;
#37215 = ORIENTED_EDGE ( 'NONE', *, *, #28737, .F. ) ;
#37216 = AXIS2_PLACEMENT_3D ( 'NONE', #10289, #13369, #29298 ) ;
#37217 = DIRECTION ( 'NONE',  ( 0.000000000000000000, 0.9213119778704139673, -0.3888241754733182676 ) ) ;
#37218 = ORIENTED_EDGE ( 'NONE', *, *, #31626, .F. ) ;
#37219 = ADVANCED_FACE ( 'NONE', ( #9398 ), #42547, .T. ) ;
#37220 = CARTESIAN_POINT ( 'NONE',  ( -60.10374203099167545, 31.00000000000000711, 78.35501831527777483 ) ) ;
#37221 = ORIENTED_EDGE ( 'NONE', *, *, #38068, .F. ) ;
#37222 = CARTESIAN_POINT ( 'NONE',  ( 8.999999999999998224, -0.6168405712489253290, 35.99471499692226217 ) ) ;
#37223 = EDGE_CURVE ( 'NONE', #4344, #32776, #21654, .T. ) ;
#37224 = DIRECTION ( 'NONE',  ( -1.000000000000000000, 0.000000000000000000, 0.000000000000000000 ) ) ;
#37225 = CARTESIAN_POINT ( 'NONE',  ( -23.73339997550686675, 31.00000000000000355, -70.23208777904191891 ) ) ;
#37226 = CARTESIAN_POINT ( 'NONE',  ( -44.72205690102931896, 40.00000000000000000, -58.47036224960022111 ) ) ;
#37227 = CARTESIAN_POINT ( 'NONE',  ( 18.00000000000000355, 19.44205635905542096, 43.33776004284615624 ) ) ;
#37228 = AXIS2_PLACEMENT_3D ( 'NONE', #18535, #41378, #28759 ) ;
#37229 = VECTOR ( 'NONE', #12231, 1000.000000000000000 ) ;
#37230 = ORIENTED_EDGE ( 'NONE', *, *, #21172, .F. ) ;
#37231 = CARTESIAN_POINT ( 'NONE',  ( 0.000000000000000000, 0.000000000000000000, 0.000000000000000000 ) ) ;
#37232 = VERTEX_POINT ( 'NONE', #32536 ) ;
#37233 = FILL_AREA_STYLE ('',( #10634 ) ) ;
#37234 = CIRCLE ( 'NONE', #7997, 116.0000000000000000 ) ;
#37235 = FACE_OUTER_BOUND ( 'NONE', #42484, .T. ) ;
#37236 = VECTOR ( 'NONE', #30109, 1000.000000000000000 ) ;
#37238 = ORIENTED_EDGE ( 'NONE', *, *, #12080, .F. ) ;
#37237 = DIRECTION ( 'NONE',  ( 0.000000000000000000, -0.9510565162951500895, -0.3090169943749581649 ) ) ;
#37239 = CARTESIAN_POINT ( 'NONE',  ( 18.00000000000000355, 35.20873326984126805, -31.88259874183992792 ) ) ;
#37240 = VERTEX_POINT ( 'NONE', #26004 ) ;
#37241 = CYLINDRICAL_SURFACE ( 'NONE', #3504, 7.500000000000000000 ) ;
#37242 = CIRCLE ( 'NONE', #5880, 120.5010000000000474 ) ;
#37243 = CARTESIAN_POINT ( 'NONE',  ( -53.76583044639610165, 40.00000000000000000, -61.28633540801820345 ) ) ;
#37244 = CARTESIAN_POINT ( 'NONE',  ( -0.3208286057739654917, 4.433571671609680465, -0.3503314178412548774 ) ) ;
#37245 = EDGE_LOOP ( 'NONE', ( #30466, #10721, #35458, #27324 ) ) ;
#37246 = ADVANCED_FACE ( 'NONE', ( #36007 ), #29489, .F. ) ;
#37247 = CARTESIAN_POINT ( 'NONE',  ( 17.99999999999999645, 108.8684555192050425, -27.12806418649509865 ) ) ;
#37248 = EDGE_CURVE ( 'NONE', #11164, #20981, #29274, .T. ) ;
#37249 = DIRECTION ( 'NONE',  ( 0.000000000000000000, -7.709882115452471264E-16, -1.000000000000000000 ) ) ;
#37250 = ADVANCED_FACE ( 'NONE', ( #25807 ), #21906, .F. ) ;
#37251 = EDGE_CURVE ( 'NONE', #20139, #10415, #35581, .T. ) ;
#37252 = ORIENTED_EDGE ( 'NONE', *, *, #42296, .F. ) ;
#37253 = VECTOR ( 'NONE', #7059, 1000.000000000000000 ) ;
#37254 = VERTEX_POINT ( 'NONE', #39065 ) ;
#37255 = DIRECTION ( 'NONE',  ( -1.000000000000000000, -0.000000000000000000, -0.000000000000000000 ) ) ;
#37256 = VERTEX_POINT ( 'NONE', #8982 ) ;
#37257 = DIRECTION ( 'NONE',  ( -1.000000000000000000, -0.000000000000000000, 0.000000000000000000 ) ) ;
#37258 = CARTESIAN_POINT ( 'NONE',  ( 0.000000000000000000, -7.220349212960190499, -35.26849241522671718 ) ) ;
#37259 = CARTESIAN_POINT ( 'NONE',  ( 17.99999999999999645, 48.55277268144325120, 105.3500273609081432 ) ) ;
#37260 = AXIS2_PLACEMENT_3D ( 'NONE', #27850, #24377, #37631 ) ;
#37261 = FACE_OUTER_BOUND ( 'NONE', #34084, .T. ) ;
#37262 = ORIENTED_EDGE ( 'NONE', *, *, #10873, .F. ) ;
#37264 = CARTESIAN_POINT ( 'NONE',  ( 9.000000000000001776, -24.47917365149914559, -45.87777302070959706 ) ) ;
#37263 = CARTESIAN_POINT ( 'NONE',  ( 6.200000000000001066, -18.77999999999998337, 2.299886688798728323E-15 ) ) ;
#37265 = CIRCLE ( 'NONE', #35176, 116.0000000000000000 ) ;
#37266 = ORIENTED_EDGE ( 'NONE', *, *, #14062, .F. ) ;
#37267 = AXIS2_PLACEMENT_3D ( 'NONE', #24673, #37931, #8048 ) ;
#37268 = DIRECTION ( 'NONE',  ( -0.000000000000000000, 5.297542245118643184E-16, 1.000000000000000000 ) ) ;
#37269 = CARTESIAN_POINT ( 'NONE',  ( -21.73352778766994575, 31.00000000000000355, 19.07242603999910457 ) ) ;
#37270 = ORIENTED_EDGE ( 'NONE', *, *, #12855, .T. ) ;
#37271 = LINE ( 'NONE', #7387, #14155 ) ;
#37272 = DIRECTION ( 'NONE',  ( 3.996523416598993920E-16, 2.658563593772947074E-15, 1.000000000000000000 ) ) ;
#37274 = AXIS2_PLACEMENT_3D ( 'NONE', #41808, #22862, #35886 ) ;
#37273 = DIRECTION ( 'NONE',  ( 0.000000000000000000, 0.000000000000000000, 1.000000000000000000 ) ) ;
#37275 = CARTESIAN_POINT ( 'NONE',  ( 72.19657831791809599, 31.00000000000000000, -19.34484491892447622 ) ) ;
#37276 = VERTEX_POINT ( 'NONE', #38642 ) ;
#37277 = CARTESIAN_POINT ( 'NONE',  ( -6.590854309045712789, 31.00000000000000355, 49.37518673228670707 ) ) ;
#37278 = EDGE_CURVE ( 'NONE', #29277, #31219, #14656, .T. ) ;
#37279 = CARTESIAN_POINT ( 'NONE',  ( 75.74279358916429317, 39.99999999999999289, -37.35102017232331661 ) ) ;
#37280 = CARTESIAN_POINT ( 'NONE',  ( 0.000000000000000000, 0.000000000000000000, 0.000000000000000000 ) ) ;
#37281 = CARTESIAN_POINT ( 'NONE',  ( 0.000000000000000000, -13.57797752207901532, -33.34124362422488730 ) ) ;
#37282 = CARTESIAN_POINT ( 'NONE',  ( -6.199999999999993960, -18.77999999999999048, 2.299886688798728717E-15 ) ) ;
#37283 = AXIS2_PLACEMENT_3D ( 'NONE', #17186, #17626, #30891 ) ;
#37284 = AXIS2_PLACEMENT_3D ( 'NONE', #30583, #37313, #7428 ) ;
#37286 = ORIENTED_EDGE ( 'NONE', *, *, #12100, .F. ) ;
#37285 = DIRECTION ( 'NONE',  ( 1.000000000000000000, 0.000000000000000000, 0.000000000000000000 ) ) ;
#37287 = AXIS2_PLACEMENT_3D ( 'NONE', #38836, #32509, #42522 ) ;
#37288 = DIRECTION ( 'NONE',  ( 1.000000000000000000, -0.000000000000000000, -0.000000000000000000 ) ) ;
#37289 = CIRCLE ( 'NONE', #9454, 20.00000000000001066 ) ;
#37290 = DIRECTION ( 'NONE',  ( 0.000000000000000000, 0.2113826236296247885, -0.9774033898178665636 ) ) ;
#37291 = CIRCLE ( 'NONE', #10133, 139.4999999999992610 ) ;
#37292 = EDGE_LOOP ( 'NONE', ( #28010, #18525 ) ) ;
#37293 = CARTESIAN_POINT ( 'NONE',  ( -53.27196957865878346, 40.00000000000000711, 26.27224001323269320 ) ) ;
#37294 = CARTESIAN_POINT ( 'NONE',  ( 0.000000000000000000, -107.1354928292866759, -44.47455650398174498 ) ) ;
#37295 = CARTESIAN_POINT ( 'NONE',  ( 4.000000000000000888, 1.563622288139206118, -0.2253451193528334950 ) ) ;
#37296 = AXIS2_PLACEMENT_3D ( 'NONE', #27815, #713, #13638 ) ;
#37297 = EDGE_LOOP ( 'NONE', ( #31205, #38611, #10163, #23963 ) ) ;
#37298 = AXIS2_PLACEMENT_3D ( 'NONE', #6682, #20045, #33081 ) ;
#37299 = DIRECTION ( 'NONE',  ( 1.000000000000000000, 0.000000000000000000, 0.000000000000000000 ) ) ;
#37300 = DIRECTION ( 'NONE',  ( -3.009274222672345096E-17, -1.000000000000000000, 2.455023325076454960E-18 ) ) ;
#37301 = CIRCLE ( 'NONE', #39369, 15.99999999999998579 ) ;
#37302 = EDGE_CURVE ( 'NONE', #2224, #15863, #40386, .T. ) ;
#37303 = ADVANCED_FACE ( 'NONE', ( #12913 ), #22543, .F. ) ;
#37304 = ORIENTED_EDGE ( 'NONE', *, *, #30000, .F. ) ;
#37305 = PLANE ( 'NONE',  #18025 ) ;
#37306 = ORIENTED_EDGE ( 'NONE', *, *, #16732, .T. ) ;
#37307 = ADVANCED_FACE ( 'NONE', ( #5279 ), #28852, .T. ) ;
#37308 = CARTESIAN_POINT ( 'NONE',  ( 17.99999999999999645, 35.72777019205667415, 106.3569410558018404 ) ) ;
#37309 = ORIENTED_EDGE ( 'NONE', *, *, #16441, .T. ) ;
#37310 = CARTESIAN_POINT ( 'NONE',  ( 0.000000000000000000, 59.07817985939141181, -105.0250430397503294 ) ) ;
#37311 = CARTESIAN_POINT ( 'NONE',  ( -13.16936484334534008, 31.00000000000000355, 99.04657264463375554 ) ) ;
#37312 = ORIENTED_EDGE ( 'NONE', *, *, #36191, .F. ) ;
#37313 = DIRECTION ( 'NONE',  ( -1.000000000000000000, -0.000000000000000000, -0.000000000000000000 ) ) ;
#37314 = DIRECTION ( 'NONE',  ( -1.000000000000000000, -0.000000000000000000, 0.000000000000000000 ) ) ;
#37315 = ORIENTED_EDGE ( 'NONE', *, *, #11635, .T. ) ;
#37316 = CARTESIAN_POINT ( 'NONE',  ( 0.000000000000000000, 116.4607004671428570, 30.94182036827243465 ) ) ;
#37317 = CYLINDRICAL_SURFACE ( 'NONE', #33160, 13.59999999999999787 ) ;
#37318 = EDGE_CURVE ( 'NONE', #25294, #27015, #32737, .T. ) ;
#37319 = CIRCLE ( 'NONE', #30359, 116.0000000000000000 ) ;
#37320 = LINE ( 'NONE', #19921, #41267 ) ;
#37321 = CARTESIAN_POINT ( 'NONE',  ( 9.000000000000001776, -35.78484819117709748, 110.3423972910431701 ) ) ;
#37322 = AXIS2_PLACEMENT_3D ( 'NONE', #1027, #27913, #10446 ) ;
#37323 = ORIENTED_EDGE ( 'NONE', *, *, #14553, .F. ) ;
#37324 = VECTOR ( 'NONE', #14134, 1000.000000000000000 ) ;
#37325 = DIRECTION ( 'NONE',  ( -0.9860591398701278321, 2.926471934477876410E-17, -0.1663952303360400065 ) ) ;
#37326 = CARTESIAN_POINT ( 'NONE',  ( 17.99999999999999645, -109.3506818544107659, -38.70953859161124910 ) ) ;
#37327 = CARTESIAN_POINT ( 'NONE',  ( -38.31599561464027914, 31.00000000000000355, 10.26995502114586678 ) ) ;
#37328 = EDGE_LOOP ( 'NONE', ( #34770, #32433, #4707, #3328 ) ) ;
#37329 = CARTESIAN_POINT ( 'NONE',  ( 18.00000000000000355, 42.03146605346785947, 22.12489237027331512 ) ) ;
#37330 = DIRECTION ( 'NONE',  ( -1.000000000000000000, -0.000000000000000000, -0.000000000000000000 ) ) ;
#37331 = ORIENTED_EDGE ( 'NONE', *, *, #20791, .T. ) ;
#37332 = VECTOR ( 'NONE', #5532, 1000.000000000000000 ) ;
#37333 = AXIS2_PLACEMENT_3D ( 'NONE', #16867, #3695, #17074 ) ;
#37334 = CARTESIAN_POINT ( 'NONE',  ( 17.99999999999999645, 51.27532863109503580, -99.79535634195073612 ) ) ;
#37335 = CARTESIAN_POINT ( 'NONE',  ( 36.61186797162192619, 40.00000000000000000, 28.07927795628900469 ) ) ;
#37336 = CARTESIAN_POINT ( 'NONE',  ( 42.13926417418816328, 40.00000000000000000, -36.83769365845790134 ) ) ;
#37337 = CIRCLE ( 'NONE', #18592, 59.00000000000000000 ) ;
#37338 = FACE_OUTER_BOUND ( 'NONE', #26131, .T. ) ;
#37339 = CARTESIAN_POINT ( 'NONE',  ( 17.99999999999999645, 5.456439917444967591, 112.0647122740742105 ) ) ;
#37340 = LINE ( 'NONE', #33043, #20656 ) ;
#37341 = FACE_OUTER_BOUND ( 'NONE', #8498, .T. ) ;
#37342 = ORIENTED_EDGE ( 'NONE', *, *, #35530, .T. ) ;
#37343 = CARTESIAN_POINT ( 'NONE',  ( -23.02120395722396395, 40.00000000000000000, 17.66995642160909696 ) ) ;
#37344 = VERTEX_POINT ( 'NONE', #5910 ) ;
#37345 = CARTESIAN_POINT ( 'NONE',  ( 18.00000000000000355, -45.78515115856033901, -12.64416602183713856 ) ) ;
#37346 = LINE ( 'NONE', #469, #36736 ) ;
#37347 = ORIENTED_EDGE ( 'NONE', *, *, #28168, .T. ) ;
#37348 = AXIS2_PLACEMENT_3D ( 'NONE', #30105, #15569, #29900 ) ;
#37349 = DIRECTION ( 'NONE',  ( -1.000000000000000000, 0.000000000000000000, 0.000000000000000000 ) ) ;
#37350 = EDGE_CURVE ( 'NONE', #20569, #40464, #19263, .T. ) ;
#37351 = FACE_OUTER_BOUND ( 'NONE', #43078, .T. ) ;
#37352 = ORIENTED_EDGE ( 'NONE', *, *, #30376, .T. ) ;
#37353 = CARTESIAN_POINT ( 'NONE',  ( 17.99999999999999645, 29.36437154451999021, 116.8684075565137164 ) ) ;
#37354 = CIRCLE ( 'NONE', #14402, 11.08000000000000007 ) ;
#37355 = EDGE_LOOP ( 'NONE', ( #25816, #32597, #26424, #11506 ) ) ;
#37356 = VECTOR ( 'NONE', #18544, 1000.000000000000000 ) ;
#37357 = LINE ( 'NONE', #40186, #30239 ) ;
#37358 = AXIS2_PLACEMENT_3D ( 'NONE', #35871, #41996, #6002 ) ;
#37359 = ORIENTED_EDGE ( 'NONE', *, *, #20978, .T. ) ;
#37360 = AXIS2_PLACEMENT_3D ( 'NONE', #4663, #16223, #19943 ) ;
#37362 = ORIENTED_EDGE ( 'NONE', *, *, #33197, .T. ) ;
#37361 = DIRECTION ( 'NONE',  ( 0.000000000000000000, 0.000000000000000000, -1.000000000000000000 ) ) ;
#37363 = CARTESIAN_POINT ( 'NONE',  ( 76.30724621508588257, 31.00000000000000000, -9.942258256679791018 ) ) ;
#37364 = AXIS2_PLACEMENT_3D ( 'NONE', #38875, #42565, #22767 ) ;
#37365 = VERTEX_POINT ( 'NONE', #1994 ) ;
#37366 = CARTESIAN_POINT ( 'NONE',  ( -4.204114297095464359, 1.660363174096617156, -3.602136431857887011 ) ) ;
#37367 = COLOUR_RGB ( '', 0.40784314, 0.44705882, 0.49803922) ;
#37368 = EDGE_CURVE ( 'NONE', #13787, #26181, #15376, .T. ) ;
#37369 = ORIENTED_EDGE ( 'NONE', *, *, #10110, .T. ) ;
#37370 = ADVANCED_FACE ( 'NONE', ( #23826 ), #13353, .T. ) ;
#37371 = DIRECTION ( 'NONE',  ( 1.000000000000000000, 0.000000000000000000, -0.000000000000000000 ) ) ;
#37372 = AXIS2_PLACEMENT_3D ( 'NONE', #31579, #1890, #11961 ) ;
#37373 = VERTEX_POINT ( 'NONE', #3480 ) ;
#37374 = CARTESIAN_POINT ( 'NONE',  ( -79.17211738000736432, 40.00000000000000711, 45.58486055166100215 ) ) ;
#37376 = DIRECTION ( 'NONE',  ( -1.000000000000000000, 0.000000000000000000, -0.000000000000000000 ) ) ;
#37375 = DIRECTION ( 'NONE',  ( 1.000000000000000000, 0.000000000000000000, 0.000000000000000000 ) ) ;
#37377 = AXIS2_PLACEMENT_3D ( 'NONE', #58, #40635, #23899 ) ;
#37378 = CYLINDRICAL_SURFACE ( 'NONE', #394, 116.0000000000000000 ) ;
#37379 = DIRECTION ( 'NONE',  ( 0.000000000000000000, 0.000000000000000000, 1.000000000000000000 ) ) ;
#37380 = VERTEX_POINT ( 'NONE', #3909 ) ;
#37381 = PRESENTATION_STYLE_ASSIGNMENT (( #10560 ) ) ;
#37382 = CARTESIAN_POINT ( 'NONE',  ( 0.000000000000000000, 110.1579703617969130, -21.29539948940136540 ) ) ;
#37383 = CARTESIAN_POINT ( 'NONE',  ( 28.03234818517180216, 31.00000000000000355, 82.53419278363811884 ) ) ;
#37384 = DIRECTION ( 'NONE',  ( -3.009274222672345096E-17, -1.000000000000000000, 2.455023325076454960E-18 ) ) ;
#37385 = VECTOR ( 'NONE', #22425, 1000.000000000000000 ) ;
#37386 = ORIENTED_EDGE ( 'NONE', *, *, #28317, .T. ) ;
#37387 = FACE_OUTER_BOUND ( 'NONE', #32631, .T. ) ;
#37388 = ADVANCED_FACE ( 'NONE', ( #20137 ), #13565, .T. ) ;
#37389 = AXIS2_PLACEMENT_3D ( 'NONE', #29470, #12889, #19037 ) ;
#37390 = VERTEX_POINT ( 'NONE', #3034 ) ;
#37391 = ORIENTED_EDGE ( 'NONE', *, *, #19844, .F. ) ;
#37392 = DIRECTION ( 'NONE',  ( 1.000000000000000000, 0.000000000000000000, 0.000000000000000000 ) ) ;
#37393 = DIRECTION ( 'NONE',  ( -1.000000000000000000, -0.000000000000000000, 0.000000000000000000 ) ) ;
#37394 = AXIS2_PLACEMENT_3D ( 'NONE', #18303, #5152, #14794 ) ;
#37395 = DIRECTION ( 'NONE',  ( 1.000000000000000000, 0.000000000000000000, 0.000000000000000000 ) ) ;
#37396 = EDGE_LOOP ( 'NONE', ( #27023, #144, #34290, #5058 ) ) ;
#37397 = LINE ( 'NONE', #21309, #11742 ) ;
#37398 = ORIENTED_EDGE ( 'NONE', *, *, #16627, .T. ) ;
#37399 = DIRECTION ( 'NONE',  ( -1.000000000000000000, 0.000000000000000000, 0.000000000000000000 ) ) ;
#37400 = AXIS2_PLACEMENT_3D ( 'NONE', #8201, #11712, #31332 ) ;
#37401 = DIRECTION ( 'NONE',  ( 0.000000000000000000, -0.6783118362696075598, -0.7347741508630750706 ) ) ;
#37402 = CARTESIAN_POINT ( 'NONE',  ( 17.99999999999999645, 111.2721026680460596, 44.61974821237341615 ) ) ;
#37403 = ORIENTED_EDGE ( 'NONE', *, *, #31759, .F. ) ;
#37404 = EDGE_LOOP ( 'NONE', ( #36172, #41957, #30568, #8061 ) ) ;
#37405 = DIRECTION ( 'NONE',  ( 0.000000000000000000, 0.000000000000000000, 1.000000000000000000 ) ) ;
#37406 = CYLINDRICAL_SURFACE ( 'NONE', #8878, 13.40000000000000213 ) ;
#37407 = CARTESIAN_POINT ( 'NONE',  ( 4.000000000000000000, -0.8732470631449981147, -3.223155494240760088 ) ) ;
#37408 = ORIENTED_EDGE ( 'NONE', *, *, #38823, .T. ) ;
#37410 = ORIENTED_EDGE ( 'NONE', *, *, #33010, .T. ) ;
#37409 = DIRECTION ( 'NONE',  ( 0.000000000000000000, 0.000000000000000000, 1.000000000000000000 ) ) ;
#37411 = CARTESIAN_POINT ( 'NONE',  ( -42.09738266246711191, 31.00000000000000355, -2.828681863544771691 ) ) ;
#37412 = LINE ( 'NONE', #24148, #20991 ) ;
#37413 = CIRCLE ( 'NONE', #29095, 116.0000000000000000 ) ;
#37414 = CIRCLE ( 'NONE', #11699, 52.00000000000000000 ) ;
#37415 = EDGE_CURVE ( 'NONE', #32115, #11322, #33603, .T. ) ;
#37416 = AXIS2_PLACEMENT_3D ( 'NONE', #20386, #14254, #23872 ) ;
#37418 = ORIENTED_EDGE ( 'NONE', *, *, #38772, .T. ) ;
#37417 = CARTESIAN_POINT ( 'NONE',  ( 0.000000000000000000, 75.72520367775085504, 82.78868281116005789 ) ) ;
#37419 = ORIENTED_EDGE ( 'NONE', *, *, #16007, .T. ) ;
#37420 = CYLINDRICAL_SURFACE ( 'NONE', #30790, 116.0000000000000000 ) ;
#37421 = CARTESIAN_POINT ( 'NONE',  ( -37.00582609754565766, 40.00000000000000000, 48.07482304778140758 ) ) ;
#37422 = AXIS2_PLACEMENT_3D ( 'NONE', #41140, #3832, #24621 ) ;
#37423 = AXIS2_PLACEMENT_3D ( 'NONE', #23279, #13451, #36116 ) ;
#37424 = AXIS2_PLACEMENT_3D ( 'NONE', #7079, #33694, #948 ) ;
#37425 = CYLINDRICAL_SURFACE ( 'NONE', #6819, 120.5010000000000190 ) ;
#37426 = CIRCLE ( 'NONE', #14483, 20.00000000000000711 ) ;
#37427 = DIRECTION ( 'NONE',  ( -1.000000000000000000, -0.000000000000000000, -0.000000000000000000 ) ) ;
#37428 = VERTEX_POINT ( 'NONE', #26645 ) ;
#37429 = CARTESIAN_POINT ( 'NONE',  ( 18.00000000000000355, 0.000000000000000000, 0.000000000000000000 ) ) ;
#37430 = ORIENTED_EDGE ( 'NONE', *, *, #26348, .T. ) ;
#37431 = CARTESIAN_POINT ( 'NONE',  ( 12.49999999999995204, -1.368091241319530598E-13, -45.00000000000000000 ) ) ;
#37432 = DIRECTION ( 'NONE',  ( -3.996523416598930318E-16, 2.658563593772947863E-15, 1.000000000000000000 ) ) ;
#37433 = VECTOR ( 'NONE', #27152, 1000.000000000000000 ) ;
#37434 = CARTESIAN_POINT ( 'NONE',  ( 48.45771864870608425, 31.00000000000000355, 27.97524394371832202 ) ) ;
#37435 = DIRECTION ( 'NONE',  ( 0.000000000000000000, -0.1590634960190596137, -0.9872683547213465527 ) ) ;
#37436 = VERTEX_POINT ( 'NONE', #3263 ) ;
#37437 = SHAPE_REPRESENTATION ( 'hex flange nut gradea_iso_ISO - 4161 - M5 - N', ( #13552 ), #41354 ) ;
#37438 = CARTESIAN_POINT ( 'NONE',  ( 17.99999999999999645, 119.8996782608629985, 12.02323392193397211 ) ) ;
#37439 = ORIENTED_EDGE ( 'NONE', *, *, #41368, .F. ) ;
#37440 = CARTESIAN_POINT ( 'NONE',  ( -7.088330391075835735, 40.00000000000000000, -20.85399598300688595 ) ) ;
#37441 = EDGE_CURVE ( 'NONE', #13305, #15791, #32041, .T. ) ;
#37442 = VERTEX_POINT ( 'NONE', #10270 ) ;
#37443 = DIRECTION ( 'NONE',  ( -1.000000000000000000, -0.000000000000000000, -0.000000000000000000 ) ) ;
#37444 = EDGE_CURVE ( 'NONE', #10305, #41147, #32954, .T. ) ;
#37445 = CARTESIAN_POINT ( 'NONE',  ( 0.000000000000000000, -114.1157422997284669, 20.82300072952894610 ) ) ;
#37446 = AXIS2_PLACEMENT_3D ( 'NONE', #27132, #26689, #23228 ) ;
#37447 = CARTESIAN_POINT ( 'NONE',  ( 60.45897909542819804, 31.00000000000000000, -46.24578392211154210 ) ) ;
#37448 = CARTESIAN_POINT ( 'NONE',  ( 46.16409756962309530, 40.00000000000000000, -59.99419878592187416 ) ) ;
#37449 = DIRECTION ( 'NONE',  ( 0.000000000000000000, -0.9574220383620022368, -0.2886919473396314384 ) ) ;
#37450 = CIRCLE ( 'NONE', #18022, 51.99999999999999289 ) ;
#37451 = CIRCLE ( 'NONE', #24998, 13.59999999999999787 ) ;
#37452 = ORIENTED_EDGE ( 'NONE', *, *, #24164, .F. ) ;
#37453 = CARTESIAN_POINT ( 'NONE',  ( 0.000000000000000000, 97.19627249181095863, 71.22763238166520239 ) ) ;
#37454 = AXIS2_PLACEMENT_3D ( 'NONE', #16000, #22345, #19072 ) ;
#37455 = ORIENTED_EDGE ( 'NONE', *, *, #15965, .T. ) ;
#37456 = AXIS2_PLACEMENT_3D ( 'NONE', #25019, #2035, #5324 ) ;
#37457 = SURFACE_SIDE_STYLE ('',( #24189 ) ) ;
#37458 = DIRECTION ( 'NONE',  ( 0.000000000000000000, 0.9996456111234526265, -0.02662052143777148688 ) ) ;
#37459 = VECTOR ( 'NONE', #33866, 1000.000000000000000 ) ;
#37461 = VERTEX_POINT ( 'NONE', #10044 ) ;
#37460 = CARTESIAN_POINT ( 'NONE',  ( 17.99999999999999645, 71.21168426767221149, -86.70160608319253015 ) ) ;
#37462 = LINE ( 'NONE', #14798, #19845 ) ;
#37463 = ORIENTED_EDGE ( 'NONE', *, *, #28948, .F. ) ;
#37464 = DIRECTION ( 'NONE',  ( -1.000000000000000000, -0.000000000000000000, 0.000000000000000000 ) ) ;
#37465 = EDGE_CURVE ( 'NONE', #19047, #27109, #30576, .T. ) ;
#37466 = CARTESIAN_POINT ( 'NONE',  ( 73.03870520561201829, 39.99999999999999289, -42.18585045165268355 ) ) ;
#37467 = CARTESIAN_POINT ( 'NONE',  ( 17.99999999999999645, 0.000000000000000000, 0.000000000000000000 ) ) ;
#37468 = CIRCLE ( 'NONE', #20079, 142.4999999999992610 ) ;
#37469 = VERTEX_POINT ( 'NONE', #26859 ) ;
#37470 = DIRECTION ( 'NONE',  ( 0.000000000000000000, -0.6783118362696074488, -0.7347741508630751817 ) ) ;
#37471 = CARTESIAN_POINT ( 'NONE',  ( 0.000000000000000000, 0.000000000000000000, 0.000000000000000000 ) ) ;
#37472 = ORIENTED_EDGE ( 'NONE', *, *, #40367, .T. ) ;
#37473 = EDGE_CURVE ( 'NONE', #41239, #24752, #23387, .T. ) ;
#37474 = SURFACE_STYLE_USAGE ( .BOTH. , #27035 ) ;
#37475 = VERTEX_POINT ( 'NONE', #9831 ) ;
#37476 = CARTESIAN_POINT ( 'NONE',  ( 18.00000000000000355, 34.03046037009255542, 33.13733193845817482 ) ) ;
#37477 = ORIENTED_EDGE ( 'NONE', *, *, #29006, .F. ) ;
#37478 = CARTESIAN_POINT ( 'NONE',  ( 28.62564328229377608, 40.00000000000000000, -21.88780996305825965 ) ) ;
#37479 = DIRECTION ( 'NONE',  ( 1.058513553088275437E-16, 1.000000000000000000, -8.813324511995299047E-17 ) ) ;
#37480 = EDGE_CURVE ( 'NONE', #19076, #37542, #23038, .T. ) ;
#37481 = CIRCLE ( 'NONE', #19429, 20.00000000000000711 ) ;
#37482 = CARTESIAN_POINT ( 'NONE',  ( 18.00000000000000355, 45.78515115856060191, -12.64416602183617577 ) ) ;
#37483 = DIRECTION ( 'NONE',  ( -3.996523416598930318E-16, 2.658563593772947863E-15, 1.000000000000000000 ) ) ;
#37484 = EDGE_LOOP ( 'NONE', ( #31013, #30284, #41452, #6236 ) ) ;
#37485 = VECTOR ( 'NONE', #28262, 1000.000000000000000 ) ;
#37487 = DIRECTION ( 'NONE',  ( -1.000000000000000000, -0.000000000000000000, -0.000000000000000000 ) ) ;
#37486 = DIRECTION ( 'NONE',  ( 0.000000000000000000, 0.000000000000000000, 1.000000000000000000 ) ) ;
#37488 = AXIS2_PLACEMENT_3D ( 'NONE', #1870, #15232, #35033 ) ;
#37489 = ORIENTED_EDGE ( 'NONE', *, *, #34780, .T. ) ;
#37490 = AXIS2_PLACEMENT_3D ( 'NONE', #31498, #1583, #7707 ) ;
#37491 = AXIS2_PLACEMENT_3D ( 'NONE', #10323, #10090, #23231 ) ;
#37492 = CYLINDRICAL_SURFACE ( 'NONE', #39166, 51.99999999999999289 ) ;
#37493 = CARTESIAN_POINT ( 'NONE',  ( 17.42035916340572399, 31.00000000000000355, 19.85006075799527991 ) ) ;
#37494 = EDGE_LOOP ( 'NONE', ( #20043, #2244, #26114, #334 ) ) ;
#37495 = DIRECTION ( 'NONE',  ( 0.000000000000000000, 0.000000000000000000, 1.000000000000000000 ) ) ;
#37496 = CIRCLE ( 'NONE', #27056, 59.00000000000000000 ) ;
#37497 = FACE_OUTER_BOUND ( 'NONE', #3662, .T. ) ;
#37498 = DIRECTION ( 'NONE',  ( 0.000000000000000000, 0.000000000000000000, 1.000000000000000000 ) ) ;
#37499 = CARTESIAN_POINT ( 'NONE',  ( -21.91107887650263564, 31.00000000000000355, 64.54935342160338507 ) ) ;
#37500 = ADVANCED_FACE ( 'NONE', ( #641 ), #27295, .T. ) ;
#37501 = EDGE_CURVE ( 'NONE', #12205, #33352, #9756, .T. ) ;
#37502 = EDGE_LOOP ( 'NONE', ( #5090, #370, #16989, #32445 ) ) ;
#37503 = CARTESIAN_POINT ( 'NONE',  ( -34.17541447290002310, 31.00000000000000355, -26.31327426976606176 ) ) ;
#37504 = EDGE_CURVE ( 'NONE', #20054, #5213, #2084, .T. ) ;
#37505 = EDGE_CURVE ( 'NONE', #13412, #37603, #17296, .T. ) ;
#37506 = CARTESIAN_POINT ( 'NONE',  ( 80.16187752211510542, 39.99999999999999289, -27.22680903928618434 ) ) ;
#37507 = CARTESIAN_POINT ( 'NONE',  ( -23.34979319748359927, 5.944745455504278020, 2.972870684497277427 ) ) ;
#37508 = CARTESIAN_POINT ( 'NONE',  ( 0.000000000000000000, 0.000000000000000000, 0.000000000000000000 ) ) ;
#37509 = DIRECTION ( 'NONE',  ( 1.058513553088275437E-16, 1.000000000000000000, -8.813324511995299047E-17 ) ) ;
#37510 = AXIS2_PLACEMENT_3D ( 'NONE', #16292, #26113, #42650 ) ;
#37511 = AXIS2_PLACEMENT_3D ( 'NONE', #6926, #26159, #19426 ) ;
#37513 = EDGE_LOOP ( 'NONE', ( #37078, #24640, #33202, #21177 ) ) ;
#37512 = CARTESIAN_POINT ( 'NONE',  ( 17.99999999999999645, -29.68570942776464960, -10.53307442156965656 ) ) ;
#37514 = DIRECTION ( 'NONE',  ( 0.000000000000000000, 0.9911528310040066403, 0.1327255272837255529 ) ) ;
#37515 = DIRECTION ( 'NONE',  ( 1.000000000000000000, 0.000000000000000000, 0.000000000000000000 ) ) ;
#37516 = CIRCLE ( 'NONE', #15299, 59.00000000000000000 ) ;
#37517 = VERTEX_POINT ( 'NONE', #30349 ) ;
#37518 = CARTESIAN_POINT ( 'NONE',  ( 37.24516168167158270, 40.00000000000000000, 42.45166511289891531 ) ) ;
#37519 = DIRECTION ( 'NONE',  ( 1.000000000000000000, 0.000000000000000000, 0.000000000000000000 ) ) ;
#37520 = DIRECTION ( 'NONE',  ( -1.000000000000000000, 0.000000000000000000, -0.000000000000000000 ) ) ;
#37521 = CIRCLE ( 'NONE', #16634, 47.49900000000000233 ) ;
#37522 = ORIENTED_EDGE ( 'NONE', *, *, #4961, .T. ) ;
#37523 = DIRECTION ( 'NONE',  ( 0.000000000000000000, 0.000000000000000000, 1.000000000000000000 ) ) ;
#37524 = DIRECTION ( 'NONE',  ( -1.000000000000000000, 0.000000000000000000, 0.000000000000000000 ) ) ;
#37525 = VERTEX_POINT ( 'NONE', #27087 ) ;
#37526 = CARTESIAN_POINT ( 'NONE',  ( 0.000000000000000000, -69.90696807222415998, -98.15042952503588936 ) ) ;
#37527 = ORIENTED_EDGE ( 'NONE', *, *, #41312, .F. ) ;
#37528 = ADVANCED_FACE ( 'NONE', ( #7195 ), #6776, .F. ) ;
#37529 = DIRECTION ( 'NONE',  ( 3.009274222672345096E-17, 1.000000000000000000, -2.455023325076455345E-18 ) ) ;
#37530 = ORIENTED_EDGE ( 'NONE', *, *, #9749, .F. ) ;
#37531 = CARTESIAN_POINT ( 'NONE',  ( 17.99999999999999645, -25.52601536738579213, -19.21447964122724272 ) ) ;
#37532 = CARTESIAN_POINT ( 'NONE',  ( -101.9001375416480499, 31.00000000000000711, 6.549163350515033954 ) ) ;
#37533 = ORIENTED_EDGE ( 'NONE', *, *, #129, .F. ) ;
#37534 = DIRECTION ( 'NONE',  ( 1.000000000000000000, 0.000000000000000000, 0.000000000000000000 ) ) ;
#37535 = CARTESIAN_POINT ( 'NONE',  ( 0.000000000000000000, 25.52601536738619714, -19.21447964122670626 ) ) ;
#37536 = ORIENTED_EDGE ( 'NONE', *, *, #24790, .F. ) ;
#37537 = CARTESIAN_POINT ( 'NONE',  ( 18.00000000000000355, -44.75336757549769118, -14.30704879393654316 ) ) ;
#37538 = CARTESIAN_POINT ( 'NONE',  ( 0.000000000000000000, 62.45178862086215332, 93.20969140437529177 ) ) ;
#37539 = AXIS2_PLACEMENT_3D ( 'NONE', #37833, #35215, #31320 ) ;
#37540 = CARTESIAN_POINT ( 'NONE',  ( 0.000000000000000000, 119.7318547011701497, 13.59315897125768124 ) ) ;
#37541 = CARTESIAN_POINT ( 'NONE',  ( -15.99999999999997691, 17.11489954122026447, 2.500000000000006217 ) ) ;
#37542 = VERTEX_POINT ( 'NONE', #29931 ) ;
#37543 = DIRECTION ( 'NONE',  ( 0.000000000000000000, 1.000000000000000000, 0.000000000000000000 ) ) ;
#37544 = CARTESIAN_POINT ( 'NONE',  ( 0.000000000000000000, 0.000000000000000000, 0.000000000000000000 ) ) ;
#37545 = CARTESIAN_POINT ( 'NONE',  ( -29.26739590608564967, 31.00000000000000355, 25.68069354617348665 ) ) ;
#37546 = ORIENTED_EDGE ( 'NONE', *, *, #4433, .T. ) ;
#37548 = DIRECTION ( 'NONE',  ( 0.000000000000000000, 0.000000000000000000, 1.000000000000000000 ) ) ;
#37547 = DIRECTION ( 'NONE',  ( -1.000000000000000000, -0.000000000000000000, -0.000000000000000000 ) ) ;
#37549 = DIRECTION ( 'NONE',  ( 0.000000000000000000, 0.9822872507286892763, -0.1873813145857214368 ) ) ;
#37550 = EDGE_CURVE ( 'NONE', #42747, #11747, #22977, .T. ) ;
#37551 = ORIENTED_EDGE ( 'NONE', *, *, #26933, .F. ) ;
#37552 = ADVANCED_FACE ( 'NONE', ( #17947 ), #37951, .F. ) ;
#37553 = EDGE_CURVE ( 'NONE', #9021, #10641, #4878, .T. ) ;
#37554 = DIRECTION ( 'NONE',  ( 0.000000000000000000, 0.000000000000000000, 1.000000000000000000 ) ) ;
#37555 = CARTESIAN_POINT ( 'NONE',  ( -25.89845354150052259, 40.00000000000000000, -44.83417823681238445 ) ) ;
#37556 = CARTESIAN_POINT ( 'NONE',  ( -26.77709713318651552, 40.00000000000000000, 54.08981485145582724 ) ) ;
#37557 = ADVANCED_FACE ( 'NONE', ( #14429 ), #4805, .F. ) ;
#37558 = DIRECTION ( 'NONE',  ( -1.000000000000000000, 0.000000000000000000, 0.000000000000000000 ) ) ;
#37559 = CYLINDRICAL_SURFACE ( 'NONE', #9588, 58.99999999999999289 ) ;
#37560 = EDGE_CURVE ( 'NONE', #16913, #1690, #29993, .T. ) ;
#37561 = DIRECTION ( 'NONE',  ( -1.000000000000000000, -0.000000000000000000, -0.000000000000000000 ) ) ;
#37562 = LINE ( 'NONE', #7019, #1525 ) ;
#37563 = ORIENTED_EDGE ( 'NONE', *, *, #25485, .T. ) ;
#37564 = CARTESIAN_POINT ( 'NONE',  ( -10.86393331615775892, 40.00000000000000000, -18.79923026442779843 ) ) ;
#37565 = ORIENTED_EDGE ( 'NONE', *, *, #14997, .T. ) ;
#37566 = CARTESIAN_POINT ( 'NONE',  ( 17.99999999999999645, 0.000000000000000000, 0.000000000000000000 ) ) ;
#37567 = CARTESIAN_POINT ( 'NONE',  ( 0.000000000000000000, 0.000000000000000000, 0.000000000000000000 ) ) ;
#37568 = EDGE_CURVE ( 'NONE', #35149, #1962, #42507, .T. ) ;
#37569 = ORIENTED_EDGE ( 'NONE', *, *, #14686, .T. ) ;
#37570 = VECTOR ( 'NONE', #5752, 1000.000000000000000 ) ;
#37571 = AXIS2_PLACEMENT_3D ( 'NONE', #16432, #33419, #3288 ) ;
#37572 = DIRECTION ( 'NONE',  ( 0.000000000000000000, 0.000000000000000000, 1.000000000000000000 ) ) ;
#37573 = DIRECTION ( 'NONE',  ( 1.000000000000000000, -1.373900992973642263E-15, -4.095874873834148624E-16 ) ) ;
#37574 = ORIENTED_EDGE ( 'NONE', *, *, #29147, .F. ) ;
#37575 = DIRECTION ( 'NONE',  ( 0.000000000000000000, 0.000000000000000000, 1.000000000000000000 ) ) ;
#37576 = EDGE_LOOP ( 'NONE', ( #29832, #15854, #30934, #29048 ) ) ;
#37577 = ORIENTED_EDGE ( 'NONE', *, *, #36621, .F. ) ;
#37579 = VERTEX_POINT ( 'NONE', #11583 ) ;
#37578 = DIRECTION ( 'NONE',  ( -1.000000000000000000, -0.000000000000000000, -0.000000000000000000 ) ) ;
#37580 = CARTESIAN_POINT ( 'NONE',  ( -64.10496366466531981, 31.00000000000000711, 31.48763712508877077 ) ) ;
#37581 = ORIENTED_EDGE ( 'NONE', *, *, #4411, .F. ) ;
#37582 = CARTESIAN_POINT ( 'NONE',  ( 18.00000000000000355, 19.74581912682842244, 48.10512059033398913 ) ) ;
#37583 = EDGE_CURVE ( 'NONE', #3236, #27591, #34046, .T. ) ;
#37584 = EDGE_LOOP ( 'NONE', ( #2468, #24137, #19217, #5121, #41855, #42471, #42257, #28275, #42466, #23710, #40876, #7083, #7744, #17279, #17709, #5552, #28036, #10657, #27762, #12701, #3121, #6722, #32475, #4783, #33090, #41601, #30547, #6300, #39835, #3587, #23996, #42786, #42661, #8073, #3843, #2330, #41005, #14919, #1014, #10789, #32161, #34885, #36358, #23949, #42916, #14565, #525, #42668, #21972, #16970, #14697, #35809, #34739, #11643, #1560, #17188, #28699, #17410, #1882, #35157, #37669, #17454, #818, #33648, #39781, #33101, #12362, #33721, #12738, #18463, #33276, #42215, #24408, #701, #9239, #30524, #36873, #13388, #24372, #31943, #24163, #4196, #4212, #8662, #33971, #25236, #15519, #8643, #900, #10467, #42191, #26703, #24188, #28705, #34043, #2220, #6096, #29486, #4276, #37777, #35880, #22357, #3952, #36082, #14093, #23598, #8077, #16908, #34081, #5759, #39807, #15731, #12047, #18024, #34097, #4405, #27465, #19534, #42744, #41395, #13895, #16906, #17347, #10724, #41722, #4873, #21592, #12035, #34041, #32151, #31854, #39726, #6361, #33674, #10426, #20410, #9798, #4838, #38838, #22993, #15868, #32403, #3680, #15715, #30090, #38108, #41906, #3899, #41220, #25836, #12296, #31972, #29701, #18593, #23624, #6933, #34079, #41445, #33652, #17588, #14643, #28758, #16498, #43147, #11636, #20628, #6377, #40103, #6350, #11404, #29658, #36000, #11028, #9524, #2069, #5957, #31345, #4550, #15481, #30453, #41370, #11280, #5528, #3706, #20329, #11376, #12113, #18143, #24945, #28350, #21755, #18798, #16513, #25858, #28710, #8684, #9762, #40356, #7251, #2611, #30768, #27722, #26814 ) ) ;
#37585 = CARTESIAN_POINT ( 'NONE',  ( -10.00000000000000000, 0.000000000000000000, 0.000000000000000000 ) ) ;
#37586 = EDGE_LOOP ( 'NONE', ( #30202, #41758, #28687, #8123 ) ) ;
#37587 = CARTESIAN_POINT ( 'NONE',  ( 47.87658044100083288, 39.99999999999999289, -82.67148682534872250 ) ) ;
#37589 = CYLINDRICAL_SURFACE ( 'NONE', #33954, 59.00000000000000000 ) ;
#37588 = DIRECTION ( 'NONE',  ( -1.000000000000000000, -0.000000000000000000, 0.000000000000000000 ) ) ;
#37590 = DIRECTION ( 'NONE',  ( -1.000000000000000000, -0.000000000000000000, 0.000000000000000000 ) ) ;
#37591 = CARTESIAN_POINT ( 'NONE',  ( 18.00000000000000355, 44.47301969247467923, -16.68249143361863318 ) ) ;
#37592 = EDGE_LOOP ( 'NONE', ( #8787, #30729, #38034, #24077 ) ) ;
#37593 = SURFACE_STYLE_FILL_AREA ( #17575 ) ;
#37594 = AXIS2_PLACEMENT_3D ( 'NONE', #38465, #31725, #22796 ) ;
#37595 = CARTESIAN_POINT ( 'NONE',  ( 8.999999999999998224, 115.5737863835462349, 9.934782381634081005 ) ) ;
#37596 = CARTESIAN_POINT ( 'NONE',  ( -89.62817255407412631, 31.00000000000000711, -11.80141054548196422 ) ) ;
#37597 = AXIS2_PLACEMENT_3D ( 'NONE', #1135, #18212, #1354 ) ;
#37598 = CARTESIAN_POINT ( 'NONE',  ( 0.000000000000000000, -21.48775762007876367, 23.64423737150130478 ) ) ;
#37599 = VERTEX_POINT ( 'NONE', #27960 ) ;
#37600 = EDGE_CURVE ( 'NONE', #8918, #33767, #24694, .T. ) ;
#37601 = CARTESIAN_POINT ( 'NONE',  ( -14.30682334061562422, 40.00000000000000000, -18.65445469299709202 ) ) ;
#37602 = ORIENTED_EDGE ( 'NONE', *, *, #38261, .F. ) ;
#37603 = VERTEX_POINT ( 'NONE', #40783 ) ;
#37604 = CARTESIAN_POINT ( 'NONE',  ( -105.9879088449591933, 17.11489954122026447, -0.3807199291576673361 ) ) ;
#37605 = CARTESIAN_POINT ( 'NONE',  ( -139.5000000000000000, 0.000000000000000000, 9.999999999999998224 ) ) ;
#37606 = DIRECTION ( 'NONE',  ( -0.000000000000000000, -0.000000000000000000, 1.000000000000000000 ) ) ;
#37607 = CARTESIAN_POINT ( 'NONE',  ( 0.000000000000000000, -112.1702510623870666, 2.471285140322257323 ) ) ;
#37608 = ADVANCED_FACE ( 'NONE', ( #41214 ), #24925, .T. ) ;
#37609 = EDGE_LOOP ( 'NONE', ( #29079, #34862, #19011, #3379 ) ) ;
#37610 = DIRECTION ( 'NONE',  ( 1.000000000000000000, -1.373900992973642460E-15, -3.469446951953632924E-16 ) ) ;
#37611 = VERTEX_POINT ( 'NONE', #24041 ) ;
#37612 = DIRECTION ( 'NONE',  ( -1.000000000000000000, 0.000000000000000000, 0.000000000000000000 ) ) ;
#37613 = LINE ( 'NONE', #20651, #6067 ) ;
#37614 = DIRECTION ( 'NONE',  ( 0.000000000000000000, 0.8993121301712202476, -0.4373073204588531770 ) ) ;
#37615 = DIRECTION ( 'NONE',  ( 0.000000000000000000, 0.000000000000000000, 1.000000000000000000 ) ) ;
#37616 = ORIENTED_EDGE ( 'NONE', *, *, #26997, .T. ) ;
#37617 = EDGE_LOOP ( 'NONE', ( #20893, #18875, #25405, #41205 ) ) ;
#37618 = DIRECTION ( 'NONE',  ( -1.000000000000000000, -0.000000000000000000, -0.000000000000000000 ) ) ;
#37619 = CARTESIAN_POINT ( 'NONE',  ( -31.74999999999999289, -19.19999999999999574, 2.351321854362917684E-15 ) ) ;
#37620 = DIRECTION ( 'NONE',  ( 1.000000000000000000, 1.836909530733573776E-16, 0.000000000000000000 ) ) ;
#37621 = AXIS2_PLACEMENT_3D ( 'NONE', #6376, #1058, #9665 ) ;
#37622 = EDGE_LOOP ( 'NONE', ( #24130, #37452, #2682, #17400 ) ) ;
#37624 = ORIENTED_EDGE ( 'NONE', *, *, #42325, .T. ) ;
#37623 = LINE ( 'NONE', #21104, #22271 ) ;
#37625 = AXIS2_PLACEMENT_3D ( 'NONE', #11285, #37660, #35038 ) ;
#37626 = CARTESIAN_POINT ( 'NONE',  ( 29.49207856985708176, 31.00000000000000355, 38.57905506995707867 ) ) ;
#37627 = AXIS2_PLACEMENT_3D ( 'NONE', #33354, #19859, #33559 ) ;
#37628 = DIRECTION ( 'NONE',  ( 1.000000000000000000, 0.000000000000000000, 0.000000000000000000 ) ) ;
#37629 = CIRCLE ( 'NONE', #4203, 20.00000000000000711 ) ;
#37631 = DIRECTION ( 'NONE',  ( 0.000000000000000000, 0.000000000000000000, 1.000000000000000000 ) ) ;
#37630 = DIRECTION ( 'NONE',  ( 1.000000000000000000, 0.000000000000000000, 0.000000000000000000 ) ) ;
#37632 = EDGE_LOOP ( 'NONE', ( #8985, #36314, #18978, #11030 ) ) ;
#37633 = CARTESIAN_POINT ( 'NONE',  ( -3.998040010416403334, 40.00000000000000000, 59.59469406578620720 ) ) ;
#37634 = DIRECTION ( 'NONE',  ( 1.000000000000000000, -0.000000000000000000, 0.000000000000000000 ) ) ;
#37635 = DIRECTION ( 'NONE',  ( -1.000000000000000000, 0.000000000000000000, 0.000000000000000000 ) ) ;
#37636 = ORIENTED_EDGE ( 'NONE', *, *, #38408, .T. ) ;
#37637 = DIRECTION ( 'NONE',  ( -1.000000000000000000, -0.000000000000000000, -0.000000000000000000 ) ) ;
#37638 = ORIENTED_EDGE ( 'NONE', *, *, #22114, .T. ) ;
#37639 =( NAMED_UNIT ( * ) PLANE_ANGLE_UNIT ( ) SI_UNIT ( $, .RADIAN. ) );
#37640 = CYLINDRICAL_SURFACE ( 'NONE', #19750, 20.00000000000000355 ) ;
#37641 = LINE ( 'NONE', #324, #24837 ) ;
#37642 = AXIS2_PLACEMENT_3D ( 'NONE', #5031, #39032, #21875 ) ;
#37643 = CARTESIAN_POINT ( 'NONE',  ( -37.49462465745612860, 31.00000000000000355, -48.86220178749748300 ) ) ;
#37644 = DIRECTION ( 'NONE',  ( -1.000000000000000000, 0.000000000000000000, 0.000000000000000000 ) ) ;
#37645 = ORIENTED_EDGE ( 'NONE', *, *, #32402, .F. ) ;
#37646 = EDGE_CURVE ( 'NONE', #6459, #33918, #27217, .T. ) ;
#37647 = AXIS2_PLACEMENT_3D ( 'NONE', #36551, #6676, #33306 ) ;
#37648 = EDGE_CURVE ( 'NONE', #2879, #9347, #14865, .T. ) ;
#37649 =( NAMED_UNIT ( * ) PLANE_ANGLE_UNIT ( ) SI_UNIT ( $, .RADIAN. ) );
#37650 = ORIENTED_EDGE ( 'NONE', *, *, #33189, .F. ) ;
#37651 = CARTESIAN_POINT ( 'NONE',  ( -24.68525358734468611, 40.00000000000000000, -18.92943107747915832 ) ) ;
#37652 = AXIS2_PLACEMENT_3D ( 'NONE', #6663, #33065, #32855 ) ;
#37653 = ORIENTED_EDGE ( 'NONE', *, *, #17864, .T. ) ;
#37654 = CARTESIAN_POINT ( 'NONE',  ( -17.77999999999999758, 0.000000000000000000, 0.000000000000000000 ) ) ;
#37655 = AXIS2_PLACEMENT_3D ( 'NONE', #22709, #35957, #25555 ) ;
#37656 = CARTESIAN_POINT ( 'NONE',  ( 0.000000000000000000, 40.47821179127761582, -32.64221760512715775 ) ) ;
#37657 = CARTESIAN_POINT ( 'NONE',  ( 76.90008882636698218, 31.00000000000000000, -4.923574515426284215 ) ) ;
#37658 = CARTESIAN_POINT ( 'NONE',  ( 34.80713033128647993, 40.00000000000000000, 70.84796410819511436 ) ) ;
#37659 = VECTOR ( 'NONE', #34189, 1000.000000000000000 ) ;
#37660 = DIRECTION ( 'NONE',  ( -1.000000000000000000, -0.000000000000000000, 0.000000000000000000 ) ) ;
#37661 = ADVANCED_FACE ( 'NONE', ( #31636 ), #27512, .F. ) ;
#37662 = ORIENTED_EDGE ( 'NONE', *, *, #40195, .F. ) ;
#37663 = DIRECTION ( 'NONE',  ( -1.000000000000000000, 0.000000000000000000, 0.000000000000000000 ) ) ;
#37664 = ORIENTED_EDGE ( 'NONE', *, *, #6196, .T. ) ;
#37665 = CARTESIAN_POINT ( 'NONE',  ( 0.000000000000000000, -17.50309955389580452, -43.60271849949383949 ) ) ;
#37666 = EDGE_CURVE ( 'NONE', #19378, #6489, #40565, .T. ) ;
#37667 = CARTESIAN_POINT ( 'NONE',  ( 17.99999999999999645, 0.000000000000000000, 0.000000000000000000 ) ) ;
#37669 = ORIENTED_EDGE ( 'NONE', *, *, #23798, .F. ) ;
#37668 = DIRECTION ( 'NONE',  ( -1.000000000000000000, -0.000000000000000000, -0.000000000000000000 ) ) ;
#37670 = DIRECTION ( 'NONE',  ( -1.000000000000000000, 0.000000000000000000, 0.000000000000000000 ) ) ;
#37671 = VERTEX_POINT ( 'NONE', #37310 ) ;
#37672 = CARTESIAN_POINT ( 'NONE',  ( 8.999999999999998224, 73.51007459736548810, -89.73443560133290475 ) ) ;
#37673 = CARTESIAN_POINT ( 'NONE',  ( -31.57754862722326905, 40.00000000000000000, 93.01713655900283584 ) ) ;
#37674 = DIRECTION ( 'NONE',  ( -1.000000000000000000, -0.000000000000000000, 0.000000000000000000 ) ) ;
#37675 = ORIENTED_EDGE ( 'NONE', *, *, #14629, .F. ) ;
#37676 = AXIS2_PLACEMENT_3D ( 'NONE', #8038, #34014, #18133 ) ;
#37677 = CYLINDRICAL_SURFACE ( 'NONE', #29727, 36.00000000000000000 ) ;
#37678 = LINE ( 'NONE', #11755, #12732 ) ;
#37679 = AXIS2_PLACEMENT_3D ( 'NONE', #33720, #30477, #40471 ) ;
#37680 = VERTEX_POINT ( 'NONE', #7425 ) ;
#37681 = DIRECTION ( 'NONE',  ( -1.000000000000000000, -0.000000000000000000, 0.000000000000000000 ) ) ;
#37684 = ORIENTED_EDGE ( 'NONE', *, *, #26503, .F. ) ;
#37683 = EDGE_CURVE ( 'NONE', #8515, #21935, #22355, .T. ) ;
#37682 = VECTOR ( 'NONE', #32807, 1000.000000000000000 ) ;
#37685 = DIRECTION ( 'NONE',  ( 0.000000000000000000, 0.000000000000000000, 1.000000000000000000 ) ) ;
#37686 = CARTESIAN_POINT ( 'NONE',  ( -22.00208165626150603, 40.00000000000000000, -25.16137218361809857 ) ) ;
#37687 = DIRECTION ( 'NONE',  ( -1.000000000000000000, 0.000000000000000000, 0.000000000000000000 ) ) ;
#37688 = EDGE_CURVE ( 'NONE', #2641, #35377, #29303, .T. ) ;
#37689 = CARTESIAN_POINT ( 'NONE',  ( 0.000000000000000000, 37.91532898920961969, -28.61088654061597936 ) ) ;
#37690 = AXIS2_PLACEMENT_3D ( 'NONE', #741, #20660, #13235 ) ;
#37691 = FACE_OUTER_BOUND ( 'NONE', #1238, .T. ) ;
#37692 = VERTEX_POINT ( 'NONE', #24271 ) ;
#37694 = CARTESIAN_POINT ( 'NONE',  ( 1.360585162435110629, -4.061296242128317857, -3.505054077164905024 ) ) ;
#37693 = LINE ( 'NONE', #7812, #12678 ) ;
#37695 = EDGE_LOOP ( 'NONE', ( #7802, #31042 ) ) ;
#37696 = CIRCLE ( 'NONE', #35601, 13.59999999999999964 ) ;
#37697 = DIRECTION ( 'NONE',  ( 1.000000000000000000, 1.836909530733573776E-16, 0.000000000000000000 ) ) ;
#37698 = CARTESIAN_POINT ( 'NONE',  ( -29.89583333557403222, 31.00000000000000355, 1.963495399902740690 ) ) ;
#37699 = ORIENTED_EDGE ( 'NONE', *, *, #29587, .F. ) ;
#37700 = DIRECTION ( 'NONE',  ( 0.000000000000000000, -0.9957341762950355779, 0.09226835946329130234 ) ) ;
#37701 = CYLINDRICAL_SURFACE ( 'NONE', #22, 120.5010000000000190 ) ;
#37702 = ITEM_DEFINED_TRANSFORMATION ( 'NONE', 'NONE', #4447,  #13552 ) ;
#37703 = ADVANCED_FACE ( 'NONE', ( #7638 ), #7854, .T. ) ;
#37704 = CARTESIAN_POINT ( 'NONE',  ( 4.000000000000000000, -2.309401076758516691, -0.4999999999999995559 ) ) ;
#37705 = CARTESIAN_POINT ( 'NONE',  ( -76.41092972884307244, 31.00000000000000711, -25.93877460596726436 ) ) ;
#37706 = ORIENTED_EDGE ( 'NONE', *, *, #3804, .T. ) ;
#37707 = CARTESIAN_POINT ( 'NONE',  ( -39.38196478161825809, 31.00000000000000355, 13.29643045357694398 ) ) ;
#37708 = CARTESIAN_POINT ( 'NONE',  ( -70.15350862410126354, 40.00000000000000711, -40.50401079722123399 ) ) ;
#37709 = EDGE_CURVE ( 'NONE', #35369, #31353, #17720, .T. ) ;
#37710 = AXIS2_PLACEMENT_3D ( 'NONE', #22762, #42126, #16202 ) ;
#37711 = DIRECTION ( 'NONE',  ( -1.000000000000000000, -0.000000000000000000, 0.000000000000000000 ) ) ;
#37712 = AXIS2_PLACEMENT_3D ( 'NONE', #15560, #28855, #33397 ) ;
#37713 = CARTESIAN_POINT ( 'NONE',  ( 0.000000000000000000, 0.000000000000000000, 0.000000000000000000 ) ) ;
#37714 = ADVANCED_FACE ( 'NONE', ( #15942 ), #39018, .F. ) ;
#37715 = CARTESIAN_POINT ( 'NONE',  ( 0.000000000000000000, 80.02407177073062883, -78.64108602299866391 ) ) ;
#37717 = EDGE_LOOP ( 'NONE', ( #27616, #24467, #32521, #16977 ) ) ;
#37716 = CARTESIAN_POINT ( 'NONE',  ( -126.0000000000000000, 1.230603612181083142E-13, -40.00000000000002842 ) ) ;
#37718 = EDGE_CURVE ( 'NONE', #22420, #27172, #5587, .T. ) ;
#37719 = DIRECTION ( 'NONE',  ( 0.000000000000000000, 0.000000000000000000, 1.000000000000000000 ) ) ;
#37720 = CARTESIAN_POINT ( 'NONE',  ( 9.000000000000001776, 112.5220807139887853, -28.19186676675729331 ) ) ;
#37721 = VERTEX_POINT ( 'NONE', #12450 ) ;
#37722 = CARTESIAN_POINT ( 'NONE',  ( -17.60292107714122878, 40.00000000000000000, 65.74579412301164894 ) ) ;
#37723 = DIRECTION ( 'NONE',  ( -1.000000000000000000, 0.000000000000000000, -0.000000000000000000 ) ) ;
#37724 = DIRECTION ( 'NONE',  ( 0.000000000000000000, 0.000000000000000000, 1.000000000000000000 ) ) ;
#37725 = AXIS2_PLACEMENT_3D ( 'NONE', #38925, #36079, #19333 ) ;
#37726 = ORIENTED_EDGE ( 'NONE', *, *, #14546, .F. ) ;
#37727 = CARTESIAN_POINT ( 'NONE',  ( 17.99999999999999645, 0.000000000000000000, 0.000000000000000000 ) ) ;
#37728 = CARTESIAN_POINT ( 'NONE',  ( 17.99999999999999645, -0.6819280456836842585, 115.9979955608738607 ) ) ;
#37729 = EDGE_LOOP ( 'NONE', ( #5976, #15172, #3434, #19911 ) ) ;
#37730 = DIRECTION ( 'NONE',  ( 1.000000000000000000, 0.000000000000000000, 0.000000000000000000 ) ) ;
#37731 = ORIENTED_EDGE ( 'NONE', *, *, #39655, .F. ) ;
#37732 = DIRECTION ( 'NONE',  ( -1.000000000000000000, 0.000000000000000000, 0.000000000000000000 ) ) ;
#37733 = ORIENTED_EDGE ( 'NONE', *, *, #32301, .T. ) ;
#37734 = DIRECTION ( 'NONE',  ( -1.000000000000000000, -0.000000000000000000, -0.000000000000000000 ) ) ;
#37735 = FACE_OUTER_BOUND ( 'NONE', #30192, .T. ) ;
#37736 = ORIENTED_EDGE ( 'NONE', *, *, #38389, .F. ) ;
#37737 = EDGE_CURVE ( 'NONE', #21959, #6529, #18195, .T. ) ;
#37738 = B_SPLINE_CURVE_WITH_KNOTS ( 'NONE', 3,
 ( #20379, #33225, #20830, #33644, #26687, #30392, #39953, #3518 ),
 .UNSPECIFIED., .F., .F.,
 ( 4, 2, 2, 4 ),
 ( 2.465131517075058656E-07, 0.001183067374689851080, 0.001774477805458923299, 0.002365888236227995517 ),
 .UNSPECIFIED. ) ;
#37739 = EDGE_CURVE ( 'NONE', #35216, #18335, #15411, .T. ) ;
#37740 = FACE_OUTER_BOUND ( 'NONE', #17867, .T. ) ;
#37741 = FACE_OUTER_BOUND ( 'NONE', #12929, .T. ) ;
#37742 = EDGE_LOOP ( 'NONE', ( #25682, #25665, #5777, #32910 ) ) ;
#37743 = FACE_OUTER_BOUND ( 'NONE', #20672, .T. ) ;
#37744 = CIRCLE ( 'NONE', #7096, 58.99999999999999289 ) ;
#37745 = AXIS2_PLACEMENT_3D ( 'NONE', #6034, #13039, #18969 ) ;
#37746 = CARTESIAN_POINT ( 'NONE',  ( 17.99999999999999645, -5.456439917444183330, -112.0647122740742390 ) ) ;
#37747 = DIRECTION ( 'NONE',  ( 1.000000000000000000, 0.000000000000000000, 0.000000000000000000 ) ) ;
#37748 = AXIS2_PLACEMENT_3D ( 'NONE', #33596, #3676, #10693 ) ;
#37749 = FACE_OUTER_BOUND ( 'NONE', #1074, .T. ) ;
#37750 = EDGE_LOOP ( 'NONE', ( #36424, #39755, #9002, #18430 ) ) ;
#37751 = DIRECTION ( 'NONE',  ( 0.6795228977073574095, -2.224984581620894522E-17, -0.7336542997157423640 ) ) ;
#37752 = DIRECTION ( 'NONE',  ( 0.000000000000000000, 0.000000000000000000, 1.000000000000000000 ) ) ;
#37753 = ADVANCED_FACE ( 'NONE', ( #12653 ), #15722, .F. ) ;
#37754 = CARTESIAN_POINT ( 'NONE',  ( -13.53264355869793967, 31.00000000000000355, -39.83251807627727459 ) ) ;
#37755 = CIRCLE ( 'NONE', #25258, 2.041999999999999815 ) ;
#37756 = ORIENTED_EDGE ( 'NONE', *, *, #11650, .F. ) ;
#37758 = CARTESIAN_POINT ( 'NONE',  ( 0.000000000000000000, 89.07460286905958924, -81.15544420874873310 ) ) ;
#37757 = DIRECTION ( 'NONE',  ( 0.000000000000000000, 0.000000000000000000, 1.000000000000000000 ) ) ;
#37759 = DIRECTION ( 'NONE',  ( -1.000000000000000000, 0.000000000000000000, 0.000000000000000000 ) ) ;
#37760 = ORIENTED_EDGE ( 'NONE', *, *, #19099, .T. ) ;
#37761 = DIRECTION ( 'NONE',  ( 1.000000000000000000, 0.000000000000000000, 0.000000000000000000 ) ) ;
#37762 = CARTESIAN_POINT ( 'NONE',  ( -49.89583333467011528, 40.00000000000000000, 3.272492339034415831 ) ) ;
#37763 = CARTESIAN_POINT ( 'NONE',  ( 50.61746024623599993, 40.00000000000000000, -24.85206051842255093 ) ) ;
#37764 = EDGE_CURVE ( 'NONE', #27281, #37276, #32766, .T. ) ;
#37765 = DIRECTION ( 'NONE',  ( 0.000000000000000000, 0.000000000000000000, 1.000000000000000000 ) ) ;
#37766 = CARTESIAN_POINT ( 'NONE',  ( 0.000000000000000000, 0.000000000000000000, 0.000000000000000000 ) ) ;
#37767 = EDGE_CURVE ( 'NONE', #8604, #33622, #34867, .T. ) ;
#37768 = CARTESIAN_POINT ( 'NONE',  ( 17.99999999999999645, -24.22031524825905890, -109.5520369638039710 ) ) ;
#37769 = FACE_OUTER_BOUND ( 'NONE', #27804, .T. ) ;
#37770 = VECTOR ( 'NONE', #13526, 1000.000000000000000 ) ;
#37771 = ORIENTED_EDGE ( 'NONE', *, *, #7404, .T. ) ;
#37772 = CARTESIAN_POINT ( 'NONE',  ( -13.09503298281258132, 40.00000000000000000, -17.05789676611946959 ) ) ;
#37773 = ORIENTED_EDGE ( 'NONE', *, *, #42785, .F. ) ;
#37774 = FACE_OUTER_BOUND ( 'NONE', #16844, .T. ) ;
#37775 = CARTESIAN_POINT ( 'NONE',  ( -4.175648173966055587, 2.207990556236529844, -3.469390959564062626 ) ) ;
#37776 = VECTOR ( 'NONE', #17100, 1000.000000000000000 ) ;
#37777 = ORIENTED_EDGE ( 'NONE', *, *, #35593, .F. ) ;
#37778 = FACE_OUTER_BOUND ( 'NONE', #33823, .T. ) ;
#37779 = VECTOR ( 'NONE', #5648, 1000.000000000000000 ) ;
#37780 = CARTESIAN_POINT ( 'NONE',  ( 0.000000000000000000, 31.94619804602764290, 16.59639811537368814 ) ) ;
#37781 = ORIENTED_EDGE ( 'NONE', *, *, #6183, .T. ) ;
#37782 = PLANE ( 'NONE',  #13784 ) ;
#37783 = VERTEX_POINT ( 'NONE', #22496 ) ;
#37784 = AXIS2_PLACEMENT_3D ( 'NONE', #1528, #5241, #11374 ) ;
#37785 = ORIENTED_EDGE ( 'NONE', *, *, #21848, .T. ) ;
#37786 = DIRECTION ( 'NONE',  ( -1.000000000000000000, 0.000000000000000000, -0.000000000000000000 ) ) ;
#37787 = EDGE_CURVE ( 'NONE', #20272, #31337, #21681, .T. ) ;
#37788 = CARTESIAN_POINT ( 'NONE',  ( -18.22940504111061344, 31.00000000000000355, 67.64968002090884625 ) ) ;
#37789 = ORIENTED_EDGE ( 'NONE', *, *, #3139, .F. ) ;
#37790 = DIRECTION ( 'NONE',  ( -1.000000000000000000, -0.000000000000000000, 0.000000000000000000 ) ) ;
#37791 = EDGE_CURVE ( 'NONE', #25035, #235, #8395, .T. ) ;
#37792 = EDGE_CURVE ( 'NONE', #5751, #42039, #38811, .T. ) ;
#37793 = EDGE_CURVE ( 'NONE', #20704, #28489, #20265, .T. ) ;
#37794 = DIRECTION ( 'NONE',  ( 1.000000000000000000, 0.000000000000000000, 0.000000000000000000 ) ) ;
#37795 = VERTEX_POINT ( 'NONE', #1952 ) ;
#37796 = CARTESIAN_POINT ( 'NONE',  ( -4.211140560182196957, 2.431303136016537803, -3.745885042887433514 ) ) ;
#37797 = EDGE_LOOP ( 'NONE', ( #41621, #26803, #3257, #1512 ) ) ;
#37798 = CARTESIAN_POINT ( 'NONE',  ( 76.36627019849126441, 39.99999999999999289, -58.43797548694632127 ) ) ;
#37800 = FACE_OUTER_BOUND ( 'NONE', #20469, .T. ) ;
#37799 = DIRECTION ( 'NONE',  ( 0.000000000000000000, 0.000000000000000000, 1.000000000000000000 ) ) ;
#37801 = DIRECTION ( 'NONE',  ( -1.000000000000000000, -0.000000000000000000, -0.000000000000000000 ) ) ;
#37802 = CYLINDRICAL_SURFACE ( 'NONE', #34006, 59.00000000000000000 ) ;
#37803 = ORIENTED_EDGE ( 'NONE', *, *, #2891, .T. ) ;
#37804 = AXIS2_PLACEMENT_3D ( 'NONE', #10228, #13748, #27052 ) ;
#37805 = CARTESIAN_POINT ( 'NONE',  ( 17.99999999999999645, 118.8387007424470738, 19.94628303336527608 ) ) ;
#37806 = ORIENTED_EDGE ( 'NONE', *, *, #16249, .T. ) ;
#37807 = CARTESIAN_POINT ( 'NONE',  ( 17.99999999999999645, 64.58410930313523579, 101.7319213743684685 ) ) ;
#37808 = CARTESIAN_POINT ( 'NONE',  ( 43.43872713698582544, 31.00000000000000355, 75.20828420317944563 ) ) ;
#37809 = FACE_OUTER_BOUND ( 'NONE', #42619, .T. ) ;
#37810 = VERTEX_POINT ( 'NONE', #9351 ) ;
#37811 = CIRCLE ( 'NONE', #23901, 20.00000000000000711 ) ;
#37812 = CARTESIAN_POINT ( 'NONE',  ( -23.27229071022945561, 40.00000000000000000, 20.35677778009942074 ) ) ;
#37813 = VECTOR ( 'NONE', #38604, 1000.000000000000000 ) ;
#37814 = ORIENTED_EDGE ( 'NONE', *, *, #22788, .F. ) ;
#37815 = ORIENTED_EDGE ( 'NONE', *, *, #1573, .F. ) ;
#37816 = DIRECTION ( 'NONE',  ( -1.000000000000000000, -0.000000000000000000, 0.000000000000000000 ) ) ;
#37817 = CARTESIAN_POINT ( 'NONE',  ( 17.99999999999999645, 111.7974656912330005, 9.465682155095883843 ) ) ;
#37818 = DIRECTION ( 'NONE',  ( 3.009274222672345096E-17, 1.000000000000000000, -2.455023325076455345E-18 ) ) ;
#37819 = CARTESIAN_POINT ( 'NONE',  ( 8.999999999999998224, 0.000000000000000000, 0.000000000000000000 ) ) ;
#37820 = B_SPLINE_CURVE_WITH_KNOTS ( 'NONE', 3,
 ( #20491, #3197, #29877, #33758, #23550, #10427, #13936, #7356 ),
 .UNSPECIFIED., .F., .F.,
 ( 4, 2, 2, 4 ),
 ( 2.465131517071610173E-07, 0.001183067374689837636, 0.001774477805458902699, 0.002365888236227967761 ),
 .UNSPECIFIED. ) ;
#37821 = ORIENTED_EDGE ( 'NONE', *, *, #10567, .F. ) ;
#37822 = DIRECTION ( 'NONE',  ( 1.000000000000000000, 0.000000000000000000, 0.000000000000000000 ) ) ;
#37823 = ORIENTED_EDGE ( 'NONE', *, *, #12975, .F. ) ;
#37824 = DIRECTION ( 'NONE',  ( 0.000000000000000000, -0.7865515558026354714, -0.6175246149462008116 ) ) ;
#37825 = CARTESIAN_POINT ( 'NONE',  ( 0.000000000000000000, 0.000000000000000000, -6.000000000000000000 ) ) ;
#37826 = CARTESIAN_POINT ( 'NONE',  ( 0.000000000000000000, 32.49609705003704363, 15.49205204337285657 ) ) ;
#37827 = DIRECTION ( 'NONE',  ( -1.000000000000000000, -0.000000000000000000, 0.000000000000000000 ) ) ;
#37828 = ORIENTED_EDGE ( 'NONE', *, *, #34378, .F. ) ;
#37829 = ORIENTED_EDGE ( 'NONE', *, *, #16329, .F. ) ;
#37830 = DIRECTION ( 'NONE',  ( -3.996523416598930318E-16, 2.658563593772947863E-15, 1.000000000000000000 ) ) ;
#37831 = FACE_OUTER_BOUND ( 'NONE', #7016, .T. ) ;
#37832 = ORIENTED_EDGE ( 'NONE', *, *, #14006, .T. ) ;
#37834 = ORIENTED_EDGE ( 'NONE', *, *, #36514, .F. ) ;
#37833 = CARTESIAN_POINT ( 'NONE',  ( 17.99999999999999645, 5.822172717930266472, 31.41458249383143198 ) ) ;
#37835 = CARTESIAN_POINT ( 'NONE',  ( 2.996940313443769099, 31.00000000000000355, -44.59688583547567475 ) ) ;
#37836 = CARTESIAN_POINT ( 'NONE',  ( 0.000000000000000000, 0.6168405712486755288, 35.99471499692226928 ) ) ;
#37837 = EDGE_CURVE ( 'NONE', #10944, #33553, #35736, .T. ) ;
#37838 = EDGE_CURVE ( 'NONE', #12073, #16328, #13989, .T. ) ;
#37840 = DIRECTION ( 'NONE',  ( -1.000000000000000000, 0.000000000000000000, 0.000000000000000000 ) ) ;
#37839 = CARTESIAN_POINT ( 'NONE',  ( 18.00000000000000355, 0.000000000000000000, 0.000000000000000000 ) ) ;
#37841 = ADVANCED_FACE ( 'NONE', ( #8942 ), #18596, .F. ) ;
#37842 = ORIENTED_EDGE ( 'NONE', *, *, #30603, .T. ) ;
#37843 = DIRECTION ( 'NONE',  ( -1.000000000000000000, -0.000000000000000000, -0.000000000000000000 ) ) ;
#37844 = CARTESIAN_POINT ( 'NONE',  ( 8.570044366896553356, 40.00000000000000000, -64.27561742002654910 ) ) ;
#37845 = CARTESIAN_POINT ( 'NONE',  ( 17.99999999999999645, 30.71634675606053833, 8.790889055186667633 ) ) ;
#37846 = CARTESIAN_POINT ( 'NONE',  ( 0.000000000000000000, 111.2559044912524939, 32.83479428644713494 ) ) ;
#37847 = ORIENTED_EDGE ( 'NONE', *, *, #33215, .T. ) ;
#37848 = DIRECTION ( 'NONE',  ( -1.000000000000000000, -0.000000000000000000, -0.000000000000000000 ) ) ;
#37849 = ADVANCED_FACE ( 'NONE', ( #41666 ), #11812, .F. ) ;
#37850 = ORIENTED_EDGE ( 'NONE', *, *, #20968, .F. ) ;
#37851 = DIRECTION ( 'NONE',  ( 0.000000000000000000, 0.000000000000000000, 1.000000000000000000 ) ) ;
#37852 = APPLICATION_CONTEXT ( 'automotive_design' ) ;
#37853 = FACE_OUTER_BOUND ( 'NONE', #36568, .T. ) ;
#37854 = FACE_OUTER_BOUND ( 'NONE', #10395, .T. ) ;
#37855 = EDGE_CURVE ( 'NONE', #22661, #19113, #38349, .T. ) ;
#37856 = CIRCLE ( 'NONE', #22584, 20.00000000000000355 ) ;
#37857 = CARTESIAN_POINT ( 'NONE',  ( -3.763366191185464782, 31.00000000000000355, 57.60416666550938203 ) ) ;
#37858 = FACE_OUTER_BOUND ( 'NONE', #17788, .T. ) ;
#37859 = VERTEX_POINT ( 'NONE', #35330 ) ;
#37860 = CIRCLE ( 'NONE', #14921, 59.00000000000000711 ) ;
#37861 = CARTESIAN_POINT ( 'NONE',  ( 9.000000000000001776, -36.06787431788703913, 37.45808914225474950 ) ) ;
#37862 = VERTEX_POINT ( 'NONE', #5454 ) ;
#37863 = AXIS2_PLACEMENT_3D ( 'NONE', #33804, #16841, #27492 ) ;
#37864 = CARTESIAN_POINT ( 'NONE',  ( 10.63353083439206870, 40.00000000000000000, -31.33693976183458219 ) ) ;
#37865 = ORIENTED_EDGE ( 'NONE', *, *, #13896, .F. ) ;
#37866 = CYLINDRICAL_SURFACE ( 'NONE', #8907, 51.99999999999999289 ) ;
#37867 = CARTESIAN_POINT ( 'NONE',  ( 0.000000000000000000, 68.63002662989875091, -93.51962064069435598 ) ) ;
#37868 = CARTESIAN_POINT ( 'NONE',  ( 22.12670472278668399, 31.00000000000000355, -82.16725659058067777 ) ) ;
#37869 = CARTESIAN_POINT ( 'NONE',  ( 22.12670472277728706, 40.00000000000000000, -82.16725659058069198 ) ) ;
#37870 = DIRECTION ( 'NONE',  ( 0.000000000000000000, -0.9968120070307509017, 0.07978610555307336094 ) ) ;
#37871 = COLOUR_RGB ( '', 0.31764706, 0.68627451, 0.89019608) ;
#37872 = ORIENTED_EDGE ( 'NONE', *, *, #32087, .T. ) ;
#37873 = DIRECTION ( 'NONE',  ( 0.000000000000000000, 0.9618256431728199329, -0.2736629900720800590 ) ) ;
#37874 = ORIENTED_EDGE ( 'NONE', *, *, #21615, .F. ) ;
#37875 = CIRCLE ( 'NONE', #7226, 13.59999999999999787 ) ;
#37876 = DIRECTION ( 'NONE',  ( -1.000000000000000000, 0.000000000000000000, -0.000000000000000000 ) ) ;
#37877 = CARTESIAN_POINT ( 'NONE',  ( -150.5000000000000284, -5.254679414958916394E-13, 10.00000000000000000 ) ) ;
#37879 = EDGE_LOOP ( 'NONE', ( #1943, #42339, #34916, #37653 ) ) ;
#37878 = LINE ( 'NONE', #41589, #9520 ) ;
#37880 = DIRECTION ( 'NONE',  ( -0.9470131699890049770, 0.000000000000000000, -0.3211947320043963550 ) ) ;
#37881 = ORIENTED_EDGE ( 'NONE', *, *, #12331, .F. ) ;
#37882 = CARTESIAN_POINT ( 'NONE',  ( 33.90854556226734218, -14.05525454449573175, -74.83297477053821467 ) ) ;
#37883 = CIRCLE ( 'NONE', #29521, 2.000000000000000888 ) ;
#37884 = CARTESIAN_POINT ( 'NONE',  ( -94.39576909109665337, 40.00000000000000711, 32.06004391471374504 ) ) ;
#37885 = CARTESIAN_POINT ( 'NONE',  ( 18.00000000000000355, 0.000000000000000000, 0.000000000000000000 ) ) ;
#37886 = ORIENTED_EDGE ( 'NONE', *, *, #17389, .T. ) ;
#37887 = DIRECTION ( 'NONE',  ( -1.000000000000000000, -0.000000000000000000, 0.000000000000000000 ) ) ;
#37888 = DIRECTION ( 'NONE',  ( -1.000000000000000000, -0.000000000000000000, -0.000000000000000000 ) ) ;
#37889 = AXIS2_PLACEMENT_3D ( 'NONE', #13111, #23153, #19028 ) ;
#37890 = ADVANCED_FACE ( 'NONE', ( #23343 ), #36605, .F. ) ;
#37892 = CARTESIAN_POINT ( 'NONE',  ( 0.000000000000000000, 0.000000000000000000, 0.000000000000000000 ) ) ;
#37891 = CARTESIAN_POINT ( 'NONE',  ( 17.99999999999999645, 18.25486108452625089, 25.66996392254279868 ) ) ;
#37893 = PRODUCT_DEFINITION ( 'UNKNOWN', '', #42068, #10393 ) ;
#37894 = CIRCLE ( 'NONE', #25393, 120.5010000000000332 ) ;
#37895 = ORIENTED_EDGE ( 'NONE', *, *, #39060, .T. ) ;
#37896 = LINE ( 'NONE', #32224, #294 ) ;
#37897 = ORIENTED_EDGE ( 'NONE', *, *, #36641, .T. ) ;
#37898 = FACE_OUTER_BOUND ( 'NONE', #27558, .T. ) ;
#37899 = CARTESIAN_POINT ( 'NONE',  ( -9.709369018688819963, 40.00000000000000000, 28.47525938324995920 ) ) ;
#37900 = CARTESIAN_POINT ( 'NONE',  ( 17.99999999999999645, -97.89532456239533076, 54.81585448086167389 ) ) ;
#37901 = ADVANCED_FACE ( 'NONE', ( #6499 ), #705, .T. ) ;
#37902 = DIRECTION ( 'NONE',  ( 3.009274222672345096E-17, 1.000000000000000000, -2.455023325076455345E-18 ) ) ;
#37903 = ORIENTED_EDGE ( 'NONE', *, *, #8169, .T. ) ;
#37906 = CARTESIAN_POINT ( 'NONE',  ( 4.175648173966055587, -2.207990556236547608, -3.469390959564065291 ) ) ;
#37905 = DIRECTION ( 'NONE',  ( -0.000000000000000000, -0.000000000000000000, 1.000000000000000000 ) ) ;
#37904 = PRODUCT_DEFINITION_FORMATION_WITH_SPECIFIED_SOURCE ( 'ANY', '', #3607, .NOT_KNOWN. ) ;
#37907 = EDGE_CURVE ( 'NONE', #39944, #4717, #30704, .T. ) ;
#37908 = ORIENTED_EDGE ( 'NONE', *, *, #37837, .F. ) ;
#37909 = STYLED_ITEM ( 'NONE', ( #7589 ), #29166 ) ;
#37910 = DIRECTION ( 'NONE',  ( -1.000000000000000000, 0.000000000000000000, 0.000000000000000000 ) ) ;
#37911 = CYLINDRICAL_SURFACE ( 'NONE', #24808, 158.5000000000000284 ) ;
#37912 = EDGE_CURVE ( 'NONE', #10533, #3682, #26525, .T. ) ;
#37913 = CARTESIAN_POINT ( 'NONE',  ( 20.70971545910534672, 31.00000000000000355, 15.87948211774388518 ) ) ;
#37914 = EDGE_LOOP ( 'NONE', ( #9433, #14105, #19262, #10879 ) ) ;
#37915 = CARTESIAN_POINT ( 'NONE',  ( 0.000000000000000000, 24.47917365149946889, 45.87777302070943364 ) ) ;
#37916 = FACE_OUTER_BOUND ( 'NONE', #17220, .T. ) ;
#37917 = AXIS2_PLACEMENT_3D ( 'NONE', #26390, #19435, #23137 ) ;
#37918 = AXIS2_PLACEMENT_3D ( 'NONE', #31638, #28606, #11586 ) ;
#37919 = CARTESIAN_POINT ( 'NONE',  ( 47.90854556226721428, -2.055254544495724645, -74.83297477053847047 ) ) ;
#37920 = CARTESIAN_POINT ( 'NONE',  ( 80.16187752211510542, 31.00000000000000000, -27.22680903928618434 ) ) ;
#37921 = ORIENTED_EDGE ( 'NONE', *, *, #23973, .F. ) ;
#37922 = CARTESIAN_POINT ( 'NONE',  ( -40.56882557770292408, 31.00000000000000355, 31.01417895415301373 ) ) ;
#37923 = AXIS2_PLACEMENT_3D ( 'NONE', #31399, #34659, #28572 ) ;
#37924 = CARTESIAN_POINT ( 'NONE',  ( 74.49266661913014786, 39.99999999999999289, 43.00976416799198176 ) ) ;
#37925 = AXIS2_PLACEMENT_3D ( 'NONE', #33542, #23759, #33756 ) ;
#37926 = VERTEX_POINT ( 'NONE', #26173 ) ;
#37927 = EDGE_CURVE ( 'NONE', #23084, #42317, #33128, .T. ) ;
#37928 = CARTESIAN_POINT ( 'NONE',  ( 17.99999999999999645, 0.000000000000000000, 0.000000000000000000 ) ) ;
#37929 = DIRECTION ( 'NONE',  ( -1.000000000000000000, -0.000000000000000000, -0.000000000000000000 ) ) ;
#37930 = EDGE_CURVE ( 'NONE', #25212, #606, #24442, .T. ) ;
#37931 = DIRECTION ( 'NONE',  ( 1.000000000000000000, 0.000000000000000000, 0.000000000000000000 ) ) ;
#37933 = ORIENTED_EDGE ( 'NONE', *, *, #15871, .F. ) ;
#37932 = LINE ( 'NONE', #4789, #18191 ) ;
#37934 = CARTESIAN_POINT ( 'NONE',  ( 17.99999999999999645, -0.5156212287272186057, -112.1962860721878172 ) ) ;
#37935 = DIRECTION ( 'NONE',  ( -1.000000000000000000, 0.000000000000000000, 0.000000000000000000 ) ) ;
#37936 = VECTOR ( 'NONE', #42937, 1000.000000000000000 ) ;
#37937 = ORIENTED_EDGE ( 'NONE', *, *, #17308, .T. ) ;
#37938 = CARTESIAN_POINT ( 'NONE',  ( 52.51402048354923835, 40.00000000000000000, 40.27907379435107060 ) ) ;
#37939 = DIRECTION ( 'NONE',  ( -1.000000000000000000, -0.000000000000000000, -0.000000000000000000 ) ) ;
#37940 = EDGE_LOOP ( 'NONE', ( #23677, #23494, #40034, #71 ) ) ;
#37941 = DIRECTION ( 'NONE',  ( 0.000000000000000000, 0.000000000000000000, 1.000000000000000000 ) ) ;
#37942 = CARTESIAN_POINT ( 'NONE',  ( -4.000000000000000000, -1.942223658245633811, -0.3516579909967644246 ) ) ;
#37943 = CLOSED_SHELL ( 'NONE', ( #40412, #5755, #14698, #36448, #10983, #25967, #14292, #24439, #21783, #37040, #11539, #36137, #17794, #4391, #21656, #10493, #13662, #34085, #5638, #9720, #14753, #1945, #11669, #17254, #17844, #42906, #16191, #3414, #42907, #9812, #39585, #42502, #16978, #41768, #34599, #16370, #4112, #25718, #38548, #5778, #40163, #14985, #38309, #25239, #5857, #9687, #8012, #40333, #8828, #41668, #38785, #24739, #35133, #38464, #439, #42554, #22062, #19417, #27003, #26927, #42179, #34843, #504, #27535, #18074, #29451, #40648, #4508, #33273, #37303, #30322, #27300, #11100, #23273, #13977, #29432, #27684, #24548, #11208, #8447, #932, #20257, #6993, #25261, #39871, #43030, #26247, #8710, #36439, #14949, #2605, #18728, #29059, #16259, #41251, #32293, #7603, #4314, #7460, #14325, #7755, #34468, #38497, #19174, #17974, #25576, #8097, #14779, #34038, #32620, #14087, #9861, #31533, #19917, #14720, #6888, #5698, #37058, #40316, #42472, #34772, #40300, #5417, #20496, #12569, #7511, #11364, #19957, #40116, #38390, #19549, #37106, #24114, #13854, #23395, #4809, #35034, #33752, #13569, #25158, #12895, #13295, #22082, #11839, #20760, #35790, #23453, #38472, #22934, #15571, #14508, #306, #443, #25330, #17700, #24473, #6021, #41915, #9846, #34344, #32428, #21112, #9507, #34163, #19755, #25391, #39225, #30295, #10161, #13767, #31242, #27593, #30627, #16159, #16174, #30153, #18942, #41123, #22088, #17233, #1161, #36684, #35067, #38533, #36898, #31083, #12517, #21610, #33836, #21139, #3140, #4139, #1051, #10376, #13409, #40439, #12276, #31140, #23075, #29323, #38565, #19899, #14140, #21976, #22515, #42853, #43107, #18206, #25743, #22246, #38369, #3861, #3511, #36438, #12409, #36326, #22206, #4996, #20719, #19327, #13540, #5652, #1248, #8022, #35819, #42974, #5719, #12371, #7513, #25800, #41102, #34020, #25786, #3937, #14560, #6864, #33780, #26575, #30347, #36932, #33077, #38235, #2538, #30725, #5543, #35115, #33216, #2476, #38167, #27177, #21635, #18001, #12511, #36511, #7178, #4657, #1455, #9531, #5935, #30762, #4698, #32724, #23765, #31937, #24354, #2792, #2361, #24131, #1075, #41458, #40993, #20475, #36030, #12211, #28765, #31462, #42042, #1964, #32061, #26743, #11677, #10775, #19629, #6976, #1207, #8610, #25683, #7048, #12539, #29848, #40402, #31547, #23578, #11952, #6384, #28533, #12210, #36673, #32719, #5805, #19826, #27989, #4028, #19599, #38267, #34395, #8991, #29251, #2514, #25285, #23751, #20390, #19223, #4548, #32114, #20831, #1433, #18943, #32641, #28764, #42863, #2503, #19381, #8215, #26945, #18084, #18499, #15269, #37552, #42909, #5787, #25626, #36184, #8626, #20615, #20120, #38237, #34056, #14066, #10715, #11818, #30485, #31483, #41883, #20726, #34327, #42531, #1541, #13962, #22648, #17850, #41679, #26036, #36559, #9389, #13735, #31529, #33857, #30442, #39606, #3557, #29244, #10511, #22878, #32456, #33471, #30266, #2679, #12570, #2606, #42284, #29704, #8990, #5239, #16416, #25105, #2355, #4948, #13595, #37557, #23291, #37890, #10389, #6078, #16315, #3350, #22309, #40132, #176, #15725, #13624, #14825, #21208, #10795, #37661, #4978, #2997, #438, #39457, #22189, #38828, #35491, #12717, #26553, #2139, #22874, #31277, #38747, #18348, #33193, #20036, #39026, #42020, #35358, #1875, #4109, #13298, #1138, #1486, #417, #39469, #4603, #32550, #41720, #37122, #9374, #3535, #37753, #1992, #8322, #20155, #18447, #18459, #35755, #40227, #32938, #38974, #7266, #16366, #5242, #31109, #15712, #18826, #40733, #12024, #16502, #37528, #36874, #38927, #27678, #38822, #23700, #35598, #40060, #6581, #1040, #37841, #7289, #28193, #7455, #18349, #9585, #19955, #41683, #31411, #21661, #5440, #30843, #25031, #35642, #37714, #8983, #12123, #2026, #14183, #5027, #40987, #14528, #26580, #39839, #180 ) ) ;
#37944 = VERTEX_POINT ( 'NONE', #22939 ) ;
#37945 = CARTESIAN_POINT ( 'NONE',  ( 0.000000000000000000, -44.75336757549789013, 14.30704879393590012 ) ) ;
#37946 = EDGE_LOOP ( 'NONE', ( #7993, #14797, #1403, #25072 ) ) ;
#37947 = EDGE_CURVE ( 'NONE', #40464, #24642, #4937, .T. ) ;
#37948 = DIRECTION ( 'NONE',  ( -1.000000000000000000, 0.000000000000000000, -0.000000000000000000 ) ) ;
#37949 = ORIENTED_EDGE ( 'NONE', *, *, #18518, .F. ) ;
#37950 = CIRCLE ( 'NONE', #17093, 20.00000000000000355 ) ;
#37951 = CYLINDRICAL_SURFACE ( 'NONE', #1406, 59.00000000000000711 ) ;
#37952 = DIRECTION ( 'NONE',  ( 0.000000000000000000, -0.9957341762950334685, -0.09226835946331299332 ) ) ;
#37953 = VERTEX_POINT ( 'NONE', #29891 ) ;
#37954 = AXIS2_PLACEMENT_3D ( 'NONE', #114, #3402, #16770 ) ;
#37955 = FACE_OUTER_BOUND ( 'NONE', #21750, .T. ) ;
#37956 = CARTESIAN_POINT ( 'NONE',  ( 0.000000000000000000, 0.000000000000000000, 0.000000000000000000 ) ) ;
#37957 = VERTEX_POINT ( 'NONE', #10218 ) ;
#37958 = LINE ( 'NONE', #4356, #12032 ) ;
#37959 = EDGE_CURVE ( 'NONE', #12545, #32231, #21713, .T. ) ;
#37960 = AXIS2_PLACEMENT_3D ( 'NONE', #24136, #17387, #738 ) ;
#37961 = DIRECTION ( 'NONE',  ( -3.009274222672345096E-17, -1.000000000000000000, 2.455023325076455345E-18 ) ) ;
#37962 = VERTEX_POINT ( 'NONE', #17015 ) ;
#37963 = DIRECTION ( 'NONE',  ( 0.000000000000000000, 0.000000000000000000, 1.000000000000000000 ) ) ;
#37964 = DIRECTION ( 'NONE',  ( 1.000000000000000000, 0.000000000000000000, 0.000000000000000000 ) ) ;
#37965 = VERTEX_POINT ( 'NONE', #23776 ) ;
#37967 = CIRCLE ( 'NONE', #2407, 59.00000000000000000 ) ;
#37966 = DIRECTION ( 'NONE',  ( 4.329780281177519431E-17, 1.000000000000000000, 4.329780281177414044E-17 ) ) ;
#37968 = DIRECTION ( 'NONE',  ( 1.000000000000000000, -0.000000000000000000, -0.000000000000000000 ) ) ;
#37969 = CARTESIAN_POINT ( 'NONE',  ( 45.10416666515585860, 31.00000000000000355, 2.945243104263102651 ) ) ;
#37970 = ORIENTED_EDGE ( 'NONE', *, *, #11865, .T. ) ;
#37972 = CARTESIAN_POINT ( 'NONE',  ( 2.600000000000000533, -12.75000000000000000, -1.199999999999999956 ) ) ;
#37971 = CARTESIAN_POINT ( 'NONE',  ( -81.46080130434573618, -34.05525454449571043, 14.45886780445633946 ) ) ;
#37973 = DIRECTION ( 'NONE',  ( 0.000000000000000000, 0.000000000000000000, 1.000000000000000000 ) ) ;
#37974 = ORIENTED_EDGE ( 'NONE', *, *, #11991, .F. ) ;
#37975 = FACE_OUTER_BOUND ( 'NONE', #6652, .T. ) ;
#37976 = CARTESIAN_POINT ( 'NONE',  ( -18.68892229297488683, 40.00000000000000000, 55.06009237583231197 ) ) ;
#37977 = VECTOR ( 'NONE', #40255, 1000.000000000000114 ) ;
#37978 = CARTESIAN_POINT ( 'NONE',  ( 55.55275676651330485, 40.00000000000000000, 14.97830846782891712 ) ) ;
#37979 = ADVANCED_FACE ( 'NONE', ( #13738 ), #39445, .F. ) ;
#37980 = VECTOR ( 'NONE', #6480, 1000.000000000000000 ) ;
#37981 = CARTESIAN_POINT ( 'NONE',  ( -10.00000000000000000, 0.000000000000000000, 0.000000000000000000 ) ) ;
#37982 = LINE ( 'NONE', #31461, #17291 ) ;
#37983 = EDGE_CURVE ( 'NONE', #23828, #41341, #27159, .T. ) ;
#37984 = AXIS2_PLACEMENT_3D ( 'NONE', #1601, #21938, #25216 ) ;
#37985 = DIRECTION ( 'NONE',  ( 0.000000000000000000, -0.4817536741017035551, -0.8763066800438700232 ) ) ;
#37986 = DIRECTION ( 'NONE',  ( -1.000000000000000000, 0.000000000000000000, 0.000000000000000000 ) ) ;
#37987 = AXIS2_PLACEMENT_3D ( 'NONE', #35629, #11899, #5745 ) ;
#37988 = ORIENTED_EDGE ( 'NONE', *, *, #23463, .T. ) ;
#37989 = CARTESIAN_POINT ( 'NONE',  ( -9.824444021593908616, 40.00000000000000000, 36.70529466175499778 ) ) ;
#37990 = ORIENTED_EDGE ( 'NONE', *, *, #32529, .T. ) ;
#37991 = CARTESIAN_POINT ( 'NONE',  ( 17.99999999999999645, -0.6168405712489235526, 35.99471499692226928 ) ) ;
#37992 = DIRECTION ( 'NONE',  ( 1.000000000000000000, 0.000000000000000000, 0.000000000000000000 ) ) ;
#37993 = ORIENTED_EDGE ( 'NONE', *, *, #35496, .F. ) ;
#37994 = DIRECTION ( 'NONE',  ( 0.000000000000000000, 0.000000000000000000, 1.000000000000000000 ) ) ;
#37995 = CARTESIAN_POINT ( 'NONE',  ( 1.600000000000000089, -12.75000000000000000, 0.000000000000000000 ) ) ;
#37996 = ORIENTED_EDGE ( 'NONE', *, *, #19396, .T. ) ;
#37997 = DIRECTION ( 'NONE',  ( 0.000000000000000000, 0.000000000000000000, 1.000000000000000000 ) ) ;
#37998 = VERTEX_POINT ( 'NONE', #16593 ) ;
#37999 = EDGE_CURVE ( 'NONE', #28176, #39148, #32802, .T. ) ;
#38000 = ORIENTED_EDGE ( 'NONE', *, *, #23595, .T. ) ;
#38001 = DIRECTION ( 'NONE',  ( 0.000000000000000000, 0.000000000000000000, 1.000000000000000000 ) ) ;
#38002 = CARTESIAN_POINT ( 'NONE',  ( -9.228224334391116557, 31.00000000000000355, 69.24269282083176336 ) ) ;
#38003 = ORIENTED_EDGE ( 'NONE', *, *, #41186, .T. ) ;
#38004 = CARTESIAN_POINT ( 'NONE',  ( -4.211399284164270895, 2.459729995988205964, -3.751162237960538715 ) ) ;
#38005 = CIRCLE ( 'NONE', #27569, 20.00000000000000711 ) ;
#38007 = DIRECTION ( 'NONE',  ( 0.000000000000000000, 0.7980172272802363853, 0.6026346363792605132 ) ) ;
#38006 = CIRCLE ( 'NONE', #33835, 13.60000000000000142 ) ;
#38008 = VERTEX_POINT ( 'NONE', #36177 ) ;
#38009 = TOROIDAL_SURFACE ( 'NONE', #40766, 5.384454397937118664, 0.5155456020628804703 ) ;
#38010 = CARTESIAN_POINT ( 'NONE',  ( -10.00000000000000000, 0.000000000000000000, 0.000000000000000000 ) ) ;
#38011 = EDGE_CURVE ( 'NONE', #606, #41289, #639, .T. ) ;
#38012 = ORIENTED_EDGE ( 'NONE', *, *, #9986, .F. ) ;
#38013 = CARTESIAN_POINT ( 'NONE',  ( 86.58052584568750376, 39.99999999999999289, -42.55516686010646765 ) ) ;
#38014 = CARTESIAN_POINT ( 'NONE',  ( 3.798394181603659270, 31.00000000000000355, 29.10671710469610574 ) ) ;
#38015 = EDGE_CURVE ( 'NONE', #11580, #1632, #33487, .T. ) ;
#38017 = CARTESIAN_POINT ( 'NONE',  ( 18.00000000000000355, 0.000000000000000000, 0.000000000000000000 ) ) ;
#38016 = LINE ( 'NONE', #28020, #2878 ) ;
#38018 = AXIS2_PLACEMENT_3D ( 'NONE', #1052, #40757, #31196 ) ;
#38019 = CIRCLE ( 'NONE', #19248, 116.0000000000000000 ) ;
#38020 = CARTESIAN_POINT ( 'NONE',  ( 5.000000000000000888, 0.000000000000000000, 0.000000000000000000 ) ) ;
#38021 = DIRECTION ( 'NONE',  ( -1.000000000000000000, 3.035766082959410566E-17, 0.000000000000000000 ) ) ;
#38022 = ORIENTED_EDGE ( 'NONE', *, *, #19237, .F. ) ;
#38023 = PRESENTATION_STYLE_ASSIGNMENT (( #23894 ) ) ;
#38024 = AXIS2_PLACEMENT_3D ( 'NONE', #35154, #5274, #18642 ) ;
#38025 = DIRECTION ( 'NONE',  ( 1.000000000000000000, 0.000000000000000000, 0.000000000000000000 ) ) ;
#38026 = ORIENTED_EDGE ( 'NONE', *, *, #39654, .F. ) ;
#38027 = DIRECTION ( 'NONE',  ( 1.000000000000000000, 0.000000000000000000, -0.000000000000000000 ) ) ;
#38028 = CARTESIAN_POINT ( 'NONE',  ( 94.89583333399441756, 31.00000000000000000, -6.217735451874103703 ) ) ;
#38029 = DIRECTION ( 'NONE',  ( 0.000000000000000000, -0.5528000653612000770, 0.8333139190825105125 ) ) ;
#38030 = ORIENTED_EDGE ( 'NONE', *, *, #23205, .F. ) ;
#38031 = CARTESIAN_POINT ( 'NONE',  ( -9.709369018688819963, 40.00000000000000000, 28.47525938324995920 ) ) ;
#38032 = ORIENTED_EDGE ( 'NONE', *, *, #21006, .F. ) ;
#38033 = EDGE_CURVE ( 'NONE', #30765, #16529, #24474, .T. ) ;
#38034 = ORIENTED_EDGE ( 'NONE', *, *, #40403, .T. ) ;
#38035 = DIRECTION ( 'NONE',  ( 0.000000000000000000, 0.000000000000000000, 1.000000000000000000 ) ) ;
#38036 = DIRECTION ( 'NONE',  ( -1.000000000000000000, 0.000000000000000000, 0.000000000000000000 ) ) ;
#38037 = ADVANCED_FACE ( 'NONE', ( #42709 ), #29662, .T. ) ;
#38039 = CARTESIAN_POINT ( 'NONE',  ( 18.00000000000000355, 0.000000000000000000, 0.000000000000000000 ) ) ;
#38038 = CIRCLE ( 'NONE', #4582, 51.99999999999999289 ) ;
#38040 = EDGE_CURVE ( 'NONE', #15479, #2864, #14715, .T. ) ;
#38041 = EDGE_CURVE ( 'NONE', #6092, #42889, #7808, .T. ) ;
#38042 = DIRECTION ( 'NONE',  ( 1.000000000000000000, 0.000000000000000000, 0.000000000000000000 ) ) ;
#38043 = VECTOR ( 'NONE', #14610, 1000.000000000000000 ) ;
#38044 = AXIS2_PLACEMENT_3D ( 'NONE', #19018, #22500, #15946 ) ;
#38045 = AXIS2_PLACEMENT_3D ( 'NONE', #16063, #29368, #22849 ) ;
#38046 = ORIENTED_EDGE ( 'NONE', *, *, #16442, .F. ) ;
#38047 = LINE ( 'NONE', #42157, #40244 ) ;
#38048 = ORIENTED_EDGE ( 'NONE', *, *, #9532, .T. ) ;
#38049 = DIRECTION ( 'NONE',  ( 1.000000000000000000, 0.000000000000000000, 0.000000000000000000 ) ) ;
#38050 = DIRECTION ( 'NONE',  ( -1.058513553088275437E-16, -1.000000000000000000, 8.813324511995299047E-17 ) ) ;
#38051 = VECTOR ( 'NONE', #15175, 1000.000000000000000 ) ;
#38052 = AXIS2_PLACEMENT_3D ( 'NONE', #13493, #32680, #2760 ) ;
#38053 = CARTESIAN_POINT ( 'NONE',  ( -15.99999999999997691, 40.00000000000000000, 5.571627607371296764E-15 ) ) ;
#38054 = VECTOR ( 'NONE', #6353, 1000.000000000000000 ) ;
#38055 = CYLINDRICAL_SURFACE ( 'NONE', #35859, 120.5010000000000190 ) ;
#38056 = EDGE_LOOP ( 'NONE', ( #10183, #33298, #13368, #25716 ) ) ;
#38057 = EDGE_LOOP ( 'NONE', ( #34427, #26023, #42023, #42403 ) ) ;
#38058 = DIRECTION ( 'NONE',  ( 0.000000000000000000, 0.000000000000000000, 1.000000000000000000 ) ) ;
#38059 = DIRECTION ( 'NONE',  ( 0.000000000000000000, 1.000000000000000000, 1.224646799147353207E-16 ) ) ;
#38060 = VECTOR ( 'NONE', #14430, 1000.000000000000000 ) ;
#38061 = ORIENTED_EDGE ( 'NONE', *, *, #19414, .F. ) ;
#38063 = ORIENTED_EDGE ( 'NONE', *, *, #496, .F. ) ;
#38062 = DIRECTION ( 'NONE',  ( 0.000000000000000000, -0.1837495178165569620, -0.9829730996839042279 ) ) ;
#38064 = CARTESIAN_POINT ( 'NONE',  ( -41.52979953746218911, 31.00000000000000355, 5.398177843165337109 ) ) ;
#38065 = LINE ( 'NONE', #27847, #11181 ) ;
#38067 = DIRECTION ( 'NONE',  ( -1.000000000000000000, 0.000000000000000000, 0.000000000000000000 ) ) ;
#38066 = CARTESIAN_POINT ( 'NONE',  ( -5.991980000000000750, 0.000000000000000000, 14.99999999999999822 ) ) ;
#38068 = EDGE_CURVE ( 'NONE', #12547, #36920, #24431, .T. ) ;
#38069 = ORIENTED_EDGE ( 'NONE', *, *, #20498, .T. ) ;
#38070 = DIRECTION ( 'NONE',  ( 0.000000000000000000, 0.000000000000000000, 1.000000000000000000 ) ) ;
#38071 = CARTESIAN_POINT ( 'NONE',  ( 66.90003082753170816, 39.99999999999999289, -4.275635516647131595 ) ) ;
#38072 = FACE_OUTER_BOUND ( 'NONE', #7171, .T. ) ;
#38073 = DIRECTION ( 'NONE',  ( 1.000000000000000000, 0.000000000000000000, 0.000000000000000000 ) ) ;
#38075 = ORIENTED_EDGE ( 'NONE', *, *, #42461, .F. ) ;
#38074 = CIRCLE ( 'NONE', #13003, 19.59999999999999076 ) ;
#38076 = CARTESIAN_POINT ( 'NONE',  ( 0.000000000000000000, 0.000000000000000000, 0.000000000000000000 ) ) ;
#38077 = VECTOR ( 'NONE', #23906, 1000.000000000000000 ) ;
#38078 = ORIENTED_EDGE ( 'NONE', *, *, #10436, .T. ) ;
#38079 = SURFACE_SIDE_STYLE ('',( #31339 ) ) ;
#38080 = VECTOR ( 'NONE', #40816, 1000.000000000000000 ) ;
#38081 = CARTESIAN_POINT ( 'NONE',  ( 153.1499999999986414, 1.392576523351516607E-12, 9.999999999999959144 ) ) ;
#38082 = CARTESIAN_POINT ( 'NONE',  ( 0.000000000000000000, 34.03109950475727175, 115.5957406979051285 ) ) ;
#38083 = CARTESIAN_POINT ( 'NONE',  ( -69.89583333424914713, 31.00000000000000711, 4.581489278091138040 ) ) ;
#38084 = CARTESIAN_POINT ( 'NONE',  ( 17.99999999999999645, 0.000000000000000000, 0.000000000000000000 ) ) ;
#38086 = ORIENTED_EDGE ( 'NONE', *, *, #38521, .T. ) ;
#38085 = VECTOR ( 'NONE', #15864, 1000.000000000000000 ) ;
#38088 = CIRCLE ( 'NONE', #29763, 20.00000000000000711 ) ;
#38087 = CARTESIAN_POINT ( 'NONE',  ( 17.99999999999999645, 0.000000000000000000, 0.000000000000000000 ) ) ;
#38089 = CIRCLE ( 'NONE', #11756, 20.00000000000000711 ) ;
#38090 = ORIENTED_EDGE ( 'NONE', *, *, #9611, .T. ) ;
#38091 = DIRECTION ( 'NONE',  ( 1.000000000000000000, -1.373900992973641277E-15, -5.551115123125812284E-16 ) ) ;
#38092 = CARTESIAN_POINT ( 'NONE',  ( 38.90854556226734218, -12.05525454449572997, -74.83297477053821467 ) ) ;
#38093 = CARTESIAN_POINT ( 'NONE',  ( -5.980347265640405752, 31.00000000000000355, 89.59238221257746204 ) ) ;
#38094 = CARTESIAN_POINT ( 'NONE',  ( 22.98560153735141043, 40.00000000000000000, 86.26083236265425569 ) ) ;
#38095 = ADVANCED_FACE ( 'NONE', ( #1464 ), #7371, .T. ) ;
#38096 = EDGE_CURVE ( 'NONE', #21731, #15816, #10416, .T. ) ;
#38097 = CARTESIAN_POINT ( 'NONE',  ( 2.500000000000000000, 1.178949249685217415, 2.041999999999998483 ) ) ;
#38098 = EDGE_CURVE ( 'NONE', #6854, #28114, #19506, .T. ) ;
#38099 = EDGE_LOOP ( 'NONE', ( #2154, #589, #1835, #5637 ) ) ;
#38100 = CARTESIAN_POINT ( 'NONE',  ( 17.99999999999999645, -5.456439917445724319, 112.0647122740741963 ) ) ;
#38101 = ORIENTED_EDGE ( 'NONE', *, *, #21468, .F. ) ;
#38102 = CARTESIAN_POINT ( 'NONE',  ( 18.00000000000000355, -6.109652351741465814, -46.58570277113515345 ) ) ;
#38103 = DIRECTION ( 'NONE',  ( -1.000000000000000000, -0.000000000000000000, -0.000000000000000000 ) ) ;
#38104 = CIRCLE ( 'NONE', #8155, 20.00000000000000711 ) ;
#38106 = VERTEX_POINT ( 'NONE', #4519 ) ;
#38105 = CARTESIAN_POINT ( 'NONE',  ( 106.4195705685763471, -106.4195705685744855, 10.00000000000000000 ) ) ;
#38107 = CYLINDRICAL_SURFACE ( 'NONE', #36513, 47.49900000000000233 ) ;
#38108 = ORIENTED_EDGE ( 'NONE', *, *, #21563, .F. ) ;
#38109 = CYLINDRICAL_SURFACE ( 'NONE', #39761, 116.0000000000000000 ) ;
#38110 = AXIS2_PLACEMENT_3D ( 'NONE', #15797, #12097, #22789 ) ;
#38111 = CARTESIAN_POINT ( 'NONE',  ( -60.37409795221152109, 40.00000000000000711, -68.82020352599361956 ) ) ;
#38112 = DIRECTION ( 'NONE',  ( 1.000000000000000000, 0.000000000000000000, 0.000000000000000000 ) ) ;
#38113 = CIRCLE ( 'NONE', #20034, 59.00000000000000000 ) ;
#38114 = CIRCLE ( 'NONE', #8162, 120.5010000000000332 ) ;
#38115 = ORIENTED_EDGE ( 'NONE', *, *, #27805, .F. ) ;
#38116 = ADVANCED_FACE ( 'NONE', ( #3858 ), #4754, .T. ) ;
#38117 = CARTESIAN_POINT ( 'NONE',  ( 8.999999999999998224, -101.1403355683142422, -56.80345518653591341 ) ) ;
#38118 = DIRECTION ( 'NONE',  ( -1.000000000000000000, 0.000000000000000000, -0.000000000000000000 ) ) ;
#38119 = AXIS2_PLACEMENT_3D ( 'NONE', #10062, #16654, #36020 ) ;
#38121 = DIRECTION ( 'NONE',  ( 3.009274222672345096E-17, 1.000000000000000000, -2.455023325076454960E-18 ) ) ;
#38120 = DIRECTION ( 'NONE',  ( -1.000000000000000000, 0.000000000000000000, -0.000000000000000000 ) ) ;
#38122 = ORIENTED_EDGE ( 'NONE', *, *, #21949, .F. ) ;
#38123 = CARTESIAN_POINT ( 'NONE',  ( 0.000000000000000000, 0.000000000000000000, 0.000000000000000000 ) ) ;
#38124 = ORIENTED_EDGE ( 'NONE', *, *, #1251, .T. ) ;
#38125 = CARTESIAN_POINT ( 'NONE',  ( 0.000000000000000000, -72.00556975657760006, 86.04342158279364128 ) ) ;
#38126 = CARTESIAN_POINT ( 'NONE',  ( -31.89861325429239258, 40.00000000000000000, 2.042328591206914012 ) ) ;
#38127 = CARTESIAN_POINT ( 'NONE',  ( 0.000000000000000000, 23.79363200506992015, -27.01597816121622486 ) ) ;
#38128 = CIRCLE ( 'NONE', #14456, 120.5010000000000190 ) ;
#38129 = DIRECTION ( 'NONE',  ( 1.000000000000000000, 0.000000000000000000, 0.000000000000000000 ) ) ;
#38130 = LINE ( 'NONE', #5178, #37356 ) ;
#38131 = VERTEX_POINT ( 'NONE', #28117 ) ;
#38132 = ADVANCED_FACE ( 'NONE', ( #11315 ), #31168, .T. ) ;
#38134 = CARTESIAN_POINT ( 'NONE',  ( 17.99999999999999645, -111.2721026680459602, 44.61974821237267719 ) ) ;
#38133 = CARTESIAN_POINT ( 'NONE',  ( 17.99999999999999645, 0.000000000000000000, 116.0000000000000000 ) ) ;
#38135 = ORIENTED_EDGE ( 'NONE', *, *, #8199, .F. ) ;
#38136 = DIRECTION ( 'NONE',  ( 0.000000000000000000, 0.000000000000000000, 1.000000000000000000 ) ) ;
#38137 = DIRECTION ( 'NONE',  ( -0.000000000000000000, -0.000000000000000000, 1.000000000000000000 ) ) ;
#38138 = CARTESIAN_POINT ( 'NONE',  ( -30.10416666442597844, 31.00000000000000355, -1.963495399902747574 ) ) ;
#38140 = ORIENTED_EDGE ( 'NONE', *, *, #9121, .F. ) ;
#38139 = AXIS2_PLACEMENT_3D ( 'NONE', #19785, #16733, #16515 ) ;
#38141 = FACE_OUTER_BOUND ( 'NONE', #41759, .T. ) ;
#38142 = AXIS2_PLACEMENT_3D ( 'NONE', #33212, #36462, #10307 ) ;
#38143 = CARTESIAN_POINT ( 'NONE',  ( 42.80287614962796994, -2.055254544495723756, 69.29271901957280022 ) ) ;
#38144 = CARTESIAN_POINT ( 'NONE',  ( 74.89583333416871369, 31.00000000000000000, -4.908738512848213276 ) ) ;
#38145 = AXIS2_PLACEMENT_3D ( 'NONE', #7210, #2846, #39927 ) ;
#38146 = CIRCLE ( 'NONE', #19375, 58.99999999999998579 ) ;
#38147 = CIRCLE ( 'NONE', #22156, 0.08402000000000062196 ) ;
#38148 = ORIENTED_EDGE ( 'NONE', *, *, #15377, .T. ) ;
#38150 = CARTESIAN_POINT ( 'NONE',  ( -15.62887661520211857, 31.00000000000000355, 57.97203279869351888 ) ) ;
#38149 = CIRCLE ( 'NONE', #38855, 2.499999999999999556 ) ;
#38151 = EDGE_CURVE ( 'NONE', #2586, #25188, #8424, .T. ) ;
#38152 = CARTESIAN_POINT ( 'NONE',  ( -90.10416666596678681, 40.00000000000000711, -5.890486217120279200 ) ) ;
#38153 = ORIENTED_EDGE ( 'NONE', *, *, #8965, .T. ) ;
#38154 = CARTESIAN_POINT ( 'NONE',  ( 0.000000000000000000, 0.000000000000000000, 0.000000000000000000 ) ) ;
#38155 = AXIS2_PLACEMENT_3D ( 'NONE', #38542, #15469, #31382 ) ;
#38156 = DIRECTION ( 'NONE',  ( 0.000000000000000000, 0.000000000000000000, -1.000000000000000000 ) ) ;
#38157 = DIRECTION ( 'NONE',  ( -1.000000000000000000, 0.000000000000000000, -0.000000000000000000 ) ) ;
#38159 = ORIENTED_EDGE ( 'NONE', *, *, #33140, .F. ) ;
#38158 = DIRECTION ( 'NONE',  ( 0.000000000000000000, 0.9714298932647090767, 0.2373266998711185127 ) ) ;
#38160 = CYLINDRICAL_SURFACE ( 'NONE', #11452, 20.00000000000000711 ) ;
#38161 = CARTESIAN_POINT ( 'NONE',  ( 18.00000000000000355, 13.85708833599968770, 45.43276465116669982 ) ) ;
#38162 = EDGE_CURVE ( 'NONE', #6244, #9154, #34895, .T. ) ;
#38163 = ORIENTED_EDGE ( 'NONE', *, *, #41388, .T. ) ;
#38164 = CARTESIAN_POINT ( 'NONE',  ( 64.37268382102905662, 39.99999999999999289, -8.487791176987355968 ) ) ;
#38165 = DIRECTION ( 'NONE',  ( -1.000000000000000000, -0.000000000000000000, -0.000000000000000000 ) ) ;
#38166 = ORIENTED_EDGE ( 'NONE', *, *, #19821, .T. ) ;
#38167 = ADVANCED_FACE ( 'NONE', ( #20950 ), #7594, .F. ) ;
#38168 = VECTOR ( 'NONE', #4230, 1000.000000000000000 ) ;
#38169 = CARTESIAN_POINT ( 'NONE',  ( -16.80298683001096904, 40.00000000000000000, -2.367532924972506336 ) ) ;
#38170 = CARTESIAN_POINT ( 'NONE',  ( 17.99999999999999645, -115.0622509503831452, -14.72000021165260897 ) ) ;
#38171 = VERTEX_POINT ( 'NONE', #37258 ) ;
#38172 = DIRECTION ( 'NONE',  ( 1.000000000000000000, 0.000000000000000000, 0.000000000000000000 ) ) ;
#38173 = VERTEX_POINT ( 'NONE', #38127 ) ;
#38174 = AXIS2_PLACEMENT_3D ( 'NONE', #24245, #34022, #4111 ) ;
#38175 = CIRCLE ( 'NONE', #6116, 10.50000000000000178 ) ;
#38176 = DIRECTION ( 'NONE',  ( -0.000000000000000000, -0.000000000000000000, -1.000000000000000000 ) ) ;
#38177 = ORIENTED_EDGE ( 'NONE', *, *, #15690, .T. ) ;
#38178 = CARTESIAN_POINT ( 'NONE',  ( 17.99999999999999645, 0.000000000000000000, 0.000000000000000000 ) ) ;
#38179 = DIRECTION ( 'NONE',  ( 1.000000000000000000, 0.000000000000000000, 0.000000000000000000 ) ) ;
#38180 = CIRCLE ( 'NONE', #6125, 120.5010000000000190 ) ;
#38181 = CARTESIAN_POINT ( 'NONE',  ( -10.00000000000000000, 0.000000000000000000, 0.000000000000000000 ) ) ;
#38182 = CARTESIAN_POINT ( 'NONE',  ( 0.000000000000000000, -52.88069566989388903, -103.2454939717374032 ) ) ;
#38183 = EDGE_LOOP ( 'NONE', ( #3041, #39287, #7860, #25372 ) ) ;
#38184 = CARTESIAN_POINT ( 'NONE',  ( 18.00000000000000355, 0.000000000000000000, 0.000000000000000000 ) ) ;
#38185 = EDGE_CURVE ( 'NONE', #19261, #6230, #19603, .T. ) ;
#38186 = DIRECTION ( 'NONE',  ( -1.000000000000000000, -0.000000000000000000, 0.000000000000000000 ) ) ;
#38187 = VERTEX_POINT ( 'NONE', #30941 ) ;
#38188 = DIRECTION ( 'NONE',  ( -1.000000000000000000, 0.000000000000000000, 0.000000000000000000 ) ) ;
#38189 = AXIS2_PLACEMENT_3D ( 'NONE', #10107, #4202, #17571 ) ;
#38190 = CARTESIAN_POINT ( 'NONE',  ( 17.99999999999999645, 27.24480646643629811, -15.80846360676556372 ) ) ;
#38191 = DIRECTION ( 'NONE',  ( -1.000000000000000000, 0.000000000000000000, 0.000000000000000000 ) ) ;
#38192 = CARTESIAN_POINT ( 'NONE',  ( -48.80550277073417931, 31.00000000000000355, -13.06547612810710035 ) ) ;
#38193 = VERTEX_POINT ( 'NONE', #40520 ) ;
#38195 = CARTESIAN_POINT ( 'NONE',  ( 0.000000000000000000, 0.000000000000000000, 0.000000000000000000 ) ) ;
#38194 = CARTESIAN_POINT ( 'NONE',  ( 17.99999999999999645, 16.86122981692056655, -27.13802899033274940 ) ) ;
#38196 = AXIS2_PLACEMENT_3D ( 'NONE', #8334, #14043, #27338 ) ;
#38197 = VERTEX_POINT ( 'NONE', #34639 ) ;
#38198 = AXIS2_PLACEMENT_3D ( 'NONE', #23375, #32732, #36209 ) ;
#38199 = DIRECTION ( 'NONE',  ( -1.000000000000000000, -0.000000000000000000, 0.000000000000000000 ) ) ;
#38200 = CARTESIAN_POINT ( 'NONE',  ( -40.54929543462775143, 40.00000000000000000, -46.21859917192507794 ) ) ;
#38201 = CIRCLE ( 'NONE', #19433, 116.0000000000000000 ) ;
#38202 = EDGE_CURVE ( 'NONE', #41125, #24437, #23991, .T. ) ;
#38203 = CARTESIAN_POINT ( 'NONE',  ( 24.55685208795062380, 40.00000000000000000, -49.59815698162134368 ) ) ;
#38204 = CIRCLE ( 'NONE', #11774, 11.00000000000023803 ) ;
#38205 = VECTOR ( 'NONE', #13398, 1000.000000000000000 ) ;
#38206 = LINE ( 'NONE', #8106, #3955 ) ;
#38207 = DIRECTION ( 'NONE',  ( 0.000000000000000000, 0.000000000000000000, 1.000000000000000000 ) ) ;
#38208 = DIRECTION ( 'NONE',  ( -1.000000000000000000, 0.000000000000000000, 0.000000000000000000 ) ) ;
#38209 = CARTESIAN_POINT ( 'NONE',  ( 20.96880926229634312, 31.00000000000000355, -12.11681000168150213 ) ) ;
#38210 = ADVANCED_FACE ( 'NONE', ( #10654 ), #31330, .T. ) ;
#38211 = ORIENTED_EDGE ( 'NONE', *, *, #28317, .F. ) ;
#38212 = CARTESIAN_POINT ( 'NONE',  ( -25.53337963587170023, 40.00000000000000000, 29.12008199578403023 ) ) ;
#38213 = ORIENTED_EDGE ( 'NONE', *, *, #11172, .F. ) ;
#38214 = DIRECTION ( 'NONE',  ( -1.000000000000000000, -0.000000000000000000, 0.000000000000000000 ) ) ;
#38215 = CARTESIAN_POINT ( 'NONE',  ( -3.455068668934486276, 2.624017327439035707, -3.316620875263955437 ) ) ;
#38216 = ORIENTED_EDGE ( 'NONE', *, *, #32676, .T. ) ;
#38217 = ADVANCED_FACE ( 'NONE', ( #40955 ), #8250, .T. ) ;
#38218 = LINE ( 'NONE', #27787, #38842 ) ;
#38219 = FACE_OUTER_BOUND ( 'NONE', #32567, .T. ) ;
#38220 = EDGE_CURVE ( 'NONE', #27792, #3514, #598, .T. ) ;
#38221 = ORIENTED_EDGE ( 'NONE', *, *, #14801, .T. ) ;
#38222 = DIRECTION ( 'NONE',  ( 0.000000000000000000, 1.000000000000000000, -1.287488025362403787E-15 ) ) ;
#38223 = ORIENTED_EDGE ( 'NONE', *, *, #20621, .T. ) ;
#38224 = ORIENTED_EDGE ( 'NONE', *, *, #12910, .T. ) ;
#38225 = CARTESIAN_POINT ( 'NONE',  ( 0.000000000000000000, 50.95304419620825342, 10.38206564895679129 ) ) ;
#38226 = CARTESIAN_POINT ( 'NONE',  ( -70.06919973877657526, 31.00000000000000711, -18.87919424805730984 ) ) ;
#38227 = VERTEX_POINT ( 'NONE', #38760 ) ;
#38228 = CARTESIAN_POINT ( 'NONE',  ( 0.000000000000000000, 8.827181066045881153, 120.1772519049559662 ) ) ;
#38229 = AXIS2_PLACEMENT_3D ( 'NONE', #33765, #16184, #23612 ) ;
#38230 = DIRECTION ( 'NONE',  ( 0.000000000000000000, 0.000000000000000000, 1.000000000000000000 ) ) ;
#38231 = ORIENTED_EDGE ( 'NONE', *, *, #36111, .T. ) ;
#38232 = CARTESIAN_POINT ( 'NONE',  ( 18.00000000000000355, 3.840921266749842022, 47.34345070675171030 ) ) ;
#38233 = VERTEX_POINT ( 'NONE', #12181 ) ;
#38234 = FACE_OUTER_BOUND ( 'NONE', #26823, .T. ) ;
#38235 = ADVANCED_FACE ( 'NONE', ( #41824 ), #8892, .F. ) ;
#38236 = CARTESIAN_POINT ( 'NONE',  ( 6.473670811831355287, 31.00000000000000355, -24.11571013580713441 ) ) ;
#38237 = ADVANCED_FACE ( 'NONE', ( #25721 ), #22020, .F. ) ;
#38239 = DIRECTION ( 'NONE',  ( -1.000000000000000000, -0.000000000000000000, -0.000000000000000000 ) ) ;
#38238 = CARTESIAN_POINT ( 'NONE',  ( 0.000000000000000000, 91.65951123222482977, 71.09524597798119316 ) ) ;
#38240 = CYLINDRICAL_SURFACE ( 'NONE', #1789, 59.00000000000000000 ) ;
#38241 = DIRECTION ( 'NONE',  ( 1.000000000000000000, 1.836909530733573776E-16, 0.000000000000000000 ) ) ;
#38242 = ORIENTED_EDGE ( 'NONE', *, *, #16705, .T. ) ;
#38243 = CARTESIAN_POINT ( 'NONE',  ( 17.99999999999999645, 0.000000000000000000, 0.000000000000000000 ) ) ;
#38244 = VERTEX_POINT ( 'NONE', #2103 ) ;
#38245 = CARTESIAN_POINT ( 'NONE',  ( 17.99999999999999645, 105.7179949885867956, -37.57629584241721687 ) ) ;
#38246 = EDGE_CURVE ( 'NONE', #40508, #69, #25500, .T. ) ;
#38247 = CARTESIAN_POINT ( 'NONE',  ( 41.30831894254264824, 31.00000000000000355, -83.80005689411834169 ) ) ;
#38248 = CARTESIAN_POINT ( 'NONE',  ( 17.99999999999999645, -111.7974656912329436, -9.465682155096647676 ) ) ;
#38249 = ORIENTED_EDGE ( 'NONE', *, *, #9105, .F. ) ;
#38250 = ADVANCED_FACE ( 'NONE', ( #28345 ), #5608, .T. ) ;
#38251 = CARTESIAN_POINT ( 'NONE',  ( 22.27703560431449148, 40.00000000000000000, 17.12883495622503816 ) ) ;
#38252 = EDGE_LOOP ( 'NONE', ( #25125, #1412, #33698, #4592 ) ) ;
#38253 = ORIENTED_EDGE ( 'NONE', *, *, #38220, .T. ) ;
#38254 = DIRECTION ( 'NONE',  ( 0.000000000000000000, 0.000000000000000000, 1.000000000000000000 ) ) ;
#38255 = DIRECTION ( 'NONE',  ( 1.000000000000000000, 0.000000000000000000, 0.000000000000000000 ) ) ;
#38256 = AXIS2_PLACEMENT_3D ( 'NONE', #6019, #8705, #4020 ) ;
#38257 = LINE ( 'NONE', #34553, #19247 ) ;
#38258 = AXIS2_PLACEMENT_3D ( 'NONE', #11959, #2092, #28547 ) ;
#38259 = CARTESIAN_POINT ( 'NONE',  ( -147.8499999999987438, -2.957510437470159335E-13, 10.00000000000004263 ) ) ;
#38260 = VECTOR ( 'NONE', #16449, 1000.000000000000000 ) ;
#38261 = EDGE_CURVE ( 'NONE', #19203, #2829, #27950, .T. ) ;
#38262 = ORIENTED_EDGE ( 'NONE', *, *, #2105, .F. ) ;
#38263 = CARTESIAN_POINT ( 'NONE',  ( 17.99999999999999645, -23.10276247328019039, -118.2656051737072431 ) ) ;
#38264 = ORIENTED_EDGE ( 'NONE', *, *, #751, .F. ) ;
#38265 = FACE_OUTER_BOUND ( 'NONE', #30330, .T. ) ;
#38266 = DIRECTION ( 'NONE',  ( 0.000000000000000000, 0.000000000000000000, 1.000000000000000000 ) ) ;
#38267 = ADVANCED_FACE ( 'NONE', ( #42460 ), #1683, .F. ) ;
#38268 = CARTESIAN_POINT ( 'NONE',  ( 17.99999999999999645, 42.87700105098753056, -107.7847984684000551 ) ) ;
#38269 = DIRECTION ( 'NONE',  ( 0.000000000000000000, 0.000000000000000000, 1.000000000000000000 ) ) ;
#38270 = VERTEX_POINT ( 'NONE', #2303 ) ;
#38271 = ORIENTED_EDGE ( 'NONE', *, *, #5736, .F. ) ;
#38272 = CARTESIAN_POINT ( 'NONE',  ( 0.000000000000000000, 0.000000000000000000, 0.000000000000000000 ) ) ;
#38273 = DIRECTION ( 'NONE',  ( -1.000000000000000000, 0.000000000000000000, 0.000000000000000000 ) ) ;
#38274 = ORIENTED_EDGE ( 'NONE', *, *, #34813, .T. ) ;
#38276 = ORIENTED_EDGE ( 'NONE', *, *, #20754, .T. ) ;
#38275 = CARTESIAN_POINT ( 'NONE',  ( 0.000000000000000000, 0.000000000000000000, 0.000000000000000000 ) ) ;
#38277 = CARTESIAN_POINT ( 'NONE',  ( -37.13421060599358725, 31.00000000000000355, -21.52932707635455500 ) ) ;
#38278 = VERTEX_POINT ( 'NONE', #15671 ) ;
#38279 = CARTESIAN_POINT ( 'NONE',  ( 0.000000000000000000, 0.000000000000000000, 0.000000000000000000 ) ) ;
#38281 = CARTESIAN_POINT ( 'NONE',  ( 17.99999999999999645, -25.52601536738605859, 19.21447964122688390 ) ) ;
#38280 = CYLINDRICAL_SURFACE ( 'NONE', #31, 120.5010000000000190 ) ;
#38282 = ORIENTED_EDGE ( 'NONE', *, *, #21796, .T. ) ;
#38283 = CYLINDRICAL_SURFACE ( 'NONE', #448, 4.500000000000000888 ) ;
#38284 = CARTESIAN_POINT ( 'NONE',  ( -30.31917247939794180, 40.00000000000000000, 52.30862930535366928 ) ) ;
#38285 = VECTOR ( 'NONE', #37687, 1000.000000000000000 ) ;
#38286 = EDGE_CURVE ( 'NONE', #16376, #28961, #36968, .T. ) ;
#38288 = EDGE_CURVE ( 'NONE', #3729, #10037, #32709, .T. ) ;
#38287 = CIRCLE ( 'NONE', #19511, 20.00000000000000711 ) ;
#38289 = CARTESIAN_POINT ( 'NONE',  ( 17.99999999999999645, -24.22031524826050841, 109.5520369638036584 ) ) ;
#38290 = EDGE_CURVE ( 'NONE', #13925, #23479, #20298, .T. ) ;
#38291 = EDGE_CURVE ( 'NONE', #36886, #7958, #39669, .T. ) ;
#38292 = DIRECTION ( 'NONE',  ( -1.000000000000000000, 0.000000000000000000, 0.000000000000000000 ) ) ;
#38293 = VERTEX_POINT ( 'NONE', #38334 ) ;
#38294 = AXIS2_PLACEMENT_3D ( 'NONE', #20331, #16632, #3020 ) ;
#38295 = CYLINDRICAL_SURFACE ( 'NONE', #22411, 59.00000000000000000 ) ;
#38296 = ORIENTED_EDGE ( 'NONE', *, *, #4427, .F. ) ;
#38297 = FACE_OUTER_BOUND ( 'NONE', #7637, .T. ) ;
#38298 = CARTESIAN_POINT ( 'NONE',  ( 17.99999999999999645, -10.40101730206288444, -120.0512800434972149 ) ) ;
#38299 = CARTESIAN_POINT ( 'NONE',  ( 62.51641183113888900, 31.00000000000000000, -16.75201923384928548 ) ) ;
#38300 = DIRECTION ( 'NONE',  ( 1.000000000000000000, 0.000000000000000000, 0.000000000000000000 ) ) ;
#38301 = ORIENTED_EDGE ( 'NONE', *, *, #27419, .T. ) ;
#38302 = DIRECTION ( 'NONE',  ( -1.000000000000000000, 0.000000000000000000, 0.000000000000000000 ) ) ;
#38303 = ORIENTED_EDGE ( 'NONE', *, *, #982, .T. ) ;
#38304 = DIRECTION ( 'NONE',  ( 0.000000000000000000, -0.8951632913550571224, -0.4457383557765488002 ) ) ;
#38305 = CARTESIAN_POINT ( 'NONE',  ( -106.4195705685748550, -106.4195705685759776, 10.00000000000000000 ) ) ;
#38306 = CARTESIAN_POINT ( 'NONE',  ( -81.66074000183850501, 31.00000000000000711, -10.87165890510346422 ) ) ;
#38307 = CARTESIAN_POINT ( 'NONE',  ( 83.84057477258951963, 39.99999999999999289, -22.33845567676512900 ) ) ;
#38308 = DIRECTION ( 'NONE',  ( 0.000000000000000000, 0.9911528310040067513, 0.1327255272837256084 ) ) ;
#38309 = ADVANCED_FACE ( 'NONE', ( #38541 ), #22447, .F. ) ;
#38310 = VERTEX_POINT ( 'NONE', #18540 ) ;
#38311 = FACE_OUTER_BOUND ( 'NONE', #10292, .T. ) ;
#38312 = EDGE_LOOP ( 'NONE', ( #729, #6965, #36716, #36065 ) ) ;
#38313 = CIRCLE ( 'NONE', #27884, 0.08402000000000062196 ) ;
#38314 = DIRECTION ( 'NONE',  ( 1.000000000000000000, 1.836909530733573776E-16, 0.000000000000000000 ) ) ;
#38315 = CIRCLE ( 'NONE', #669, 120.5010000000000190 ) ;
#38316 = CARTESIAN_POINT ( 'NONE',  ( 5.991980000000000750, 1.847259681127465666E-15, -15.08402000000000065 ) ) ;
#38317 = AXIS2_PLACEMENT_3D ( 'NONE', #11202, #14916, #4399 ) ;
#38319 = ORIENTED_EDGE ( 'NONE', *, *, #2222, .T. ) ;
#38318 = DIRECTION ( 'NONE',  ( -1.000000000000000000, -0.000000000000000000, 0.000000000000000000 ) ) ;
#38320 = DIRECTION ( 'NONE',  ( -1.000000000000000000, -0.000000000000000000, -0.000000000000000000 ) ) ;
#38321 = VERTEX_POINT ( 'NONE', #8457 ) ;
#38322 = CARTESIAN_POINT ( 'NONE',  ( 8.999999999999998224, -31.94619804602753277, -16.59639811537390131 ) ) ;
#38323 = CARTESIAN_POINT ( 'NONE',  ( 0.000000000000000000, 0.000000000000000000, 0.000000000000000000 ) ) ;
#38324 = VERTEX_POINT ( 'NONE', #21819 ) ;
#38325 = FACE_OUTER_BOUND ( 'NONE', #25993, .T. ) ;
#38326 = DIRECTION ( 'NONE',  ( 1.000000000000000000, 0.000000000000000000, 0.000000000000000000 ) ) ;
#38328 = DIRECTION ( 'NONE',  ( -1.000000000000000000, 0.000000000000000000, 0.000000000000000000 ) ) ;
#38327 = DIRECTION ( 'NONE',  ( -1.000000000000000000, -0.000000000000000000, 0.000000000000000000 ) ) ;
#38329 = EDGE_LOOP ( 'NONE', ( #4445, #24977, #39625, #28417 ) ) ;
#38330 = DIRECTION ( 'NONE',  ( 1.000000000000000000, 0.000000000000000000, 0.000000000000000000 ) ) ;
#38331 = VERTEX_POINT ( 'NONE', #31815 ) ;
#38332 = DIRECTION ( 'NONE',  ( 0.000000000000000000, 0.000000000000000000, 1.000000000000000000 ) ) ;
#38333 = CARTESIAN_POINT ( 'NONE',  ( 36.20216622922067984, 40.00000000000000000, 9.761693653842600682 ) ) ;
#38334 = CARTESIAN_POINT ( 'NONE',  ( 2.649999999999987477, 150.5000000000000284, 10.00000000000000000 ) ) ;
#38335 = EDGE_CURVE ( 'NONE', #20914, #30242, #29957, .T. ) ;
#38336 = CIRCLE ( 'NONE', #16098, 116.0000000000000000 ) ;
#38337 = EDGE_CURVE ( 'NONE', #4630, #21903, #6234, .T. ) ;
#38338 = CYLINDRICAL_SURFACE ( 'NONE', #8920, 116.0000000000000000 ) ;
#38339 = EDGE_CURVE ( 'NONE', #5363, #19975, #8359, .T. ) ;
#38340 = EDGE_CURVE ( 'NONE', #5647, #8178, #6946, .T. ) ;
#38341 = DIRECTION ( 'NONE',  ( 1.000000000000000000, 0.000000000000000000, 0.000000000000000000 ) ) ;
#38342 = VERTEX_POINT ( 'NONE', #9740 ) ;
#38343 = CARTESIAN_POINT ( 'NONE',  ( 3.455068668934414777, -2.624017327439094327, -3.316620875263732504 ) ) ;
#38344 = EDGE_CURVE ( 'NONE', #39961, #28966, #13238, .T. ) ;
#38345 = ORIENTED_EDGE ( 'NONE', *, *, #20270, .T. ) ;
#38346 = AXIS2_PLACEMENT_3D ( 'NONE', #41854, #8049, #42054 ) ;
#38347 = DIRECTION ( 'NONE',  ( 0.000000000000000000, 0.000000000000000000, 1.000000000000000000 ) ) ;
#38348 = CARTESIAN_POINT ( 'NONE',  ( 8.999999999999998224, -87.74575819880118388, -75.87280091124561920 ) ) ;
#38350 = CARTESIAN_POINT ( 'NONE',  ( 27.23661496637203427, 31.00000000000000355, 23.88131275951389654 ) ) ;
#38349 = CIRCLE ( 'NONE', #20993, 52.00000000000000000 ) ;
#38351 = ORIENTED_EDGE ( 'NONE', *, *, #25929, .F. ) ;
#38352 = DIRECTION ( 'NONE',  ( 0.000000000000000000, 0.000000000000000000, 1.000000000000000000 ) ) ;
#38353 = AXIS2_PLACEMENT_3D ( 'NONE', #4118, #13981, #10251 ) ;
#38354 = EDGE_CURVE ( 'NONE', #16239, #25141, #30045, .T. ) ;
#38355 = CONTEXT_DEPENDENT_SHAPE_REPRESENTATION ( #42049, #1215 ) ;
#38356 = CARTESIAN_POINT ( 'NONE',  ( -10.00000000000000000, 0.000000000000000000, 0.000000000000000000 ) ) ;
#38357 = CARTESIAN_POINT ( 'NONE',  ( -25.13323546007955045, 31.00000000000000355, 74.03861446737784036 ) ) ;
#38358 = VERTEX_POINT ( 'NONE', #26757 ) ;
#38359 = CARTESIAN_POINT ( 'NONE',  ( 51.84393115708665079, 31.00000000000000355, 25.66707601012906892 ) ) ;
#38360 = CARTESIAN_POINT ( 'NONE',  ( 81.15556025174309696, 39.99999999999999289, 27.54985289775053658 ) ) ;
#38361 = VERTEX_POINT ( 'NONE', #2734 ) ;
#38362 = DIRECTION ( 'NONE',  ( 0.000000000000000000, 0.000000000000000000, 1.000000000000000000 ) ) ;
#38363 = DIRECTION ( 'NONE',  ( -1.000000000000000000, 0.000000000000000000, 0.000000000000000000 ) ) ;
#38365 = ORIENTED_EDGE ( 'NONE', *, *, #11645, .F. ) ;
#38364 = DIRECTION ( 'NONE',  ( 1.000000000000000000, 0.000000000000000000, 0.000000000000000000 ) ) ;
#38366 = CARTESIAN_POINT ( 'NONE',  ( 9.000000000000001776, -110.8621702203446659, -34.14058016547651420 ) ) ;
#38367 = AXIS2_PLACEMENT_3D ( 'NONE', #6458, #32869, #26352 ) ;
#38369 = ADVANCED_FACE ( 'NONE', ( #16754 ), #36546, .F. ) ;
#38368 = CARTESIAN_POINT ( 'NONE',  ( 17.99999999999999645, -64.69195966009955612, 96.28577441832231898 ) ) ;
#38370 = ORIENTED_EDGE ( 'NONE', *, *, #34054, .F. ) ;
#38371 = CARTESIAN_POINT ( 'NONE',  ( 33.41571365387085280, 40.00000000000000000, 57.85165222247763239 ) ) ;
#38372 = CYLINDRICAL_SURFACE ( 'NONE', #22929, 2.649999999999999467 ) ;
#38373 = AXIS2_PLACEMENT_3D ( 'NONE', #37417, #37630, #13894 ) ;
#38374 = CIRCLE ( 'NONE', #30734, 31.49899999999999878 ) ;
#38375 = ORIENTED_EDGE ( 'NONE', *, *, #7944, .F. ) ;
#38376 = VECTOR ( 'NONE', #35490, 1000.000000000000000 ) ;
#38377 = DIRECTION ( 'NONE',  ( 0.000000000000000000, 0.000000000000000000, 1.000000000000000000 ) ) ;
#38378 = CARTESIAN_POINT ( 'NONE',  ( 0.000000000000000000, -13.85708833599937861, -45.43276465116677798 ) ) ;
#38379 = AXIS2_PLACEMENT_3D ( 'NONE', #20075, #43140, #30078 ) ;
#38380 = CARTESIAN_POINT ( 'NONE',  ( 0.000000000000000000, 0.7408941433508176022, -1.199999999999999956 ) ) ;
#38381 = ORIENTED_EDGE ( 'NONE', *, *, #4733, .F. ) ;
#38382 = ORIENTED_EDGE ( 'NONE', *, *, #296, .T. ) ;
#38383 = CYLINDRICAL_SURFACE ( 'NONE', #12836, 23.00000000000000000 ) ;
#38384 = ORIENTED_EDGE ( 'NONE', *, *, #12191, .F. ) ;
#38385 = CIRCLE ( 'NONE', #22423, 20.00000000000000711 ) ;
#38386 = CARTESIAN_POINT ( 'NONE',  ( 0.000000000000000000, 0.000000000000000000, 0.000000000000000000 ) ) ;
#38387 = DIRECTION ( 'NONE',  ( 0.000000000000000000, 0.000000000000000000, 1.000000000000000000 ) ) ;
#38388 = DIRECTION ( 'NONE',  ( 0.000000000000000000, 0.000000000000000000, 1.000000000000000000 ) ) ;
#38389 = EDGE_CURVE ( 'NONE', #1383, #19619, #26125, .T. ) ;
#38390 = ADVANCED_FACE ( 'NONE', ( #29608 ), #42665, .F. ) ;
#38391 = CARTESIAN_POINT ( 'NONE',  ( 0.000000000000000000, -68.63002662989681824, -93.51962064069581970 ) ) ;
#38392 = EDGE_LOOP ( 'NONE', ( #25914, #40321, #3000, #27242 ) ) ;
#38393 = DIRECTION ( 'NONE',  ( 1.000000000000000000, 0.000000000000000000, -0.000000000000000000 ) ) ;
#38394 = EDGE_CURVE ( 'NONE', #2759, #38331, #38313, .T. ) ;
#38395 = DIRECTION ( 'NONE',  ( -1.000000000000000000, 0.000000000000000000, 0.000000000000000000 ) ) ;
#38396 = ORIENTED_EDGE ( 'NONE', *, *, #29294, .F. ) ;
#38397 = CARTESIAN_POINT ( 'NONE',  ( 17.99999999999999645, 89.07460286905958924, -81.15544420874873310 ) ) ;
#38398 = AXIS2_PLACEMENT_3D ( 'NONE', #38076, #34371, #31118 ) ;
#38399 = DIRECTION ( 'NONE',  ( -1.000000000000000000, -0.000000000000000000, 0.000000000000000000 ) ) ;
#38400 = EDGE_CURVE ( 'NONE', #40375, #25565, #6669, .T. ) ;
#38401 = DIRECTION ( 'NONE',  ( -0.7071067811865512365, -6.123233995736766036E-17, -0.7071067811865437980 ) ) ;
#38402 = CARTESIAN_POINT ( 'NONE',  ( 18.00000000000000355, 0.000000000000000000, 0.000000000000000000 ) ) ;
#38403 = CARTESIAN_POINT ( 'NONE',  ( -38.92335646797288717, 31.00000000000000355, 29.86975225897632313 ) ) ;
#38404 = EDGE_LOOP ( 'NONE', ( #35576, #40529, #37266, #20626 ) ) ;
#38406 = CARTESIAN_POINT ( 'NONE',  ( 0.000000000000000000, -0.6505223195686533622, 51.99593080916758936 ) ) ;
#38405 = CARTESIAN_POINT ( 'NONE',  ( 0.000000000000000000, 0.000000000000000000, 0.000000000000000000 ) ) ;
#38407 = AXIS2_PLACEMENT_3D ( 'NONE', #17067, #30352, #428 ) ;
#38408 = EDGE_CURVE ( 'NONE', #36747, #19747, #1374, .T. ) ;
#38409 = VERTEX_POINT ( 'NONE', #39613 ) ;
#38410 = AXIS2_PLACEMENT_3D ( 'NONE', #18471, #37830, #41094 ) ;
#38411 = CARTESIAN_POINT ( 'NONE',  ( 50.09382087749727930, 40.00000000000000000, 24.69014870349942825 ) ) ;
#38412 = DIRECTION ( 'NONE',  ( -1.000000000000000000, 0.000000000000000000, -0.000000000000000000 ) ) ;
#38413 = CARTESIAN_POINT ( 'NONE',  ( 17.99999999999999645, -83.49789599728842404, 86.88263557826738293 ) ) ;
#38414 = CARTESIAN_POINT ( 'NONE',  ( 17.99999999999999645, -114.1157422997281969, -20.82300072953048442 ) ) ;
#38415 = LINE ( 'NONE', #41903, #1559 ) ;
#38416 = ORIENTED_EDGE ( 'NONE', *, *, #25060, .T. ) ;
#38417 = CARTESIAN_POINT ( 'NONE',  ( 33.47591237148697729, 40.00000000000000000, -8.973542178613062248 ) ) ;
#38418 = EDGE_LOOP ( 'NONE', ( #35024, #21336, #28637, #19502 ) ) ;
#38419 = CARTESIAN_POINT ( 'NONE',  ( 18.00000000000000355, 36.05989434073613609, 30.12041790338630776 ) ) ;
#38420 = CARTESIAN_POINT ( 'NONE',  ( -4.141042297810615835, 2.227970268150415656, -3.687027686973619822 ) ) ;
#38421 = VERTEX_POINT ( 'NONE', #42880 ) ;
#38422 = DIRECTION ( 'NONE',  ( -1.000000000000000000, -0.000000000000000000, -0.000000000000000000 ) ) ;
#38423 = DIRECTION ( 'NONE',  ( -1.000000000000000000, -0.000000000000000000, -0.000000000000000000 ) ) ;
#38424 = ORIENTED_EDGE ( 'NONE', *, *, #28926, .F. ) ;
#38425 = CARTESIAN_POINT ( 'NONE',  ( 17.99999999999999645, -114.6488492393077081, -37.09625815500128709 ) ) ;
#38426 = ORIENTED_EDGE ( 'NONE', *, *, #33708, .F. ) ;
#38427 = AXIS2_PLACEMENT_3D ( 'NONE', #8556, #24757, #2003 ) ;
#38428 = ORIENTED_EDGE ( 'NONE', *, *, #4138, .F. ) ;
#38429 = CARTESIAN_POINT ( 'NONE',  ( 17.99999999999999645, 6.486220790509957368, -112.0098273076986715 ) ) ;
#38430 = AXIS2_PLACEMENT_3D ( 'NONE', #39611, #23087, #32225 ) ;
#38431 = CARTESIAN_POINT ( 'NONE',  ( -81.66074000183850501, 31.00000000000000711, -10.87165890510346422 ) ) ;
#38432 = EDGE_LOOP ( 'NONE', ( #7600, #13191, #3208, #29698 ) ) ;
#38433 = CARTESIAN_POINT ( 'NONE',  ( 17.99999999999999645, 29.03409033315581667, 12.21509719675401051 ) ) ;
#38434 = EDGE_CURVE ( 'NONE', #29115, #35353, #32863, .T. ) ;
#38435 = DIRECTION ( 'NONE',  ( -0.000000000000000000, -0.000000000000000000, 1.000000000000000000 ) ) ;
#38436 = ORIENTED_EDGE ( 'NONE', *, *, #9501, .T. ) ;
#38437 = DIRECTION ( 'NONE',  ( 1.000000000000000000, -1.373900992973641868E-15, -3.273063162220443081E-16 ) ) ;
#38438 = CARTESIAN_POINT ( 'NONE',  ( -61.42214656771047743, 40.00000000000000711, 79.86467493626639680 ) ) ;
#38439 = AXIS2_PLACEMENT_3D ( 'NONE', #36939, #33664, #11217 ) ;
#38440 = CARTESIAN_POINT ( 'NONE',  ( -11.85532105537472525, 31.00000000000000355, -20.54123584193516550 ) ) ;
#38442 = CARTESIAN_POINT ( 'NONE',  ( -22.00000000000000000, 17.11489954122026447, 0.000000000000000000 ) ) ;
#38441 = FACE_OUTER_BOUND ( 'NONE', #8726, .T. ) ;
#38443 = LINE ( 'NONE', #24764, #18606 ) ;
#38444 = DIRECTION ( 'NONE',  ( 0.000000000000000000, -0.2113826236296315053, 0.9774033898178651203 ) ) ;
#38445 = ORIENTED_EDGE ( 'NONE', *, *, #32335, .T. ) ;
#38446 = EDGE_CURVE ( 'NONE', #38310, #29868, #18846, .T. ) ;
#38447 = DIRECTION ( 'NONE',  ( -1.000000000000000000, -0.000000000000000000, -0.000000000000000000 ) ) ;
#38448 = ORIENTED_EDGE ( 'NONE', *, *, #6842, .F. ) ;
#38449 = CARTESIAN_POINT ( 'NONE',  ( 17.99999999999999645, 0.000000000000000000, 0.000000000000000000 ) ) ;
#38450 = EDGE_CURVE ( 'NONE', #19972, #40017, #11151, .T. ) ;
#38451 = CARTESIAN_POINT ( 'NONE',  ( -86.05617919112455638, 31.00000000000000711, 49.70311056393224192 ) ) ;
#38452 = CYLINDRICAL_SURFACE ( 'NONE', #12814, 59.00000000000000000 ) ;
#38453 = ORIENTED_EDGE ( 'NONE', *, *, #21561, .T. ) ;
#38454 = CARTESIAN_POINT ( 'NONE',  ( 4.597210615070504325, 40.00000000000000000, -34.47704375835832025 ) ) ;
#38455 = AXIS2_PLACEMENT_3D ( 'NONE', #40743, #14173, #36615 ) ;
#38456 = AXIS2_PLACEMENT_3D ( 'NONE', #35392, #39501, #35588 ) ;
#38457 = ORIENTED_EDGE ( 'NONE', *, *, #26397, .T. ) ;
#38458 = ORIENTED_EDGE ( 'NONE', *, *, #38096, .F. ) ;
#38459 = CARTESIAN_POINT ( 'NONE',  ( 1.598609366639573350E-14, -1.063425437509180407E-13, -40.00000000000000000 ) ) ;
#38460 = DIRECTION ( 'NONE',  ( 0.000000000000000000, 0.000000000000000000, 1.000000000000000000 ) ) ;
#38461 = CARTESIAN_POINT ( 'NONE',  ( -142.5000000000000284, 1.745121688784978386E-14, -25.00000000000000000 ) ) ;
#38462 = AXIS2_PLACEMENT_3D ( 'NONE', #31426, #25546, #21644 ) ;
#38463 = DIRECTION ( 'NONE',  ( 0.000000000000000000, 0.000000000000000000, 1.000000000000000000 ) ) ;
#38464 = ADVANCED_FACE ( 'NONE', ( #13042 ), #26343, .F. ) ;
#38465 = CARTESIAN_POINT ( 'NONE',  ( 0.000000000000000000, 0.000000000000000000, 0.000000000000000000 ) ) ;
#38466 = ORIENTED_EDGE ( 'NONE', *, *, #15006, .T. ) ;
#38467 = CYLINDRICAL_SURFACE ( 'NONE', #27744, 2.649999999999999467 ) ;
#38468 = ORIENTED_EDGE ( 'NONE', *, *, #25911, .T. ) ;
#38469 = CARTESIAN_POINT ( 'NONE',  ( 17.99999999999999645, 0.000000000000000000, 0.000000000000000000 ) ) ;
#38470 = EDGE_CURVE ( 'NONE', #20449, #20287, #9043, .T. ) ;
#38471 = DIRECTION ( 'NONE',  ( 0.000000000000000000, 0.000000000000000000, 1.000000000000000000 ) ) ;
#38472 = ADVANCED_FACE ( 'NONE', ( #6037 ), #19388, .F. ) ;
#38473 = DIRECTION ( 'NONE',  ( 0.000000000000000000, -0.7865515558026479059, 0.6175246149461850464 ) ) ;
#38474 = FACE_OUTER_BOUND ( 'NONE', #41008, .T. ) ;
#38475 = ORIENTED_EDGE ( 'NONE', *, *, #29165, .T. ) ;
#38476 = VERTEX_POINT ( 'NONE', #19304 ) ;
#38477 = LINE ( 'NONE', #21544, #13790 ) ;
#38478 = ADVANCED_BREP_SHAPE_REPRESENTATION ( '', ( #13741, #13552 ), #32277 ) ;
#38479 = ORIENTED_EDGE ( 'NONE', *, *, #34813, .F. ) ;
#38481 = ORIENTED_EDGE ( 'NONE', *, *, #38162, .T. ) ;
#38480 = FACE_OUTER_BOUND ( 'NONE', #32305, .T. ) ;
#38482 = CARTESIAN_POINT ( 'NONE',  ( 54.55067978551168295, 31.00000000000000355, 18.62288743479739139 ) ) ;
#38483 = ORIENTED_EDGE ( 'NONE', *, *, #30198, .T. ) ;
#38484 = DIRECTION ( 'NONE',  ( -1.000000000000000000, -0.000000000000000000, -0.000000000000000000 ) ) ;
#38485 = EDGE_CURVE ( 'NONE', #12223, #17739, #2231, .T. ) ;
#38487 = DIRECTION ( 'NONE',  ( 0.000000000000000000, 0.000000000000000000, 1.000000000000000000 ) ) ;
#38486 = CARTESIAN_POINT ( 'NONE',  ( 0.000000000000000000, 0.000000000000000000, -5.000000000000000000 ) ) ;
#38488 = ORIENTED_EDGE ( 'NONE', *, *, #27740, .F. ) ;
#38489 = AXIS2_PLACEMENT_3D ( 'NONE', #38769, #12189, #32871 ) ;
#38490 = CARTESIAN_POINT ( 'NONE',  ( 17.81064159970942384, 40.00000000000000000, 66.89829513328324140 ) ) ;
#38491 = DIRECTION ( 'NONE',  ( -0.000000000000000000, -0.000000000000000000, 1.000000000000000000 ) ) ;
#38492 = VECTOR ( 'NONE', #5166, 1000.000000000000000 ) ;
#38493 = DIRECTION ( 'NONE',  ( 1.000000000000000000, 0.000000000000000000, 0.000000000000000000 ) ) ;
#38494 = ORIENTED_EDGE ( 'NONE', *, *, #40934, .F. ) ;
#38495 = DIRECTION ( 'NONE',  ( 0.000000000000000000, 0.000000000000000000, 1.000000000000000000 ) ) ;
#38496 = VERTEX_POINT ( 'NONE', #11890 ) ;
#38497 = ADVANCED_FACE ( 'NONE', ( #42383 ), #35419, .F. ) ;
#38498 =( NAMED_UNIT ( * ) SI_UNIT ( $, .STERADIAN. ) SOLID_ANGLE_UNIT ( ) );
#38499 = CIRCLE ( 'NONE', #41985, 59.00000000000001421 ) ;
#38500 = CARTESIAN_POINT ( 'NONE',  ( 0.000000000000000000, 27.24480646643607074, 15.80846360676594564 ) ) ;
#38501 = CARTESIAN_POINT ( 'NONE',  ( -25.39999999999999147, 0.000000000000000000, 0.000000000000000000 ) ) ;
#38502 = EDGE_CURVE ( 'NONE', #11159, #38585, #12552, .T. ) ;
#38503 = CARTESIAN_POINT ( 'NONE',  ( -51.86900026051868196, 31.00000000000000355, 45.50549606403863123 ) ) ;
#38504 = DIRECTION ( 'NONE',  ( -1.000000000000000000, -0.000000000000000000, -0.000000000000000000 ) ) ;
#38505 = ORIENTED_EDGE ( 'NONE', *, *, #40981, .T. ) ;
#38506 = EDGE_CURVE ( 'NONE', #26923, #42412, #28892, .T. ) ;
#38507 = DIRECTION ( 'NONE',  ( -1.000000000000000000, -0.000000000000000000, 0.000000000000000000 ) ) ;
#38508 = ORIENTED_EDGE ( 'NONE', *, *, #39009, .F. ) ;
#38509 = DIRECTION ( 'NONE',  ( 0.000000000000000000, 0.000000000000000000, 1.000000000000000000 ) ) ;
#38510 = DIRECTION ( 'NONE',  ( -1.000000000000000000, -0.000000000000000000, 0.000000000000000000 ) ) ;
#38511 = CARTESIAN_POINT ( 'NONE',  ( 53.86549405311983918, 31.00000000000000355, 70.40131829849023859 ) ) ;
#38512 = CARTESIAN_POINT ( 'NONE',  ( 58.29702017945731995, 39.99999999999999289, 66.63806913872475945 ) ) ;
#38513 = DIRECTION ( 'NONE',  ( 0.000000000000000000, 0.8477344278896721264, -0.5304209081197405196 ) ) ;
#38514 = AXIS2_PLACEMENT_3D ( 'NONE', #35026, #17842, #21340 ) ;
#38515 = ORIENTED_EDGE ( 'NONE', *, *, #18062, .F. ) ;
#38516 = DIRECTION ( 'NONE',  ( -1.000000000000000000, -0.000000000000000000, -0.000000000000000000 ) ) ;
#38517 = ORIENTED_EDGE ( 'NONE', *, *, #569, .F. ) ;
#38518 = LINE ( 'NONE', #11507, #17235 ) ;
#38519 = CARTESIAN_POINT ( 'NONE',  ( 0.000000000000000000, -11.58753559615464290, -29.77419532459275331 ) ) ;
#38520 = EDGE_CURVE ( 'NONE', #19286, #32742, #18164, .T. ) ;
#38521 = EDGE_CURVE ( 'NONE', #27109, #23893, #28574, .T. ) ;
#38523 = ORIENTED_EDGE ( 'NONE', *, *, #25433, .T. ) ;
#38522 = DIRECTION ( 'NONE',  ( -1.000000000000000000, -0.000000000000000000, -0.000000000000000000 ) ) ;
#38524 = DIRECTION ( 'NONE',  ( 0.000000000000000000, 0.000000000000000000, 1.000000000000000000 ) ) ;
#38525 = ORIENTED_EDGE ( 'NONE', *, *, #27133, .F. ) ;
#38526 = DIRECTION ( 'NONE',  ( -1.000000000000000000, 0.000000000000000000, 0.000000000000000000 ) ) ;
#38527 = DIRECTION ( 'NONE',  ( 0.000000000000000000, 0.1253332335643046469, -0.9921147013144777649 ) ) ;
#38528 = CARTESIAN_POINT ( 'NONE',  ( 0.000000000000000000, 0.000000000000000000, -5.000000000000000000 ) ) ;
#38529 = VECTOR ( 'NONE', #27208, 1000.000000000000000 ) ;
#38530 = ORIENTED_EDGE ( 'NONE', *, *, #28210, .T. ) ;
#38531 = CARTESIAN_POINT ( 'NONE',  ( 53.80287614962789178, -40.05525454449572464, 69.29271901957253021 ) ) ;
#38532 = CARTESIAN_POINT ( 'NONE',  ( 0.000000000000000000, -104.6166166098448826, 50.11350645393640235 ) ) ;
#38533 = ADVANCED_FACE ( 'NONE', ( #12101 ), #8806, .F. ) ;
#38535 = CARTESIAN_POINT ( 'NONE',  ( 0.000000000000000000, 49.65209126885762458, 15.44894276735567651 ) ) ;
#38534 = CYLINDRICAL_SURFACE ( 'NONE', #35559, 13.60000000000000142 ) ;
#38536 = ORIENTED_EDGE ( 'NONE', *, *, #30325, .T. ) ;
#38537 = DIRECTION ( 'NONE',  ( -1.000000000000000000, -0.000000000000000000, -0.000000000000000000 ) ) ;
#38538 = EDGE_LOOP ( 'NONE', ( #7848, #34011, #6117, #2548 ) ) ;
#38539 = DIRECTION ( 'NONE',  ( 0.000000000000000000, -0.7164567402983067490, -0.6976315211349933820 ) ) ;
#38540 = CARTESIAN_POINT ( 'NONE',  ( 2.996940313443920978, 40.00000000000000000, -44.59688583547568896 ) ) ;
#38541 = FACE_OUTER_BOUND ( 'NONE', #33482, .T. ) ;
#38542 = CARTESIAN_POINT ( 'NONE',  ( 17.99999999999999645, 0.000000000000000000, 0.000000000000000000 ) ) ;
#38543 = AXIS2_PLACEMENT_3D ( 'NONE', #40373, #3929, #7442 ) ;
#38544 = FACE_OUTER_BOUND ( 'NONE', #26818, .T. ) ;
#38545 = ORIENTED_EDGE ( 'NONE', *, *, #34213, .F. ) ;
#38546 = LINE ( 'NONE', #28565, #41524 ) ;
#38547 = ORIENTED_EDGE ( 'NONE', *, *, #18056, .T. ) ;
#38548 = ADVANCED_FACE ( 'NONE', ( #18460 ), #12735, .F. ) ;
#38549 = CIRCLE ( 'NONE', #19779, 47.49900000000000944 ) ;
#38550 = CARTESIAN_POINT ( 'NONE',  ( 0.000000000000000000, 109.4038418350903470, 50.51029986767587587 ) ) ;
#38551 = DIRECTION ( 'NONE',  ( -1.000000000000000000, 0.000000000000000000, 0.000000000000000000 ) ) ;
#38552 = EDGE_CURVE ( 'NONE', #23356, #10153, #25218, .T. ) ;
#38553 = CARTESIAN_POINT ( 'NONE',  ( -2.781618486875174767, 31.00000000000000355, -42.39583333490362804 ) ) ;
#38554 = EDGE_LOOP ( 'NONE', ( #9829, #23731, #29987, #15617 ) ) ;
#38555 = CARTESIAN_POINT ( 'NONE',  ( 17.99999999999999645, 27.83061035786954918, 117.2431154827798281 ) ) ;
#38556 = CARTESIAN_POINT ( 'NONE',  ( 0.000000000000000000, 54.09091620264722877, 102.6166301549519488 ) ) ;
#38557 = CARTESIAN_POINT ( 'NONE',  ( 26.74431375183570481, 31.00000000000000355, -78.78324499025107741 ) ) ;
#38558 = CIRCLE ( 'NONE', #2293, 120.5010000000000474 ) ;
#38559 = EDGE_LOOP ( 'NONE', ( #8898, #24389, #37814, #3482 ) ) ;
#38560 = CARTESIAN_POINT ( 'NONE',  ( 56.43498182460272972, 31.00000000000000355, -7.339809665447901921 ) ) ;
#38561 = CARTESIAN_POINT ( 'NONE',  ( -23.88228986782336349, 40.00000000000000000, -89.13686966975919290 ) ) ;
#38562 = AXIS2_PLACEMENT_3D ( 'NONE', #20603, #33876, #20838 ) ;
#38563 = ORIENTED_EDGE ( 'NONE', *, *, #15425, .T. ) ;
#38564 = CARTESIAN_POINT ( 'NONE',  ( 0.000000000000000000, 0.000000000000000000, -20.00000000000000000 ) ) ;
#38565 = ADVANCED_FACE ( 'NONE', ( #41956 ), #32357, .F. ) ;
#38566 = CARTESIAN_POINT ( 'NONE',  ( 0.000000000000000000, 30.78424799127077094, -6.672111855472859787 ) ) ;
#38567 = AXIS2_PLACEMENT_3D ( 'NONE', #32767, #41940, #35183 ) ;
#38568 = DIRECTION ( 'NONE',  ( 0.000000000000000000, 0.000000000000000000, 1.000000000000000000 ) ) ;
#38569 = EDGE_CURVE ( 'NONE', #10316, #37810, #2750, .T. ) ;
#38570 = EDGE_CURVE ( 'NONE', #26693, #5822, #10451, .T. ) ;
#38571 = EDGE_CURVE ( 'NONE', #38997, #40885, #32733, .T. ) ;
#38572 = CIRCLE ( 'NONE', #941, 116.0000000000000000 ) ;
#38574 = ORIENTED_EDGE ( 'NONE', *, *, #19048, .T. ) ;
#38573 = FACE_OUTER_BOUND ( 'NONE', #6432, .T. ) ;
#38575 = CYLINDRICAL_SURFACE ( 'NONE', #15631, 20.00000000000000711 ) ;
#38576 = DIRECTION ( 'NONE',  ( -1.000000000000000000, 0.000000000000000000, -0.000000000000000000 ) ) ;
#38577 = VECTOR ( 'NONE', #28586, 1000.000000000000000 ) ;
#38578 = VERTEX_POINT ( 'NONE', #15181 ) ;
#38579 = CARTESIAN_POINT ( 'NONE',  ( -4.417864660710832503, 40.00000000000000000, 67.60416666563759236 ) ) ;
#38580 = DIRECTION ( 'NONE',  ( 0.000000000000000000, 0.3681245526846720906, 0.9297764858882537897 ) ) ;
#38581 = VERTEX_POINT ( 'NONE', #29112 ) ;
#38582 = CARTESIAN_POINT ( 'NONE',  ( 0.000000000000000000, -2.007101075699733173, -31.43498920425971832 ) ) ;
#38583 = CARTESIAN_POINT ( 'NONE',  ( 17.99999999999999645, 23.85344185397347161, -113.5209818126988779 ) ) ;
#38584 = DIRECTION ( 'NONE',  ( -1.000000000000000000, -0.000000000000000000, 0.000000000000000000 ) ) ;
#38585 = VERTEX_POINT ( 'NONE', #28486 ) ;
#38586 = AXIS2_PLACEMENT_3D ( 'NONE', #28824, #8954, #38401 ) ;
#38587 = ORIENTED_EDGE ( 'NONE', *, *, #9227, .F. ) ;
#38588 = CARTESIAN_POINT ( 'NONE',  ( 17.99999999999999645, -29.86146781000025285, 112.0905559814577970 ) ) ;
#38589 = AXIS2_PLACEMENT_3D ( 'NONE', #29152, #38300, #42419 ) ;
#38590 = ORIENTED_EDGE ( 'NONE', *, *, #27178, .F. ) ;
#38591 = DIRECTION ( 'NONE',  ( 0.000000000000000000, 0.000000000000000000, 1.000000000000000000 ) ) ;
#38592 = DIRECTION ( 'NONE',  ( 0.000000000000000000, 0.000000000000000000, -1.000000000000000000 ) ) ;
#38593 = CARTESIAN_POINT ( 'NONE',  ( 17.99999999999999645, -30.71634675606047793, -8.790889055186887902 ) ) ;
#38594 = CLOSED_SHELL ( 'NONE', ( #6720, #21558, #6910, #41995, #15191, #20158, #20135, #30830, #2189, #36733, #5493, #15229, #16060, #31310, #11614, #40253, #15207, #24922, #40350, #28484, #5468, #14387, #29355, #42261, #31226, #17851, #15134, #30250, #8307, #20213, #9670, #39711, #11737, #22598, #41230, #28113, #30792, #28480, #21187, #161 ) ) ;
#38595 = DIRECTION ( 'NONE',  ( -1.000000000000000000, -0.000000000000000000, -0.000000000000000000 ) ) ;
#38597 = ORIENTED_EDGE ( 'NONE', *, *, #27984, .T. ) ;
#38596 = CIRCLE ( 'NONE', #263, 120.5010000000000190 ) ;
#38598 = CARTESIAN_POINT ( 'NONE',  ( 0.000000000000000000, 46.12538073176347808, 111.3235835452212825 ) ) ;
#38599 = UNCERTAINTY_MEASURE_WITH_UNIT (LENGTH_MEASURE( 1.000000000000000082E-05 ), #18440, 'distance_accuracy_value', 'NONE');
#38600 = ORIENTED_EDGE ( 'NONE', *, *, #39579, .F. ) ;
#38601 = AXIS2_PLACEMENT_3D ( 'NONE', #5786, #18945, #32201 ) ;
#38602 = CARTESIAN_POINT ( 'NONE',  ( 17.99999999999999645, 0.000000000000000000, 0.000000000000000000 ) ) ;
#38603 = ORIENTED_EDGE ( 'NONE', *, *, #21166, .T. ) ;
#38604 = DIRECTION ( 'NONE',  ( -1.000000000000000000, 0.000000000000000000, -0.000000000000000000 ) ) ;
#38605 = CIRCLE ( 'NONE', #6552, 13.59999999999999964 ) ;
#38606 = EDGE_CURVE ( 'NONE', #17796, #10741, #25135, .T. ) ;
#38607 = DIRECTION ( 'NONE',  ( 0.000000000000000000, -0.9911528310040057521, -0.1327255272837324362 ) ) ;
#38608 = SHAPE_DEFINITION_REPRESENTATION ( #16550, #18009 ) ;
#38609 = CARTESIAN_POINT ( 'NONE',  ( 0.2500000000000002220, 0.000000000000000000, 4.000000000000000000 ) ) ;
#38610 = CARTESIAN_POINT ( 'NONE',  ( 43.19851606872948935, 31.00000000000000355, 14.66122656362567689 ) ) ;
#38611 = ORIENTED_EDGE ( 'NONE', *, *, #26679, .T. ) ;
#38612 = CARTESIAN_POINT ( 'NONE',  ( 0.000000000000000000, -28.57802095670076881, -14.28532136906702732 ) ) ;
#38613 = ORIENTED_EDGE ( 'NONE', *, *, #6607, .F. ) ;
#38614 = CARTESIAN_POINT ( 'NONE',  ( 16.30650823456882748, 40.00000000000000000, -60.90571087954511142 ) ) ;
#38615 = ORIENTED_EDGE ( 'NONE', *, *, #42992, .F. ) ;
#38616 = VECTOR ( 'NONE', #40584, 1000.000000000000000 ) ;
#38617 = AXIS2_PLACEMENT_3D ( 'NONE', #38194, #14887, #27763 ) ;
#38618 = CARTESIAN_POINT ( 'NONE',  ( -107.9608013043457930, -12.05525454449572109, 14.45886780445738395 ) ) ;
#38619 = LINE ( 'NONE', #38413, #27011 ) ;
#38620 = EDGE_CURVE ( 'NONE', #35353, #5127, #35508, .T. ) ;
#38621 = EDGE_CURVE ( 'NONE', #36853, #19393, #41069, .T. ) ;
#38622 = DIRECTION ( 'NONE',  ( 0.000000000000000000, -0.1062934856473523731, -0.9943348002101385363 ) ) ;
#38623 = VECTOR ( 'NONE', #4965, 1000.000000000000000 ) ;
#38624 = DIRECTION ( 'NONE',  ( 0.000000000000000000, 0.000000000000000000, 1.000000000000000000 ) ) ;
#38625 = EDGE_CURVE ( 'NONE', #32708, #29708, #28686, .T. ) ;
#38626 = CIRCLE ( 'NONE', #17789, 13.59999999999999964 ) ;
#38627 = ORIENTED_EDGE ( 'NONE', *, *, #31388, .T. ) ;
#38628 = CARTESIAN_POINT ( 'NONE',  ( 29.64712525329720449, 40.00000000000000000, -17.12831674356021239 ) ) ;
#38629 = ORIENTED_EDGE ( 'NONE', *, *, #40006, .T. ) ;
#38630 = CYLINDRICAL_SURFACE ( 'NONE', #29912, 36.00000000000000000 ) ;
#38631 = DIRECTION ( 'NONE',  ( 0.000000000000000000, 0.000000000000000000, 1.000000000000000000 ) ) ;
#38632 = CIRCLE ( 'NONE', #25478, 59.00000000000000000 ) ;
#38633 = VERTEX_POINT ( 'NONE', #39948 ) ;
#38634 = AXIS2_PLACEMENT_3D ( 'NONE', #10286, #36665, #33195 ) ;
#38635 = CARTESIAN_POINT ( 'NONE',  ( 142.4999999999992895, -3.154162532185255727E-13, -45.00000000000004974 ) ) ;
#38636 = VECTOR ( 'NONE', #14999, 1000.000000000000000 ) ;
#38637 = ORIENTED_EDGE ( 'NONE', *, *, #23110, .T. ) ;
#38638 = LINE ( 'NONE', #8761, #6773 ) ;
#38639 = ORIENTED_EDGE ( 'NONE', *, *, #23914, .T. ) ;
#38640 = VECTOR ( 'NONE', #40883, 1000.000000000000000 ) ;
#38641 = ORIENTED_EDGE ( 'NONE', *, *, #5906, .F. ) ;
#38642 = CARTESIAN_POINT ( 'NONE',  ( 0.000000000000000000, 47.00885577955421013, -6.806061952191806874 ) ) ;
#38643 = EDGE_CURVE ( 'NONE', #4169, #9213, #20958, .T. ) ;
#38644 = CARTESIAN_POINT ( 'NONE',  ( 86.24314314301659579, 31.00000000000000000, -11.24622374123920920 ) ) ;
#38645 = ORIENTED_EDGE ( 'NONE', *, *, #17042, .F. ) ;
#38646 = DIRECTION ( 'NONE',  ( 0.000000000000000000, 0.4132121857683790922, -0.9106347728549127885 ) ) ;
#38647 = CARTESIAN_POINT ( 'NONE',  ( 17.99999999999999645, 0.000000000000000000, 0.000000000000000000 ) ) ;
#38648 = ORIENTED_EDGE ( 'NONE', *, *, #1113, .T. ) ;
#38650 = CIRCLE ( 'NONE', #19180, 59.00000000000000000 ) ;
#38649 = CARTESIAN_POINT ( 'NONE',  ( 17.99999999999999645, 11.65176648921190150, -115.4133282497341355 ) ) ;
#38651 = CARTESIAN_POINT ( 'NONE',  ( 31.77777543000702565, 40.00000000000000000, 93.95825142774114624 ) ) ;
#38652 = CARTESIAN_POINT ( 'NONE',  ( -1.974796425974089331, 31.00000000000000355, 29.60085432090884439 ) ) ;
#38654 = DIRECTION ( 'NONE',  ( 3.009274222672345096E-17, 1.000000000000000000, -2.455023325076454960E-18 ) ) ;
#38653 = CARTESIAN_POINT ( 'NONE',  ( 8.999999999999998224, 14.91999999999999993, 0.000000000000000000 ) ) ;
#38655 = AXIS2_PLACEMENT_3D ( 'NONE', #26437, #29285, #32749 ) ;
#38656 = CARTESIAN_POINT ( 'NONE',  ( -19.99999999999999645, 31.00000000000000355, 1.283214542831032867 ) ) ;
#38657 = EDGE_CURVE ( 'NONE', #23539, #33268, #11135, .T. ) ;
#38658 = CYLINDRICAL_SURFACE ( 'NONE', #22187, 116.0000000000000000 ) ;
#38659 = CIRCLE ( 'NONE', #15716, 13.59999999999999964 ) ;
#38660 = ORIENTED_EDGE ( 'NONE', *, *, #3974, .T. ) ;
#38661 = CARTESIAN_POINT ( 'NONE',  ( 0.000000000000000000, -42.60732521687558005, -19.80331771201703006 ) ) ;
#38662 = ORIENTED_EDGE ( 'NONE', *, *, #19639, .F. ) ;
#38663 = VECTOR ( 'NONE', #38157, 1000.000000000000000 ) ;
#38664 = DIRECTION ( 'NONE',  ( 0.000000000000000000, 0.000000000000000000, 1.000000000000000000 ) ) ;
#38665 = CARTESIAN_POINT ( 'NONE',  ( 42.89041025189590783, 31.00000000000000355, 86.97820559439793442 ) ) ;
#38666 = AXIS2_PLACEMENT_3D ( 'NONE', #42253, #12407, #5617 ) ;
#38667 = DIRECTION ( 'NONE',  ( 0.000000000000000000, 0.000000000000000000, -1.000000000000000000 ) ) ;
#38668 = ORIENTED_EDGE ( 'NONE', *, *, #15076, .F. ) ;
#38669 = AXIS2_PLACEMENT_3D ( 'NONE', #7277, #3120, #40220 ) ;
#38670 = CARTESIAN_POINT ( 'NONE',  ( -27.97094176822542977, 40.00000000000000000, 9.504947828999611659 ) ) ;
#38671 = CARTESIAN_POINT ( 'NONE',  ( 15.66220904948252546, 40.00000000000000000, -31.63873590539992975 ) ) ;
#38672 = AXIS2_PLACEMENT_3D ( 'NONE', #20179, #40181, #13184 ) ;
#38673 = VERTEX_POINT ( 'NONE', #4331 ) ;
#38674 = ORIENTED_EDGE ( 'NONE', *, *, #13459, .F. ) ;
#38675 = CARTESIAN_POINT ( 'NONE',  ( 139.5000000000000000, -2.144538195783117691E-13, 10.00000000000005684 ) ) ;
#38676 = FACE_OUTER_BOUND ( 'NONE', #4104, .T. ) ;
#38677 = EDGE_CURVE ( 'NONE', #14692, #2034, #839, .T. ) ;
#38678 = FACE_OUTER_BOUND ( 'NONE', #16231, .T. ) ;
#38679 = DIRECTION ( 'NONE',  ( 0.000000000000000000, 0.000000000000000000, 1.000000000000000000 ) ) ;
#38680 = ORIENTED_EDGE ( 'NONE', *, *, #3696, .T. ) ;
#38681 = DIRECTION ( 'NONE',  ( -1.000000000000000000, -0.000000000000000000, 0.000000000000000000 ) ) ;
#38682 = ORIENTED_EDGE ( 'NONE', *, *, #9326, .F. ) ;
#38683 = LINE ( 'NONE', #28690, #13154 ) ;
#38684 = AXIS2_PLACEMENT_3D ( 'NONE', #877, #39933, #17525 ) ;
#38685 = DIRECTION ( 'NONE',  ( 0.000000000000000000, 0.000000000000000000, -1.000000000000000000 ) ) ;
#38686 = AXIS2_PLACEMENT_3D ( 'NONE', #8405, #38710, #8202 ) ;
#38687 = EDGE_CURVE ( 'NONE', #24756, #6694, #40690, .T. ) ;
#38688 = LINE ( 'NONE', #2039, #16595 ) ;
#38689 = DIRECTION ( 'NONE',  ( -1.000000000000000000, -0.000000000000000000, -0.000000000000000000 ) ) ;
#38690 = VERTEX_POINT ( 'NONE', #27490 ) ;
#38691 = ORIENTED_EDGE ( 'NONE', *, *, #8418, .T. ) ;
#38692 = AXIS2_PLACEMENT_3D ( 'NONE', #12918, #27093, #23190 ) ;
#38693 = LINE ( 'NONE', #22176, #6097 ) ;
#38694 = EDGE_CURVE ( 'NONE', #36535, #844, #18874, .T. ) ;
#38695 = AXIS2_PLACEMENT_3D ( 'NONE', #40379, #34280, #31015 ) ;
#38696 = ORIENTED_EDGE ( 'NONE', *, *, #25007, .F. ) ;
#38697 = AXIS2_PLACEMENT_3D ( 'NONE', #38519, #31793, #8641 ) ;
#38699 = VERTEX_POINT ( 'NONE', #7406 ) ;
#38698 = CARTESIAN_POINT ( 'NONE',  ( -8.749793197483594298, -2.055254544495723756, 2.972870684497274762 ) ) ;
#38700 = EDGE_CURVE ( 'NONE', #22923, #6899, #14677, .T. ) ;
#38701 = CARTESIAN_POINT ( 'NONE',  ( 35.58199112953183629, 31.00000000000000355, 46.53705319858424616 ) ) ;
#38702 = CIRCLE ( 'NONE', #25515, 2.649999999999957723 ) ;
#38703 = ORIENTED_EDGE ( 'NONE', *, *, #14566, .T. ) ;
#38704 = CARTESIAN_POINT ( 'NONE',  ( 0.000000000000000000, 57.69704296431325474, -105.7900857083224082 ) ) ;
#38705 = DIRECTION ( 'NONE',  ( 0.000000000000000000, 1.505387152034110654E-14, -1.000000000000000000 ) ) ;
#38706 = AXIS2_PLACEMENT_3D ( 'NONE', #32694, #25175, #2771 ) ;
#38707 = EDGE_LOOP ( 'NONE', ( #17390, #19942, #14852, #7581 ) ) ;
#38708 = CARTESIAN_POINT ( 'NONE',  ( -71.90006454724937157, 40.00000000000000711, 4.599370544632132685 ) ) ;
#38709 = CARTESIAN_POINT ( 'NONE',  ( 7.000000000000002665, 19.59999999999999787, 0.000000000000000000 ) ) ;
#38710 = DIRECTION ( 'NONE',  ( -1.000000000000000000, -0.000000000000000000, -0.000000000000000000 ) ) ;
#38711 = VERTEX_POINT ( 'NONE', #26259 ) ;
#38712 = CARTESIAN_POINT ( 'NONE',  ( 0.000000000000000000, -57.69704296431255131, 105.7900857083227635 ) ) ;
#38713 = VERTEX_POINT ( 'NONE', #13174 ) ;
#38714 =( LENGTH_UNIT ( ) NAMED_UNIT ( * ) SI_UNIT ( .MILLI., .METRE. ) );
#38715 = EDGE_CURVE ( 'NONE', #35323, #14426, #42501, .T. ) ;
#38716 = CARTESIAN_POINT ( 'NONE',  ( 17.99999999999999645, 0.000000000000000000, 0.000000000000000000 ) ) ;
#38717 = FACE_OUTER_BOUND ( 'NONE', #15950, .T. ) ;
#38718 = CARTESIAN_POINT ( 'NONE',  ( -62.26029918285335896, 31.00000000000000711, 30.70375207684418228 ) ) ;
#38720 = CARTESIAN_POINT ( 'NONE',  ( 0.000000000000000000, -106.6051926090968180, -45.73109345704927620 ) ) ;
#38719 = LINE ( 'NONE', #28522, #24692 ) ;
#38721 = CIRCLE ( 'NONE', #29680, 31.49899999999999878 ) ;
#38722 = ORIENTED_EDGE ( 'NONE', *, *, #27475, .F. ) ;
#38723 = AXIS2_PLACEMENT_3D ( 'NONE', #6730, #12868, #26177 ) ;
#38724 = CIRCLE ( 'NONE', #25540, 120.5010000000000190 ) ;
#38725 = FILL_AREA_STYLE_COLOUR ( '', #15694 ) ;
#38726 = CIRCLE ( 'NONE', #19968, 59.00000000000001421 ) ;
#38727 = ORIENTED_EDGE ( 'NONE', *, *, #21360, .T. ) ;
#38728 = CARTESIAN_POINT ( 'NONE',  ( 18.00000000000000355, 0.000000000000000000, 0.000000000000000000 ) ) ;
#38729 = CARTESIAN_POINT ( 'NONE',  ( 9.000000000000001776, -47.31079789947556691, 105.9135893174949530 ) ) ;
#38730 = CARTESIAN_POINT ( 'NONE',  ( -11.85673204380701939, 31.00000000000000355, 89.11174773313419450 ) ) ;
#38732 = CARTESIAN_POINT ( 'NONE',  ( 11.57239447660066567, 40.00000000000000000, 88.72710294830137912 ) ) ;
#38731 = CIRCLE ( 'NONE', #24172, 116.0000000000000000 ) ;
#38733 = VECTOR ( 'NONE', #14007, 1000.000000000000000 ) ;
#38734 = DIRECTION ( 'NONE',  ( -1.000000000000000000, -0.000000000000000000, -0.000000000000000000 ) ) ;
#38735 = ADVANCED_FACE ( 'NONE', ( #23011 ), #30764, .T. ) ;
#38736 = AXIS2_PLACEMENT_3D ( 'NONE', #5057, #41481, #19635 ) ;
#38737 = ORIENTED_EDGE ( 'NONE', *, *, #1361, .T. ) ;
#38738 = CARTESIAN_POINT ( 'NONE',  ( 0.000000000000000000, -104.0201923570379137, 51.34003878071028026 ) ) ;
#38739 = EDGE_LOOP ( 'NONE', ( #40517, #22426, #21491, #35494 ) ) ;
#38740 = CARTESIAN_POINT ( 'NONE',  ( 18.00000000000000355, 26.17370628620655637, 39.63700417846172286 ) ) ;
#38742 = VERTEX_POINT ( 'NONE', #32989 ) ;
#38741 = FACE_OUTER_BOUND ( 'NONE', #9393, .T. ) ;
#38743 = CARTESIAN_POINT ( 'NONE',  ( 0.000000000000000000, 0.000000000000000000, 0.000000000000000000 ) ) ;
#38744 = ORIENTED_EDGE ( 'NONE', *, *, #39605, .T. ) ;
#38745 = DIRECTION ( 'NONE',  ( 0.000000000000000000, -0.3612416661871405421, -0.9324722294043605864 ) ) ;
#38746 = DIRECTION ( 'NONE',  ( 1.000000000000000000, 0.000000000000000000, 0.000000000000000000 ) ) ;
#38747 = ADVANCED_FACE ( 'NONE', ( #7619 ), #16230, .F. ) ;
#38748 = LINE ( 'NONE', #1887, #38937 ) ;
#38749 = EDGE_LOOP ( 'NONE', ( #31913, #8825, #29223, #32942 ) ) ;
#38750 = CARTESIAN_POINT ( 'NONE',  ( 24.14050371820132668, 31.00000000000000355, 13.97356841391235704 ) ) ;
#38751 = CARTESIAN_POINT ( 'NONE',  ( -36.79328511490363240, -12.05525454449572464, -55.66638716446937707 ) ) ;
#38752 = CIRCLE ( 'NONE', #41521, 36.00000000000000000 ) ;
#38753 = CIRCLE ( 'NONE', #3195, 58.99999999999999289 ) ;
#38755 = DIRECTION ( 'NONE',  ( 0.000000000000000000, 0.9574220383620042352, 0.2886919473396248326 ) ) ;
#38754 = CYLINDRICAL_SURFACE ( 'NONE', #9101, 120.5010000000000190 ) ;
#38756 = ORIENTED_EDGE ( 'NONE', *, *, #37648, .F. ) ;
#38757 = FACE_OUTER_BOUND ( 'NONE', #26673, .T. ) ;
#38758 = CARTESIAN_POINT ( 'NONE',  ( -2.855764796983342624, 2.970025579236414082, -0.09382832055445475272 ) ) ;
#38759 = CARTESIAN_POINT ( 'NONE',  ( 22.78600399168703916, 40.00000000000000000, -39.30137845373389638 ) ) ;
#38760 = CARTESIAN_POINT ( 'NONE',  ( 17.99999999999999645, -89.07460286905904923, 81.15544420874930154 ) ) ;
#38761 = CIRCLE ( 'NONE', #20003, 58.99999999999999289 ) ;
#38762 = DIRECTION ( 'NONE',  ( -1.000000000000000000, 0.000000000000000000, 0.000000000000000000 ) ) ;
#38763 = DIRECTION ( 'NONE',  ( -1.000000000000000000, 0.000000000000000000, -0.000000000000000000 ) ) ;
#38764 = ORIENTED_EDGE ( 'NONE', *, *, #34060, .T. ) ;
#38765 = CARTESIAN_POINT ( 'NONE',  ( 17.99999999999999645, -100.6739960869714139, -49.52796165323368172 ) ) ;
#38767 = EDGE_LOOP ( 'NONE', ( #33579, #23406, #2358, #27702 ) ) ;
#38766 = VECTOR ( 'NONE', #31222, 1000.000000000000000 ) ;
#38768 = EDGE_CURVE ( 'NONE', #1680, #24177, #16773, .T. ) ;
#38769 = CARTESIAN_POINT ( 'NONE',  ( 42.80287614962723808, -34.05525454449571754, 69.29271901957299917 ) ) ;
#38770 = CARTESIAN_POINT ( 'NONE',  ( 6.908545562266867002, -12.05525454449572464, -74.83297477053821467 ) ) ;
#38772 = EDGE_CURVE ( 'NONE', #26339, #26382, #39016, .T. ) ;
#38771 = CARTESIAN_POINT ( 'NONE',  ( 20.45440555730427690, 31.00000000000000355, -26.67302265141799467 ) ) ;
#38773 = VERTEX_POINT ( 'NONE', #26681 ) ;
#38774 = CARTESIAN_POINT ( 'NONE',  ( 17.99999999999999645, -51.98489025774233596, -108.7109110710166391 ) ) ;
#38775 = ORIENTED_EDGE ( 'NONE', *, *, #18162, .F. ) ;
#38776 = AXIS2_PLACEMENT_3D ( 'NONE', #16716, #37384, #6853 ) ;
#38777 = PRODUCT_DEFINITION_SHAPE ( 'NONE', 'NONE',  #43199 ) ;
#38778 = DIRECTION ( 'NONE',  ( -1.000000000000000000, 0.000000000000000000, 0.000000000000000000 ) ) ;
#38779 = CARTESIAN_POINT ( 'NONE',  ( -22.78857244739539212, 31.00000000000000355, 85.10612709700112077 ) ) ;
#38781 = VERTEX_POINT ( 'NONE', #24250 ) ;
#38780 = AXIS2_PLACEMENT_3D ( 'NONE', #15449, #15866, #19151 ) ;
#38782 = CARTESIAN_POINT ( 'NONE',  ( 57.09498703527648900, 31.00000000000000355, 3.831922229400927637 ) ) ;
#38783 = CARTESIAN_POINT ( 'NONE',  ( 70.70367055548476287, 39.99999999999999289, -62.02616482874480397 ) ) ;
#38784 = AXIS2_PLACEMENT_3D ( 'NONE', #24350, #27825, #31300 ) ;
#38785 = ADVANCED_FACE ( 'NONE', ( #39736 ), #32782, .F. ) ;
#38786 = ORIENTED_EDGE ( 'NONE', *, *, #33882, .T. ) ;
#38787 = AXIS2_PLACEMENT_3D ( 'NONE', #20370, #30384, #27119 ) ;
#38788 = DIRECTION ( 'NONE',  ( -1.000000000000000000, -0.000000000000000000, -0.000000000000000000 ) ) ;
#38789 = AXIS2_PLACEMENT_3D ( 'NONE', #15454, #12165, #1295 ) ;
#38790 = CYLINDRICAL_SURFACE ( 'NONE', #4044, 2.649999999999971934 ) ;
#38791 = CYLINDRICAL_SURFACE ( 'NONE', #24804, 59.00000000000001421 ) ;
#38792 = VECTOR ( 'NONE', #4495, 1000.000000000000000 ) ;
#38794 = VERTEX_POINT ( 'NONE', #14410 ) ;
#38793 = DIRECTION ( 'NONE',  ( 0.000000000000000000, 0.9407002666710341243, -0.3392388661180278930 ) ) ;
#38795 = CARTESIAN_POINT ( 'NONE',  ( 18.00000000000000355, -42.41764978026593269, -20.20639853260334107 ) ) ;
#38796 = DIRECTION ( 'NONE',  ( 1.000000000000000000, 0.000000000000000000, -6.546126324440850663E-16 ) ) ;
#38797 = AXIS2_PLACEMENT_3D ( 'NONE', #36606, #6727, #33560 ) ;
#38798 = EDGE_CURVE ( 'NONE', #17354, #38008, #17464, .T. ) ;
#38799 = ORIENTED_EDGE ( 'NONE', *, *, #24685, .T. ) ;
#38800 = CARTESIAN_POINT ( 'NONE',  ( -79.89583333417640176, 40.00000000000000711, 5.235987747608064957 ) ) ;
#38801 = DIRECTION ( 'NONE',  ( 1.000000000000000000, 0.000000000000000000, 0.000000000000000000 ) ) ;
#38802 = AXIS2_PLACEMENT_3D ( 'NONE', #33893, #6617, #707 ) ;
#38803 = ORIENTED_EDGE ( 'NONE', *, *, #12133, .F. ) ;
#38804 = EDGE_CURVE ( 'NONE', #596, #39282, #27918, .T. ) ;
#38805 = CARTESIAN_POINT ( 'NONE',  ( 17.99999999999999645, -51.98489025774375705, 108.7109110710159854 ) ) ;
#38806 = ORIENTED_EDGE ( 'NONE', *, *, #10761, .T. ) ;
#38807 = EDGE_CURVE ( 'NONE', #2567, #39845, #2863, .T. ) ;
#38808 = EDGE_LOOP ( 'NONE', ( #23022, #23334, #6696, #16517 ) ) ;
#38809 = CARTESIAN_POINT ( 'NONE',  ( 9.000000000000001776, 63.55543939553764687, 97.03971415477347762 ) ) ;
#38810 = VERTEX_POINT ( 'NONE', #33220 ) ;
#38811 = LINE ( 'NONE', #19015, #39021 ) ;
#38812 = DIRECTION ( 'NONE',  ( -1.000000000000000000, 0.000000000000000000, 0.000000000000000000 ) ) ;
#38813 = AXIS2_PLACEMENT_3D ( 'NONE', #17601, #25024, #7945 ) ;
#38814 = CARTESIAN_POINT ( 'NONE',  ( 17.99999999999999645, 99.97660604680052643, -67.26937820704789317 ) ) ;
#38815 = CARTESIAN_POINT ( 'NONE',  ( 21.00000000000000000, 2.055000000000000160, 0.000000000000000000 ) ) ;
#38816 = ORIENTED_EDGE ( 'NONE', *, *, #22439, .F. ) ;
#38817 = AXIS2_PLACEMENT_3D ( 'NONE', #27326, #11183, #14464 ) ;
#38818 = AXIS2_PLACEMENT_3D ( 'NONE', #21048, #34302, #3963 ) ;
#38819 = ORIENTED_EDGE ( 'NONE', *, *, #33455, .T. ) ;
#38820 = AXIS2_PLACEMENT_3D ( 'NONE', #10632, #27223, #34611 ) ;
#38821 = FACE_OUTER_BOUND ( 'NONE', #3476, .T. ) ;
#38822 = ADVANCED_FACE ( 'NONE', ( #34884 ), #21193, .F. ) ;
#38823 = EDGE_CURVE ( 'NONE', #36920, #17401, #19569, .T. ) ;
#38824 = ORIENTED_EDGE ( 'NONE', *, *, #41064, .F. ) ;
#38825 = DIRECTION ( 'NONE',  ( 0.000000000000000000, 0.9574220383620042352, 0.2886919473396248881 ) ) ;
#38826 = VECTOR ( 'NONE', #23272, 1000.000000000000000 ) ;
#38827 = EDGE_CURVE ( 'NONE', #3472, #10645, #2778, .T. ) ;
#38828 = ADVANCED_FACE ( 'NONE', ( #8280 ), #5207, .F. ) ;
#38829 = EDGE_CURVE ( 'NONE', #16730, #30917, #25159, .T. ) ;
#38830 = AXIS2_PLACEMENT_3D ( 'NONE', #17743, #17972, #37973 ) ;
#38831 = CARTESIAN_POINT ( 'NONE',  ( 18.00000000000000355, -20.99948489194451540, 42.60488980472774045 ) ) ;
#38832 = DIRECTION ( 'NONE',  ( -3.552713678800500929E-15, -6.123233995736766036E-17, -1.000000000000000000 ) ) ;
#38833 = CARTESIAN_POINT ( 'NONE',  ( 0.000000000000000000, -51.93417535146738828, -2.615612846549715709 ) ) ;
#38834 = CARTESIAN_POINT ( 'NONE',  ( -60.10416666555506993, 31.00000000000000711, -3.926990808566252156 ) ) ;
#38835 = EDGE_LOOP ( 'NONE', ( #16549, #26882, #6715, #35265 ) ) ;
#38836 = CARTESIAN_POINT ( 'NONE',  ( 17.99999999999999645, 30.01658535635262481, 108.1077105353199102 ) ) ;
#38837 = AXIS2_PLACEMENT_3D ( 'NONE', #20623, #23246, #37152 ) ;
#38838 = ORIENTED_EDGE ( 'NONE', *, *, #1791, .F. ) ;
#38839 = CARTESIAN_POINT ( 'NONE',  ( 37.24516168167158270, 40.00000000000000000, 42.45166511289891531 ) ) ;
#38840 = DIRECTION ( 'NONE',  ( 0.000000000000000000, 0.000000000000000000, 1.000000000000000000 ) ) ;
#38841 = CARTESIAN_POINT ( 'NONE',  ( 0.000000000000000000, -91.51415974874635140, 64.91094698989267897 ) ) ;
#38842 = VECTOR ( 'NONE', #30824, 1000.000000000000000 ) ;
#38843 = DIRECTION ( 'NONE',  ( -1.000000000000000000, 1.058513553088275437E-16, 0.000000000000000000 ) ) ;
#38844 = CARTESIAN_POINT ( 'NONE',  ( -19.47536345555549886, 31.00000000000000355, -6.605835105517199324 ) ) ;
#38845 = CIRCLE ( 'NONE', #15904, 51.99999999999999289 ) ;
#38846 = CIRCLE ( 'NONE', #24267, 59.00000000000000711 ) ;
#38847 = EDGE_CURVE ( 'NONE', #8080, #4507, #31616, .T. ) ;
#38848 = VERTEX_POINT ( 'NONE', #4549 ) ;
#38849 = CARTESIAN_POINT ( 'NONE',  ( 33.70925502316616473, 40.00000000000000000, 11.43906998022225707 ) ) ;
#38850 = ORIENTED_EDGE ( 'NONE', *, *, #11149, .F. ) ;
#38851 = DIRECTION ( 'NONE',  ( 0.000000000000000000, -0.9826841245925228563, 0.1852887240871046171 ) ) ;
#38852 = CARTESIAN_POINT ( 'NONE',  ( 0.000000000000000000, 0.000000000000000000, 0.000000000000000000 ) ) ;
#38853 = AXIS2_PLACEMENT_3D ( 'NONE', #18462, #12318, #35200 ) ;
#38854 = ORIENTED_EDGE ( 'NONE', *, *, #11342, .F. ) ;
#38855 = AXIS2_PLACEMENT_3D ( 'NONE', #43027, #9671, #39741 ) ;
#38856 = CARTESIAN_POINT ( 'NONE',  ( 0.000000000000000000, 5.667686777401707232, 46.64153600743607342 ) ) ;
#38857 = ORIENTED_EDGE ( 'NONE', *, *, #12721, .T. ) ;
#38858 = CARTESIAN_POINT ( 'NONE',  ( 17.99999999999999645, 0.000000000000000000, 0.000000000000000000 ) ) ;
#38859 = ORIENTED_EDGE ( 'NONE', *, *, #35712, .T. ) ;
#38860 = ORIENTED_EDGE ( 'NONE', *, *, #29609, .F. ) ;
#38861 = DIRECTION ( 'NONE',  ( -1.000000000000000000, -0.000000000000000000, -0.000000000000000000 ) ) ;
#38862 = CIRCLE ( 'NONE', #5430, 47.49900000000000233 ) ;
#38863 = CARTESIAN_POINT ( 'NONE',  ( -73.09555549758189841, 31.00000000000000711, 35.91380138263622257 ) ) ;
#38864 = VERTEX_POINT ( 'NONE', #41644 ) ;
#38865 = DIRECTION ( 'NONE',  ( 1.000000000000000000, 0.000000000000000000, 0.000000000000000000 ) ) ;
#38866 = DIRECTION ( 'NONE',  ( 0.000000000000000000, 0.000000000000000000, 1.000000000000000000 ) ) ;
#38867 = ORIENTED_EDGE ( 'NONE', *, *, #35277, .F. ) ;
#38868 = FACE_OUTER_BOUND ( 'NONE', #5661, .T. ) ;
#38869 = PRODUCT_DEFINITION_SHAPE ( 'NONE', 'NONE',  #43211 ) ;
#38870 = LINE ( 'NONE', #18864, #1820 ) ;
#38871 = CARTESIAN_POINT ( 'NONE',  ( 3.245924575715138705, 31.00000000000000355, -24.54795925723445649 ) ) ;
#38873 = ADVANCED_FACE ( 'NONE', ( #1931 ), #18572, .T. ) ;
#38872 = AXIS2_PLACEMENT_3D ( 'NONE', #17762, #24971, #1346 ) ;
#38875 = CARTESIAN_POINT ( 'NONE',  ( 17.99999999999999645, 105.7179949885863266, 37.57629584241859533 ) ) ;
#38874 = DIRECTION ( 'NONE',  ( 1.000000000000000000, 0.000000000000000000, -0.000000000000000000 ) ) ;
#38876 = EDGE_CURVE ( 'NONE', #26478, #26596, #12580, .T. ) ;
#38877 = EDGE_CURVE ( 'NONE', #9730, #25913, #4902, .T. ) ;
#38878 = DIRECTION ( 'NONE',  ( 1.000000000000000000, 0.000000000000000000, 0.000000000000000000 ) ) ;
#38879 = LINE ( 'NONE', #2417, #1948 ) ;
#38880 = VECTOR ( 'NONE', #9974, 1000.000000000000000 ) ;
#38881 = EDGE_LOOP ( 'NONE', ( #3962, #38453 ) ) ;
#38882 = AXIS2_PLACEMENT_3D ( 'NONE', #25466, #28938, #22414 ) ;
#38883 =( NAMED_UNIT ( * ) SI_UNIT ( $, .STERADIAN. ) SOLID_ANGLE_UNIT ( ) );
#38884 = EDGE_CURVE ( 'NONE', #12837, #29515, #5002, .T. ) ;
#38885 = SURFACE_STYLE_FILL_AREA ( #1373 ) ;
#38886 = AXIS2_PLACEMENT_3D ( 'NONE', #26053, #9452, #27 ) ;
#38887 = ORIENTED_EDGE ( 'NONE', *, *, #20013, .F. ) ;
#38888 = FACE_OUTER_BOUND ( 'NONE', #12129, .T. ) ;
#38889 = CYLINDRICAL_SURFACE ( 'NONE', #7749, 59.00000000000001421 ) ;
#38891 = ORIENTED_EDGE ( 'NONE', *, *, #17961, .F. ) ;
#38890 = AXIS2_PLACEMENT_3D ( 'NONE', #12483, #6121, #2390 ) ;
#38892 = CARTESIAN_POINT ( 'NONE',  ( 14.71924655979513297, 40.00000000000000000, -29.87007926703815741 ) ) ;
#38893 = CARTESIAN_POINT ( 'NONE',  ( 32.80084743084300669, 40.00000000000000000, 19.01436317119532760 ) ) ;
#38894 = EDGE_LOOP ( 'NONE', ( #14842, #22370, #14814, #37624 ) ) ;
#38895 = ORIENTED_EDGE ( 'NONE', *, *, #14879, .F. ) ;
#38896 = DIRECTION ( 'NONE',  ( 0.000000000000000000, -6.538873467836204094E-15, 1.000000000000000000 ) ) ;
#38897 = CARTESIAN_POINT ( 'NONE',  ( 0.000000000000000000, -2.123073309835498801, 47.45152853935333326 ) ) ;
#38898 = DIRECTION ( 'NONE',  ( 1.000000000000000000, 0.000000000000000000, 0.000000000000000000 ) ) ;
#38899 = DIRECTION ( 'NONE',  ( -1.000000000000000000, 0.000000000000000000, 0.000000000000000000 ) ) ;
#38900 = DIRECTION ( 'NONE',  ( 0.000000000000000000, 0.000000000000000000, 1.000000000000000000 ) ) ;
#38901 = ORIENTED_EDGE ( 'NONE', *, *, #24419, .T. ) ;
#38902 = DIRECTION ( 'NONE',  ( -1.000000000000000000, 0.000000000000000000, 0.000000000000000000 ) ) ;
#38903 = ORIENTED_EDGE ( 'NONE', *, *, #23994, .F. ) ;
#38904 = DIRECTION ( 'NONE',  ( 1.000000000000000000, 0.000000000000000000, 0.000000000000000000 ) ) ;
#38905 = FACE_OUTER_BOUND ( 'NONE', #41819, .T. ) ;
#38906 = AXIS2_PLACEMENT_3D ( 'NONE', #41000, #31427, #7847 ) ;
#38907 = CIRCLE ( 'NONE', #24328, 13.59999999999999964 ) ;
#38908 = PLANE ( 'NONE',  #12410 ) ;
#38909 = LINE ( 'NONE', #42165, #35223 ) ;
#38910 = ORIENTED_EDGE ( 'NONE', *, *, #19605, .F. ) ;
#38911 = CARTESIAN_POINT ( 'NONE',  ( -78.83182461418512332, 40.00000000000000711, -45.51551753872077910 ) ) ;
#38912 = EDGE_CURVE ( 'NONE', #12154, #25951, #15498, .T. ) ;
#38913 = VERTEX_POINT ( 'NONE', #35095 ) ;
#38914 = CIRCLE ( 'NONE', #7588, 2.649999999999971934 ) ;
#38915 = CARTESIAN_POINT ( 'NONE',  ( 0.000000000000000000, 47.49120266317495265, 0.8606222198176843863 ) ) ;
#38916 = ORIENTED_EDGE ( 'NONE', *, *, #33408, .F. ) ;
#38918 = ORIENTED_EDGE ( 'NONE', *, *, #6318, .T. ) ;
#38917 = CARTESIAN_POINT ( 'NONE',  ( 17.99999999999999645, 111.8797445107944810, -8.437727291343108504 ) ) ;
#38919 = CARTESIAN_POINT ( 'NONE',  ( -40.56882557770292408, 31.00000000000000355, 31.01417895415301373 ) ) ;
#38920 = EDGE_LOOP ( 'NONE', ( #28904, #11809, #37908, #26295 ) ) ;
#38921 = CYLINDRICAL_SURFACE ( 'NONE', #35536, 47.49900000000000233 ) ;
#38922 = FACE_BOUND ( 'NONE', #41626, .T. ) ;
#38923 = ORIENTED_EDGE ( 'NONE', *, *, #14326, .T. ) ;
#38924 = CARTESIAN_POINT ( 'NONE',  ( -23.73339997550686675, 40.00000000000000000, -70.23208777907456124 ) ) ;
#38926 = CARTESIAN_POINT ( 'NONE',  ( 0.000000000000000000, 110.3490479609632615, -20.28201389785435182 ) ) ;
#38925 = CARTESIAN_POINT ( 'NONE',  ( 18.00000000000000355, -36.05989434073592292, -30.12041790338656710 ) ) ;
#38927 = ADVANCED_FACE ( 'NONE', ( #38573 ), #31845, .F. ) ;
#38928 = CARTESIAN_POINT ( 'NONE',  ( 0.000000000000000000, 111.2721026680458749, 14.38025178762809908 ) ) ;
#38929 = ORIENTED_EDGE ( 'NONE', *, *, #517, .T. ) ;
#38930 = DIRECTION ( 'NONE',  ( -1.000000000000000000, 0.000000000000000000, 0.000000000000000000 ) ) ;
#38931 = ORIENTED_EDGE ( 'NONE', *, *, #27683, .T. ) ;
#38932 = CARTESIAN_POINT ( 'NONE',  ( 0.000000000000000000, 15.21076497709711184, 119.5371223922155792 ) ) ;
#38933 = DIRECTION ( 'NONE',  ( -1.000000000000000000, -0.000000000000000000, 0.000000000000000000 ) ) ;
#38934 = CARTESIAN_POINT ( 'NONE',  ( -45.35818215263140019, 31.00000000000000355, 51.72168634911185592 ) ) ;
#38936 = DIRECTION ( 'NONE',  ( -1.000000000000000000, 0.000000000000000000, 0.000000000000000000 ) ) ;
#38935 = CARTESIAN_POINT ( 'NONE',  ( 0.000000000000000000, -67.32409792376445523, -89.75376489259431878 ) ) ;
#38937 = VECTOR ( 'NONE', #32011, 1000.000000000000000 ) ;
#38938 = ORIENTED_EDGE ( 'NONE', *, *, #4487, .F. ) ;
#38939 = AXIS2_PLACEMENT_3D ( 'NONE', #2186, #9179, #5487 ) ;
#38940 = EDGE_CURVE ( 'NONE', #12095, #10939, #16073, .T. ) ;
#38941 = DIRECTION ( 'NONE',  ( 1.000000000000000000, 1.836909530733573776E-16, 0.000000000000000000 ) ) ;
#38942 = EDGE_CURVE ( 'NONE', #15674, #39595, #32762, .T. ) ;
#38943 = ORIENTED_EDGE ( 'NONE', *, *, #31830, .T. ) ;
#38944 = CARTESIAN_POINT ( 'NONE',  ( 17.99999999999999645, 25.46650492921896713, 19.29328419707794495 ) ) ;
#38945 = DIRECTION ( 'NONE',  ( 0.000000000000000000, 0.000000000000000000, 1.000000000000000000 ) ) ;
#38946 = CARTESIAN_POINT ( 'NONE',  ( -45.36921519482122278, 31.00000000000000711, 78.33339762288051134 ) ) ;
#38947 = CARTESIAN_POINT ( 'NONE',  ( 83.51212062389942048, 39.99999999999999289, -48.08891344038907079 ) ) ;
#38948 = DIRECTION ( 'NONE',  ( 0.000000000000000000, 0.000000000000000000, 1.000000000000000000 ) ) ;
#38949 = ORIENTED_EDGE ( 'NONE', *, *, #15660, .F. ) ;
#38950 = DIRECTION ( 'NONE',  ( -1.000000000000000000, -0.000000000000000000, -0.000000000000000000 ) ) ;
#38951 = VERTEX_POINT ( 'NONE', #22052 ) ;
#38952 = CARTESIAN_POINT ( 'NONE',  ( 17.99999999999999645, 0.000000000000000000, 0.000000000000000000 ) ) ;
#38954 = VERTEX_POINT ( 'NONE', #37716 ) ;
#38953 = CYLINDRICAL_SURFACE ( 'NONE', #42946, 13.60000000000000142 ) ;
#38955 = DIRECTION ( 'NONE',  ( -0.000000000000000000, -0.000000000000000000, -1.000000000000000000 ) ) ;
#38956 = ORIENTED_EDGE ( 'NONE', *, *, #2717, .F. ) ;
#38957 = FACE_BOUND ( 'NONE', #28967, .T. ) ;
#38958 = DIRECTION ( 'NONE',  ( 0.000000000000000000, 0.9574220383620062336, -0.2886919473396183933 ) ) ;
#38959 = DIRECTION ( 'NONE',  ( 0.000000000000000000, 0.000000000000000000, 1.000000000000000000 ) ) ;
#38960 = ORIENTED_EDGE ( 'NONE', *, *, #10616, .T. ) ;
#38961 = CARTESIAN_POINT ( 'NONE',  ( 1.622176940739286310, 31.00000000000000355, -24.60292901074088334 ) ) ;
#38962 = VECTOR ( 'NONE', #11857, 1000.000000000000000 ) ;
#38963 = DIRECTION ( 'NONE',  ( 1.000000000000000000, 1.836909530733573776E-16, 0.000000000000000000 ) ) ;
#38964 = AXIS2_PLACEMENT_3D ( 'NONE', #20021, #6877, #39167 ) ;
#38965 = AXIS2_PLACEMENT_3D ( 'NONE', #13774, #16180, #10030 ) ;
#38967 = ORIENTED_EDGE ( 'NONE', *, *, #38470, .F. ) ;
#38966 = DIRECTION ( 'NONE',  ( -1.000000000000000000, 0.000000000000000000, 0.000000000000000000 ) ) ;
#38968 = VERTEX_POINT ( 'NONE', #35314 ) ;
#38969 = CARTESIAN_POINT ( 'NONE',  ( -102.0670434220619427, -2.055254544495720648, 139.0496534599708980 ) ) ;
#38970 = CARTESIAN_POINT ( 'NONE',  ( 2.339412683011424132, -12.05525454449572464, -89.04250581823735899 ) ) ;
#38971 = CARTESIAN_POINT ( 'NONE',  ( 45.11287655886649617, 40.00000000000000000, -12.00022417491798521 ) ) ;
#38972 = DIRECTION ( 'NONE',  ( 0.000000000000000000, 2.140472356798500845E-14, -1.000000000000000000 ) ) ;
#38973 = DIRECTION ( 'NONE',  ( 0.000000000000000000, 0.000000000000000000, -1.000000000000000000 ) ) ;
#38974 = ADVANCED_FACE ( 'NONE', ( #7835 ), #31201, .F. ) ;
#38975 = CARTESIAN_POINT ( 'NONE',  ( 17.99999999999999645, 0.000000000000000000, 0.000000000000000000 ) ) ;
#38976 = ORIENTED_EDGE ( 'NONE', *, *, #23365, .T. ) ;
#38977 = CARTESIAN_POINT ( 'NONE',  ( 0.000000000000000000, 16.77727049691149475, -27.19001440037526862 ) ) ;
#38978 = EDGE_CURVE ( 'NONE', #34048, #39608, #37932, .T. ) ;
#38979 = EDGE_LOOP ( 'NONE', ( #1779, #41046, #18723, #3313 ) ) ;
#38980 = DIRECTION ( 'NONE',  ( 0.000000000000000000, 0.4610925014493266194, -0.8873520750565710991 ) ) ;
#38981 = CARTESIAN_POINT ( 'NONE',  ( 17.99999999999999645, -110.1579703617967567, 21.29539948940213634 ) ) ;
#38982 = CARTESIAN_POINT ( 'NONE',  ( -39.95047694894377344, 31.00000000000000355, -5.256506769647570465 ) ) ;
#38983 = ORIENTED_EDGE ( 'NONE', *, *, #12708, .F. ) ;
#38984 = SURFACE_STYLE_USAGE ( .BOTH. , #32238 ) ;
#38985 = VERTEX_POINT ( 'NONE', #15261 ) ;
#38986 = EDGE_CURVE ( 'NONE', #21881, #33572, #703, .T. ) ;
#38987 = DIRECTION ( 'NONE',  ( -1.000000000000000000, -0.000000000000000000, -0.000000000000000000 ) ) ;
#38988 = CARTESIAN_POINT ( 'NONE',  ( 22.58587702529213104, 31.00000000000000355, 84.29678642628191199 ) ) ;
#38989 = AXIS2_PLACEMENT_3D ( 'NONE', #25297, #11972, #29190 ) ;
#38990 = AXIS2_PLACEMENT_3D ( 'NONE', #20271, #20479, #37449 ) ;
#38991 = ADVANCED_FACE ( 'NONE', ( #12174 ), #32019, .T. ) ;
#38992 = PLANE ( 'NONE',  #22028 ) ;
#38993 = ORIENTED_EDGE ( 'NONE', *, *, #14398, .F. ) ;
#38994 = CARTESIAN_POINT ( 'NONE',  ( -41.78821403078461572, 31.00000000000000355, -47.79414628086201589 ) ) ;
#38995 = CARTESIAN_POINT ( 'NONE',  ( -35.33737842959504860, 40.00000000000000000, 60.98257694382487415 ) ) ;
#38996 = CARTESIAN_POINT ( 'NONE',  ( 72.43982367323130234, 39.99999999999999289, 63.53091779346544143 ) ) ;
#38997 = VERTEX_POINT ( 'NONE', #21600 ) ;
#38998 =( REPRESENTATION_RELATIONSHIP ('NONE','NONE', #330, #18009 ) REPRESENTATION_RELATIONSHIP_WITH_TRANSFORMATION ( #3875 )SHAPE_REPRESENTATION_RELATIONSHIP( ) );
#38999 = FACE_OUTER_BOUND ( 'NONE', #12221, .T. ) ;
#39000 = DIRECTION ( 'NONE',  ( 0.000000000000000000, 0.000000000000000000, 1.000000000000000000 ) ) ;
#39001 = FACE_OUTER_BOUND ( 'NONE', #22668, .T. ) ;
#39003 = VERTEX_POINT ( 'NONE', #25493 ) ;
#39002 = CARTESIAN_POINT ( 'NONE',  ( 4.000000000000000000, 2.309401076758497151, -3.433295621305379353 ) ) ;
#39004 = DIRECTION ( 'NONE',  ( -1.000000000000000000, 0.000000000000000000, 0.000000000000000000 ) ) ;
#39005 = DIRECTION ( 'NONE',  ( 1.000000000000000000, 1.836909530733573776E-16, 0.000000000000000000 ) ) ;
#39006 = ORIENTED_EDGE ( 'NONE', *, *, #24249, .F. ) ;
#39007 = CARTESIAN_POINT ( 'NONE',  ( 65.81435062899562638, 39.99999999999999289, 37.99825742656441463 ) ) ;
#39008 = CYLINDRICAL_SURFACE ( 'NONE', #43073, 47.49900000000000233 ) ;
#39009 = EDGE_CURVE ( 'NONE', #4850, #22654, #11905, .T. ) ;
#39010 = ORIENTED_EDGE ( 'NONE', *, *, #21583, .F. ) ;
#39011 = EDGE_CURVE ( 'NONE', #28805, #26249, #9755, .T. ) ;
#39012 = CARTESIAN_POINT ( 'NONE',  ( -2.797566391619251075E-15, 1.860994515641065082E-14, 7.000000000000002665 ) ) ;
#39013 = ORIENTED_EDGE ( 'NONE', *, *, #23934, .T. ) ;
#39014 = ORIENTED_EDGE ( 'NONE', *, *, #41286, .T. ) ;
#39015 = FACE_OUTER_BOUND ( 'NONE', #28669, .T. ) ;
#39017 = ORIENTED_EDGE ( 'NONE', *, *, #16253, .T. ) ;
#39016 = CIRCLE ( 'NONE', #36210, 20.00000000000000355 ) ;
#39018 = CYLINDRICAL_SURFACE ( 'NONE', #9072, 59.00000000000000000 ) ;
#39019 = CIRCLE ( 'NONE', #6294, 13.60000000000000142 ) ;
#39020 = CARTESIAN_POINT ( 'NONE',  ( 18.00000000000000355, 0.000000000000000000, 0.000000000000000000 ) ) ;
#39021 = VECTOR ( 'NONE', #25342, 1000.000000000000000 ) ;
#39022 = CARTESIAN_POINT ( 'NONE',  ( 17.99999999999999645, 92.10690493017145286, -64.06707842432085442 ) ) ;
#39023 = DIRECTION ( 'NONE',  ( 1.000000000000000000, 0.000000000000000000, 0.000000000000000000 ) ) ;
#39024 = ORIENTED_EDGE ( 'NONE', *, *, #9749, .T. ) ;
#39025 = CARTESIAN_POINT ( 'NONE',  ( 17.99999999999999645, 0.000000000000000000, 0.000000000000000000 ) ) ;
#39026 = ADVANCED_FACE ( 'NONE', ( #8885 ), #38754, .F. ) ;
#39027 = UNCERTAINTY_MEASURE_WITH_UNIT (LENGTH_MEASURE( 1.000000000000000082E-05 ), #41067, 'distance_accuracy_value', 'NONE');
#39028 = ORIENTED_EDGE ( 'NONE', *, *, #21298, .F. ) ;
#39029 = CARTESIAN_POINT ( 'NONE',  ( 18.00000000000000355, 0.000000000000000000, 0.000000000000000000 ) ) ;
#39030 = ORIENTED_EDGE ( 'NONE', *, *, #37553, .F. ) ;
#39031 = CARTESIAN_POINT ( 'NONE',  ( 18.00000000000000355, 0.000000000000000000, 0.000000000000000000 ) ) ;
#39032 = DIRECTION ( 'NONE',  ( -1.000000000000000000, -0.000000000000000000, 0.000000000000000000 ) ) ;
#39033 = EDGE_CURVE ( 'NONE', #24964, #7188, #7004, .T. ) ;
#39034 = CARTESIAN_POINT ( 'NONE',  ( 0.000000000000000000, 99.97660604680052643, -67.26937820704789317 ) ) ;
#39035 = CARTESIAN_POINT ( 'NONE',  ( -40.54929543462775143, 31.00000000000000355, -46.21859917192507794 ) ) ;
#39036 = ORIENTED_EDGE ( 'NONE', *, *, #34361, .F. ) ;
#39037 = FACE_OUTER_BOUND ( 'NONE', #36107, .T. ) ;
#39038 = CIRCLE ( 'NONE', #20284, 130.0000000000000284 ) ;
#39039 = EDGE_CURVE ( 'NONE', #18280, #22812, #5396, .T. ) ;
#39040 = VERTEX_POINT ( 'NONE', #41156 ) ;
#39041 = CARTESIAN_POINT ( 'NONE',  ( 17.12248163736668261, 31.00000000000000355, 34.87662400048955647 ) ) ;
#39042 = CARTESIAN_POINT ( 'NONE',  ( -9.469526743414824921, 40.00000000000000000, -71.82433816204535049 ) ) ;
#39043 = AXIS2_PLACEMENT_3D ( 'NONE', #35698, #36135, #12607 ) ;
#39044 = AXIS2_PLACEMENT_3D ( 'NONE', #22879, #36122, #42874 ) ;
#39045 = AXIS2_PLACEMENT_3D ( 'NONE', #15825, #22600, #31973 ) ;
#39046 = CARTESIAN_POINT ( 'NONE',  ( 17.99999999999999645, 0.000000000000000000, 0.000000000000000000 ) ) ;
#39047 = CARTESIAN_POINT ( 'NONE',  ( 0.000000000000000000, -16.86122981692000167, -27.13802899033310112 ) ) ;
#39048 = AXIS2_PLACEMENT_3D ( 'NONE', #11764, #34857, #39180 ) ;
#39049 = CIRCLE ( 'NONE', #13312, 13.59999999999999964 ) ;
#39050 = DIRECTION ( 'NONE',  ( -1.770125995894701695E-16, 1.000000000000000000, 0.000000000000000000 ) ) ;
#39051 = DIRECTION ( 'NONE',  ( 1.000000000000000000, 0.000000000000000000, 0.000000000000000000 ) ) ;
#39052 = ORIENTED_EDGE ( 'NONE', *, *, #9409, .T. ) ;
#39053 = CARTESIAN_POINT ( 'NONE',  ( 28.34477777927418529, 40.00000000000000000, 36.93558740410973229 ) ) ;
#39054 = CARTESIAN_POINT ( 'NONE',  ( 17.99999999999999645, 0.000000000000000000, 0.000000000000000000 ) ) ;
#39055 = DIRECTION ( 'NONE',  ( 0.000000000000000000, 0.000000000000000000, -1.000000000000000000 ) ) ;
#39056 = ORIENTED_EDGE ( 'NONE', *, *, #19227, .T. ) ;
#39057 = EDGE_CURVE ( 'NONE', #16946, #1540, #19598, .T. ) ;
#39058 = CARTESIAN_POINT ( 'NONE',  ( 18.00000000000000355, 44.47301969247467923, -16.68249143361863318 ) ) ;
#39059 = FACE_OUTER_BOUND ( 'NONE', #25379, .T. ) ;
#39060 = EDGE_CURVE ( 'NONE', #25006, #33094, #14017, .T. ) ;
#39061 = ORIENTED_EDGE ( 'NONE', *, *, #40509, .F. ) ;
#39062 = DIRECTION ( 'NONE',  ( 0.000000000000000000, 0.3612416661871538093, -0.9324722294043554793 ) ) ;
#39063 = ORIENTED_EDGE ( 'NONE', *, *, #21530, .T. ) ;
#39064 = ORIENTED_EDGE ( 'NONE', *, *, #24701, .T. ) ;
#39065 = CARTESIAN_POINT ( 'NONE',  ( 0.000000000000000000, 68.63002662989747193, 93.51962064069530811 ) ) ;
#39066 = CARTESIAN_POINT ( 'NONE',  ( 11.20008397362390618, 31.00000000000000355, -84.14439686172904942 ) ) ;
#39067 = ORIENTED_EDGE ( 'NONE', *, *, #40417, .T. ) ;
#39068 = CARTESIAN_POINT ( 'NONE',  ( 18.00000000000000355, -27.43636312076294814, -38.14186064215179073 ) ) ;
#39069 = AXIS2_PLACEMENT_3D ( 'NONE', #35856, #5982, #19337 ) ;
#39070 = CYLINDRICAL_SURFACE ( 'NONE', #2418, 13.59999999999999964 ) ;
#39071 = ORIENTED_EDGE ( 'NONE', *, *, #34653, .T. ) ;
#39072 = CYLINDRICAL_SURFACE ( 'NONE', #17584, 36.00000000000000000 ) ;
#39073 = EDGE_CURVE ( 'NONE', #27001, #25725, #5615, .T. ) ;
#39074 = EDGE_CURVE ( 'NONE', #3831, #41306, #4962, .T. ) ;
#39075 = DIRECTION ( 'NONE',  ( 1.000000000000000000, 0.000000000000000000, 0.000000000000000000 ) ) ;
#39076 = VECTOR ( 'NONE', #5345, 1000.000000000000000 ) ;
#39077 = CIRCLE ( 'NONE', #41891, 51.99999999999999289 ) ;
#39078 = DIRECTION ( 'NONE',  ( -1.000000000000000000, 0.000000000000000000, 0.000000000000000000 ) ) ;
#39080 = PLANE ( 'NONE',  #12875 ) ;
#39079 = LINE ( 'NONE', #29721, #12711 ) ;
#39081 = AXIS2_PLACEMENT_3D ( 'NONE', #1448, #4503, #25079 ) ;
#39082 = SHAPE_REPRESENTATION ( 'housing left', ( #13552 ), #23961 ) ;
#39083 = CARTESIAN_POINT ( 'NONE',  ( -132.0000507999999968, 0.000000000000000000, 0.000000000000000000 ) ) ;
#39084 = ORIENTED_EDGE ( 'NONE', *, *, #20319, .T. ) ;
#39085 =( NAMED_UNIT ( * ) PLANE_ANGLE_UNIT ( ) SI_UNIT ( $, .RADIAN. ) );
#39086 = ADVANCED_FACE ( 'NONE', ( #11523 ), #38534, .T. ) ;
#39087 = CARTESIAN_POINT ( 'NONE',  ( -23.46968090759046888, 31.00000000000000355, -20.57717900685300449 ) ) ;
#39088 = AXIS2_PLACEMENT_3D ( 'NONE', #11112, #4763, #37486 ) ;
#39089 = ORIENTED_EDGE ( 'NONE', *, *, #8496, .T. ) ;
#39090 = DIRECTION ( 'NONE',  ( -1.000000000000000000, 0.000000000000000000, -0.000000000000000000 ) ) ;
#39091 = EDGE_CURVE ( 'NONE', #3822, #7775, #25857, .T. ) ;
#39092 = CYLINDRICAL_SURFACE ( 'NONE', #11258, 116.0000000000000000 ) ;
#39093 = ORIENTED_EDGE ( 'NONE', *, *, #23993, .T. ) ;
#39094 = CARTESIAN_POINT ( 'NONE',  ( 19.70274684888802952, 40.00000000000000000, 17.27304525429847359 ) ) ;
#39095 = CARTESIAN_POINT ( 'NONE',  ( 32.62694724487211317, 40.00000000000000000, -16.02036196159510339 ) ) ;
#39096 = VERTEX_POINT ( 'NONE', #24638 ) ;
#39097 = ORIENTED_EDGE ( 'NONE', *, *, #928, .F. ) ;
#39098 = DIRECTION ( 'NONE',  ( 1.000000000000000000, -1.373900992973642263E-15, -3.996523416598957436E-16 ) ) ;
#39099 = DIRECTION ( 'NONE',  ( -3.009274222672345096E-17, -1.000000000000000000, 2.455023325076454960E-18 ) ) ;
#39100 = DIRECTION ( 'NONE',  ( 0.000000000000000000, 0.000000000000000000, 1.000000000000000000 ) ) ;
#39101 = CARTESIAN_POINT ( 'NONE',  ( -2.000000000000007550, -3.464101615137749945, 0.000000000000000000 ) ) ;
#39102 = DIRECTION ( 'NONE',  ( -1.000000000000000000, -0.000000000000000000, -0.000000000000000000 ) ) ;
#39103 = CARTESIAN_POINT ( 'NONE',  ( 17.99999999999999645, 0.000000000000000000, 0.000000000000000000 ) ) ;
#39104 = ORIENTED_EDGE ( 'NONE', *, *, #33029, .T. ) ;
#39105 = DIRECTION ( 'NONE',  ( 0.000000000000000000, 0.000000000000000000, 1.000000000000000000 ) ) ;
#39106 = ORIENTED_EDGE ( 'NONE', *, *, #10281, .T. ) ;
#39107 = DIRECTION ( 'NONE',  ( 0.000000000000000000, 0.000000000000000000, -1.000000000000000000 ) ) ;
#39108 = VECTOR ( 'NONE', #17566, 1000.000000000000000 ) ;
#39109 = CYLINDRICAL_SURFACE ( 'NONE', #29108, 116.0000000000000000 ) ;
#39110 = VECTOR ( 'NONE', #27404, 1000.000000000000000 ) ;
#39111 = EDGE_CURVE ( 'NONE', #34589, #32501, #20292, .T. ) ;
#39112 = ADVANCED_FACE ( 'NONE', ( #28756 ), #2297, .T. ) ;
#39113 = LINE ( 'NONE', #9237, #34681 ) ;
#39114 = EDGE_CURVE ( 'NONE', #10741, #10211, #41607, .T. ) ;
#39115 = EDGE_CURVE ( 'NONE', #32554, #18274, #11757, .T. ) ;
#39116 = CIRCLE ( 'NONE', #1498, 20.00000000000000711 ) ;
#39117 = CARTESIAN_POINT ( 'NONE',  ( 0.000000000000000000, -22.82995208772716467, 41.06517797613655318 ) ) ;
#39118 = ORIENTED_EDGE ( 'NONE', *, *, #39864, .T. ) ;
#39119 = CARTESIAN_POINT ( 'NONE',  ( 90.64482129758324902, 39.99999999999999289, 30.77200948131585889 ) ) ;
#39120 = ORIENTED_EDGE ( 'NONE', *, *, #37018, .F. ) ;
#39121 = DIRECTION ( 'NONE',  ( -1.000000000000000000, 0.000000000000000000, 0.000000000000000000 ) ) ;
#39122 = CIRCLE ( 'NONE', #30094, 59.00000000000001421 ) ;
#39123 = ORIENTED_EDGE ( 'NONE', *, *, #42990, .T. ) ;
#39125 = EDGE_LOOP ( 'NONE', ( #43005, #2121, #38282, #12402 ) ) ;
#39124 = DIRECTION ( 'NONE',  ( 0.000000000000000000, 0.8477344278896721264, -0.5304209081197406306 ) ) ;
#39126 = CARTESIAN_POINT ( 'NONE',  ( 53.62204311759385433, 31.00000000000000355, -18.10832464707264577 ) ) ;
#39127 = ORIENTED_EDGE ( 'NONE', *, *, #33533, .T. ) ;
#39128 = DIRECTION ( 'NONE',  ( -1.000000000000000000, 0.000000000000000000, 0.000000000000000000 ) ) ;
#39129 = DIRECTION ( 'NONE',  ( 0.000000000000000000, 0.000000000000000000, 1.000000000000000000 ) ) ;
#39130 = PRODUCT_DEFINITION_SHAPE ( 'NONE', 'NONE',  #43186 ) ;
#39131 = ORIENTED_EDGE ( 'NONE', *, *, #9519, .F. ) ;
#39132 = CARTESIAN_POINT ( 'NONE',  ( 30.38134496340388324, 40.00000000000000000, 61.85720693096894252 ) ) ;
#39134 = LINE ( 'NONE', #26497, #26957 ) ;
#39133 = CARTESIAN_POINT ( 'NONE',  ( 17.99999999999999645, -87.92975456462950490, 69.68953103478128241 ) ) ;
#39135 = CARTESIAN_POINT ( 'NONE',  ( 17.99999999999999645, 88.56657216608614647, 68.87840567545953263 ) ) ;
#39136 = ORIENTED_EDGE ( 'NONE', *, *, #9767, .T. ) ;
#39137 = CARTESIAN_POINT ( 'NONE',  ( -109.0695705685748607, -106.4195705685759776, 6.999999999999998224 ) ) ;
#39138 = ORIENTED_EDGE ( 'NONE', *, *, #31466, .F. ) ;
#39139 = DIRECTION ( 'NONE',  ( 1.000000000000000000, 0.000000000000000000, 0.000000000000000000 ) ) ;
#39140 = CARTESIAN_POINT ( 'NONE',  ( -10.00000000000000000, 0.000000000000000000, 0.000000000000000000 ) ) ;
#39141 = AXIS2_PLACEMENT_3D ( 'NONE', #1116, #31026, #10308 ) ;
#39142 = CARTESIAN_POINT ( 'NONE',  ( 10.81967497908702214, 31.00000000000000355, -82.17651821321413763 ) ) ;
#39144 = DIRECTION ( 'NONE',  ( 0.000000000000000000, 1.000000000000000000, 1.224646799147353207E-16 ) ) ;
#39143 = PLANE ( 'NONE',  #19825 ) ;
#39145 = ORIENTED_EDGE ( 'NONE', *, *, #11635, .F. ) ;
#39146 = CIRCLE ( 'NONE', #10603, 59.00000000000000000 ) ;
#39147 = AXIS2_PLACEMENT_3D ( 'NONE', #5512, #28660, #8143 ) ;
#39148 = VERTEX_POINT ( 'NONE', #2728 ) ;
#39149 = CARTESIAN_POINT ( 'NONE',  ( 109.0695705685763244, -106.4195705685744855, 9.999999999999998224 ) ) ;
#39150 = CARTESIAN_POINT ( 'NONE',  ( 17.99999999999999645, 79.94368240339547071, -90.16373242487824768 ) ) ;
#39151 = CARTESIAN_POINT ( 'NONE',  ( 87.78546986788515483, 31.00000000000000000, 43.41392487578124104 ) ) ;
#39152 = CARTESIAN_POINT ( 'NONE',  ( 86.58052584568750376, 39.99999999999999289, -42.55516686010646765 ) ) ;
#39153 = CARTESIAN_POINT ( 'NONE',  ( 17.99999999999999645, 88.56657216608705596, -68.87840567545838155 ) ) ;
#39154 = ORIENTED_EDGE ( 'NONE', *, *, #10007, .T. ) ;
#39155 = DIRECTION ( 'NONE',  ( 0.000000000000000000, 0.000000000000000000, 1.000000000000000000 ) ) ;
#39156 = ORIENTED_EDGE ( 'NONE', *, *, #4012, .T. ) ;
#39157 = CARTESIAN_POINT ( 'NONE',  ( 17.99999999999999645, -6.854627147197943415, -115.7972974066014018 ) ) ;
#39158 = CARTESIAN_POINT ( 'NONE',  ( 17.99999999999999645, 12.43843445475317822, 111.5058645182329968 ) ) ;
#39159 = EDGE_CURVE ( 'NONE', #11580, #255, #9523, .T. ) ;
#39160 = EDGE_CURVE ( 'NONE', #37436, #10195, #3498, .T. ) ;
#39161 = DIRECTION ( 'NONE',  ( 1.000000000000000000, 0.000000000000000000, 0.000000000000000000 ) ) ;
#39162 = VERTEX_POINT ( 'NONE', #29389 ) ;
#39163 = DIRECTION ( 'NONE',  ( 0.000000000000000000, 0.000000000000000000, 1.000000000000000000 ) ) ;
#39164 = DIRECTION ( 'NONE',  ( 0.000000000000000000, 0.000000000000000000, 1.000000000000000000 ) ) ;
#39165 = EDGE_CURVE ( 'NONE', #9752, #33321, #9785, .T. ) ;
#39166 = AXIS2_PLACEMENT_3D ( 'NONE', #20959, #13961, #30539 ) ;
#39167 = DIRECTION ( 'NONE',  ( 0.000000000000000000, -0.9980267284282723361, 0.06279051952930261860 ) ) ;
#39168 = CIRCLE ( 'NONE', #37092, 31.49899999999999878 ) ;
#39169 = ORIENTED_EDGE ( 'NONE', *, *, #36396, .T. ) ;
#39170 = CARTESIAN_POINT ( 'NONE',  ( -3.169834189307652927, 31.00000000000000355, -24.13593742708953016 ) ) ;
#39171 = DIRECTION ( 'NONE',  ( -1.000000000000000000, 0.000000000000000000, 0.000000000000000000 ) ) ;
#39172 = CIRCLE ( 'NONE', #28070, 2.100000000000000089 ) ;
#39174 = ORIENTED_EDGE ( 'NONE', *, *, #19091, .T. ) ;
#39173 = DIRECTION ( 'NONE',  ( 1.000000000000000000, 0.000000000000000000, 0.000000000000000000 ) ) ;
#39175 = EDGE_LOOP ( 'NONE', ( #17059, #41788, #1898, #33904 ) ) ;
#39176 = CARTESIAN_POINT ( 'NONE',  ( 4.000000000000000000, -2.309401076758514915, -5.000000000000000000 ) ) ;
#39177 = DIRECTION ( 'NONE',  ( -1.000000000000000000, 0.000000000000000000, 0.000000000000000000 ) ) ;
#39179 = CARTESIAN_POINT ( 'NONE',  ( 42.86166521172830102, 40.00000000000000000, 21.22462828019262204 ) ) ;
#39178 = AXIS2_PLACEMENT_3D ( 'NONE', #34265, #4361, #31002 ) ;
#39180 = DIRECTION ( 'NONE',  ( 0.000000000000000000, -0.6783118362696075598, -0.7347741508630750706 ) ) ;
#39181 = EDGE_CURVE ( 'NONE', #35178, #18183, #19382, .T. ) ;
#39182 = FACE_OUTER_BOUND ( 'NONE', #27606, .T. ) ;
#39183 = CARTESIAN_POINT ( 'NONE',  ( -102.9608013043458072, -14.05525454449570688, 14.45886780445738218 ) ) ;
#39184 = EDGE_LOOP ( 'NONE', ( #12651, #576, #17596, #31478 ) ) ;
#39185 = CARTESIAN_POINT ( 'NONE',  ( 17.99999999999999645, -107.2703412112697094, 32.88383143828427535 ) ) ;
#39186 = VERTEX_POINT ( 'NONE', #28965 ) ;
#39187 = DIRECTION ( 'NONE',  ( 0.000000000000000000, 0.000000000000000000, 1.000000000000000000 ) ) ;
#39188 = DIRECTION ( 'NONE',  ( 0.000000000000000000, 0.000000000000000000, 1.000000000000000000 ) ) ;
#39189 = CARTESIAN_POINT ( 'NONE',  ( -27.33276042269523387, 31.00000000000000355, -31.15086293565511966 ) ) ;
#39190 = CARTESIAN_POINT ( 'NONE',  ( 17.99999999999999645, 76.48293397876260258, 82.08917884620340999 ) ) ;
#39191 = VERTEX_POINT ( 'NONE', #42658 ) ;
#39192 = EDGE_CURVE ( 'NONE', #26141, #42150, #10506, .T. ) ;
#39193 = LINE ( 'NONE', #22465, #10747 ) ;
#39194 = CARTESIAN_POINT ( 'NONE',  ( -29.64342647699677613, 31.00000000000000355, -87.27882330658468391 ) ) ;
#39195 = CARTESIAN_POINT ( 'NONE',  ( 17.99999999999999645, 114.1529630473449686, 38.59523323561477781 ) ) ;
#39196 = ORIENTED_EDGE ( 'NONE', *, *, #2383, .T. ) ;
#39197 = CARTESIAN_POINT ( 'NONE',  ( 45.08926718328532246, 31.00000000000000355, 51.56349680124436219 ) ) ;
#39198 = AXIS2_PLACEMENT_3D ( 'NONE', #22235, #42018, #16295 ) ;
#39199 = CARTESIAN_POINT ( 'NONE',  ( 45.08926718327026606, 40.00000000000000000, 51.56349680124436219 ) ) ;
#39200 = DIRECTION ( 'NONE',  ( 1.000000000000000000, 0.000000000000000000, 0.000000000000000000 ) ) ;
#39201 = VERTEX_POINT ( 'NONE', #3152 ) ;
#39202 = CIRCLE ( 'NONE', #25318, 36.00000000000000000 ) ;
#39203 = CARTESIAN_POINT ( 'NONE',  ( 0.000000000000000000, 108.8684555192046872, 27.12806418649654105 ) ) ;
#39204 = DIRECTION ( 'NONE',  ( 1.000000000000000000, 0.000000000000000000, 0.000000000000000000 ) ) ;
#39206 = ORIENTED_EDGE ( 'NONE', *, *, #42840, .T. ) ;
#39205 = DIRECTION ( 'NONE',  ( 0.000000000000000000, -0.6382441836448109473, -0.7698339834299138262 ) ) ;
#39207 = EDGE_CURVE ( 'NONE', #39608, #15819, #4933, .T. ) ;
#39208 = CARTESIAN_POINT ( 'NONE',  ( 0.000000000000000000, 100.6739960869717834, 49.52796165323294986 ) ) ;
#39209 = CARTESIAN_POINT ( 'NONE',  ( -105.0363123600777442, 40.00000000000000000, -2.692529638013756887 ) ) ;
#39210 = ORIENTED_EDGE ( 'NONE', *, *, #34482, .F. ) ;
#39211 = CARTESIAN_POINT ( 'NONE',  ( -66.92166868300088822, 40.00000000000000711, -22.71661802240650019 ) ) ;
#39212 = DIRECTION ( 'NONE',  ( -1.000000000000000000, -0.000000000000000000, -0.000000000000000000 ) ) ;
#39213 = EDGE_LOOP ( 'NONE', ( #31363, #40526, #15807, #4921 ) ) ;
#39214 = DIRECTION ( 'NONE',  ( 0.000000000000000000, 0.000000000000000000, 1.000000000000000000 ) ) ;
#39215 = LINE ( 'NONE', #39862, #23216 ) ;
#39216 = ADVANCED_FACE ( 'NONE', ( #3378 ), #13248, .T. ) ;
#39217 = ORIENTED_EDGE ( 'NONE', *, *, #28181, .T. ) ;
#39218 = EDGE_CURVE ( 'NONE', #14987, #8291, #20988, .T. ) ;
#39219 = CIRCLE ( 'NONE', #41316, 59.00000000000000000 ) ;
#39220 = ORIENTED_EDGE ( 'NONE', *, *, #7553, .T. ) ;
#39221 = CARTESIAN_POINT ( 'NONE',  ( -20.64238946400878305, 40.00000000000000000, 3.177240882809045708 ) ) ;
#39222 = EDGE_LOOP ( 'NONE', ( #13657, #23079, #30558, #33243 ) ) ;
#39223 = DIRECTION ( 'NONE',  ( -1.000000000000000000, -0.000000000000000000, -0.000000000000000000 ) ) ;
#39224 = DIRECTION ( 'NONE',  ( 0.000000000000000000, 2.211037379550099895E-14, -1.000000000000000000 ) ) ;
#39225 = ADVANCED_FACE ( 'NONE', ( #2935 ), #23083, .F. ) ;
#39226 = DIRECTION ( 'NONE',  ( 0.000000000000000000, 0.7164567402983162969, -0.6976315211349835010 ) ) ;
#39227 = CARTESIAN_POINT ( 'NONE',  ( 0.000000000000000000, -80.02407177072905142, -78.64108602300026973 ) ) ;
#39228 = ORIENTED_EDGE ( 'NONE', *, *, #3084, .F. ) ;
#39230 = LINE ( 'NONE', #9149, #24515 ) ;
#39229 = COLOUR_RGB ( '', 0.66274510, 0.83137255, 0.94901961) ;
#39231 = ORIENTED_EDGE ( 'NONE', *, *, #23504, .F. ) ;
#39232 = CARTESIAN_POINT ( 'NONE',  ( 17.99999999999999645, 0.000000000000000000, 0.000000000000000000 ) ) ;
#39233 = ORIENTED_EDGE ( 'NONE', *, *, #22498, .T. ) ;
#39234 = CARTESIAN_POINT ( 'NONE',  ( 0.000000000000000000, -112.1702510623870239, -2.471285140323770335 ) ) ;
#39235 = DIRECTION ( 'NONE',  ( 0.000000000000000000, 0.000000000000000000, 1.000000000000000000 ) ) ;
#39236 = AXIS2_PLACEMENT_3D ( 'NONE', #29124, #36480, #22591 ) ;
#39237 = CARTESIAN_POINT ( 'NONE',  ( 17.99999999999999645, 68.63002662989747193, 93.51962064069530811 ) ) ;
#39238 = CARTESIAN_POINT ( 'NONE',  ( 54.85378563033546584, 31.00000000000000355, 7.219977902337870290 ) ) ;
#39239 = ADVANCED_FACE ( 'NONE', ( #29600 ), #20028, .T. ) ;
#39240 = FACE_OUTER_BOUND ( 'NONE', #11948, .T. ) ;
#39241 = CIRCLE ( 'NONE', #41338, 47.49900000000000233 ) ;
#39242 = VERTEX_POINT ( 'NONE', #36539 ) ;
#39243 = CARTESIAN_POINT ( 'NONE',  ( -8.786317949316114095, 31.00000000000000355, -33.00646673688142840 ) ) ;
#39244 = AXIS2_PLACEMENT_3D ( 'NONE', #29788, #24502, #37752 ) ;
#39245 = CARTESIAN_POINT ( 'NONE',  ( -34.23962737045593485, 40.00000000000000000, 59.30561363632230609 ) ) ;
#39246 = FACE_OUTER_BOUND ( 'NONE', #31106, .T. ) ;
#39247 = CARTESIAN_POINT ( 'NONE',  ( 9.000000000000001776, 12.30077720129167851, -50.52416135122069107 ) ) ;
#39248 = CARTESIAN_POINT ( 'NONE',  ( 18.00000000000000355, 47.22458491092820765, 5.098390039074388369 ) ) ;
#39249 = DIRECTION ( 'NONE',  ( -1.000000000000000000, 0.000000000000000000, 0.000000000000000000 ) ) ;
#39250 = EDGE_CURVE ( 'NONE', #27794, #22079, #16803, .T. ) ;
#39251 = ORIENTED_EDGE ( 'NONE', *, *, #27935, .F. ) ;
#39252 = CARTESIAN_POINT ( 'NONE',  ( -10.91816144241376563, 40.00000000000000000, -40.73603723627661566 ) ) ;
#39253 = CARTESIAN_POINT ( 'NONE',  ( -10.00000000000000000, 0.000000000000000000, 0.000000000000000000 ) ) ;
#39254 = CIRCLE ( 'NONE', #2324, 58.99999999999999289 ) ;
#39255 = CARTESIAN_POINT ( 'NONE',  ( -101.9959696149863930, 31.00000000000000355, -0.1269066430507536924 ) ) ;
#39256 = ORIENTED_EDGE ( 'NONE', *, *, #3271, .F. ) ;
#39257 = DIRECTION ( 'NONE',  ( -1.000000000000000000, -0.000000000000000000, -0.000000000000000000 ) ) ;
#39258 = DIRECTION ( 'NONE',  ( 1.000000000000000000, -1.373900992973642263E-15, 0.000000000000000000 ) ) ;
#39259 = ORIENTED_EDGE ( 'NONE', *, *, #6523, .F. ) ;
#39260 = CARTESIAN_POINT ( 'NONE',  ( 0.000000000000000000, 107.2703412112694963, 32.88383143828500721 ) ) ;
#39261 = VERTEX_POINT ( 'NONE', #43095 ) ;
#39262 = EDGE_CURVE ( 'NONE', #21384, #291, #41831, .T. ) ;
#39263 = ORIENTED_EDGE ( 'NONE', *, *, #6907, .F. ) ;
#39264 = AXIS2_PLACEMENT_3D ( 'NONE', #16726, #4003, #43074 ) ;
#39265 = DIRECTION ( 'NONE',  ( -1.000000000000000000, -0.000000000000000000, -0.000000000000000000 ) ) ;
#39266 = CARTESIAN_POINT ( 'NONE',  ( 68.41293481155882716, 31.00000000000000000, -52.34142988146868447 ) ) ;
#39267 = VERTEX_POINT ( 'NONE', #36329 ) ;
#39268 = DIRECTION ( 'NONE',  ( 0.000000000000000000, 0.000000000000000000, 1.000000000000000000 ) ) ;
#39269 = AXIS2_PLACEMENT_3D ( 'NONE', #29906, #19661, #3006 ) ;
#39270 = CARTESIAN_POINT ( 'NONE',  ( 18.00000000000000355, 24.72041153920788403, -40.55929306992662475 ) ) ;
#39271 = EDGE_CURVE ( 'NONE', #26760, #39508, #6446, .T. ) ;
#39272 = CARTESIAN_POINT ( 'NONE',  ( 0.000000000000000000, -29.60891106212812574, 37.14118181634756155 ) ) ;
#39273 = ORIENTED_EDGE ( 'NONE', *, *, #2446, .F. ) ;
#39274 = CARTESIAN_POINT ( 'NONE',  ( 0.000000000000000000, 97.97378550988226209, 62.10585602713792497 ) ) ;
#39275 = VECTOR ( 'NONE', #12432, 1000.000000000000000 ) ;
#39276 = DIRECTION ( 'NONE',  ( -1.000000000000000000, 0.000000000000000000, -0.000000000000000000 ) ) ;
#39277 = FACE_OUTER_BOUND ( 'NONE', #21620, .T. ) ;
#39279 = CARTESIAN_POINT ( 'NONE',  ( 0.000000000000000000, -15.49408907645141653, -44.90087086784608061 ) ) ;
#39278 = CARTESIAN_POINT ( 'NONE',  ( 17.99999999999999645, -0.04937522221101428577, -31.94951095880159286 ) ) ;
#39280 = DIRECTION ( 'NONE',  ( 0.000000000000000000, 0.000000000000000000, 1.000000000000000000 ) ) ;
#39281 = AXIS2_PLACEMENT_3D ( 'NONE', #24055, #10954, #41235 ) ;
#39282 = VERTEX_POINT ( 'NONE', #12392 ) ;
#39283 = DIRECTION ( 'NONE',  ( -0.06205737506068762649, 1.862744738831246665E-18, 0.9980725836333634859 ) ) ;
#39284 = CARTESIAN_POINT ( 'NONE',  ( 22.22924588317381023, 31.00000000000000355, -25.35314793696836588 ) ) ;
#39285 = AXIS2_PLACEMENT_3D ( 'NONE', #11829, #4826, #18619 ) ;
#39286 = ADVANCED_FACE ( 'NONE', ( #2519 ), #42453, .T. ) ;
#39287 = ORIENTED_EDGE ( 'NONE', *, *, #29198, .F. ) ;
#39288 = DIRECTION ( 'NONE',  ( -1.000000000000000000, -0.000000000000000000, -0.000000000000000000 ) ) ;
#39289 = EDGE_CURVE ( 'NONE', #26508, #27767, #30731, .T. ) ;
#39290 = CARTESIAN_POINT ( 'NONE',  ( 0.000000000000000000, 0.000000000000000000, 0.000000000000000000 ) ) ;
#39291 = VERTEX_POINT ( 'NONE', #35687 ) ;
#39292 = DIRECTION ( 'NONE',  ( 0.000000000000000000, 0.000000000000000000, 1.000000000000000000 ) ) ;
#39293 = CARTESIAN_POINT ( 'NONE',  ( 31.10108666877329853, 40.00000000000000000, 17.95223046116557697 ) ) ;
#39294 = AXIS2_PLACEMENT_3D ( 'NONE', #34635, #1678, #18117 ) ;
#39295 = CARTESIAN_POINT ( 'NONE',  ( -30.84436395684957333, 40.00000000000000000, -10.52363363425145337 ) ) ;
#39296 = AXIS2_PLACEMENT_3D ( 'NONE', #22499, #23346, #26603 ) ;
#39297 = EDGE_LOOP ( 'NONE', ( #34619, #5310, #31630, #17239 ) ) ;
#39298 = VECTOR ( 'NONE', #12312, 1000.000000000000000 ) ;
#39299 = EDGE_LOOP ( 'NONE', ( #11487, #24973, #20376, #18721 ) ) ;
#39300 = CARTESIAN_POINT ( 'NONE',  ( 0.000000000000000000, -66.49630760163661591, 90.36876423295966276 ) ) ;
#39301 = DIRECTION ( 'NONE',  ( -1.000000000000000000, 0.000000000000000000, 0.000000000000000000 ) ) ;
#39302 = VECTOR ( 'NONE', #2322, 1000.000000000000000 ) ;
#39303 = CARTESIAN_POINT ( 'NONE',  ( 17.99999999999999645, 7.749090474611513457, 30.53094492177216068 ) ) ;
#39304 = CARTESIAN_POINT ( 'NONE',  ( 17.99999999999999645, 89.07460286905850921, 81.15544420874991260 ) ) ;
#39305 = DIRECTION ( 'NONE',  ( -1.000000000000000000, 0.000000000000000000, 0.000000000000000000 ) ) ;
#39306 = VERTEX_POINT ( 'NONE', #5808 ) ;
#39307 = DIRECTION ( 'NONE',  ( 0.000000000000000000, -0.6845471059286950544, 0.7289686274214053352 ) ) ;
#39308 = ORIENTED_EDGE ( 'NONE', *, *, #28676, .F. ) ;
#39309 = DIRECTION ( 'NONE',  ( 1.000000000000000000, 0.000000000000000000, 0.000000000000000000 ) ) ;
#39310 = DIRECTION ( 'NONE',  ( -1.000000000000000000, 0.000000000000000000, -0.000000000000000000 ) ) ;
#39311 = CARTESIAN_POINT ( 'NONE',  ( 0.000000000000000000, 63.24564713401792204, 102.5693868539697178 ) ) ;
#39312 = DIRECTION ( 'NONE',  ( -1.000000000000000000, -0.000000000000000000, -0.000000000000000000 ) ) ;
#39313 = ORIENTED_EDGE ( 'NONE', *, *, #4911, .T. ) ;
#39314 = DIRECTION ( 'NONE',  ( 0.000000000000000000, 0.000000000000000000, 1.000000000000000000 ) ) ;
#39315 = VERTEX_POINT ( 'NONE', #20670 ) ;
#39316 = CARTESIAN_POINT ( 'NONE',  ( 0.000000000000000000, 0.000000000000000000, 0.000000000000000000 ) ) ;
#39317 = DIRECTION ( 'NONE',  ( -1.000000000000000000, 0.000000000000000000, 0.000000000000000000 ) ) ;
#39318 = VECTOR ( 'NONE', #9263, 999.9999999999998863 ) ;
#39319 = EDGE_CURVE ( 'NONE', #32698, #36927, #17177, .T. ) ;
#39320 = VERTEX_POINT ( 'NONE', #17399 ) ;
#39322 = VERTEX_POINT ( 'NONE', #27401 ) ;
#39321 = DIRECTION ( 'NONE',  ( -1.000000000000000000, -0.000000000000000000, -0.000000000000000000 ) ) ;
#39323 = CARTESIAN_POINT ( 'NONE',  ( 17.81483206087466442, 31.00000000000000355, -52.17936214187551514 ) ) ;
#39324 = EDGE_CURVE ( 'NONE', #10364, #13484, #23773, .T. ) ;
#39325 = EDGE_LOOP ( 'NONE', ( #35512, #22108 ) ) ;
#39326 = CARTESIAN_POINT ( 'NONE',  ( 17.99999999999999645, 61.59243992711585491, -93.77976230225978327 ) ) ;
#39327 = AXIS2_PLACEMENT_3D ( 'NONE', #30467, #21272, #38230 ) ;
#39328 = EDGE_LOOP ( 'NONE', ( #39989, #3524, #4882, #12577 ) ) ;
#39329 = CARTESIAN_POINT ( 'NONE',  ( 0.000000000000000000, 0.000000000000000000, 0.000000000000000000 ) ) ;
#39330 = CIRCLE ( 'NONE', #29624, 120.5010000000000474 ) ;
#39331 = ORIENTED_EDGE ( 'NONE', *, *, #27184, .T. ) ;
#39332 = CARTESIAN_POINT ( 'NONE',  ( -69.31868535678037802, 40.00000000000000711, 18.45717643660483986 ) ) ;
#39333 = AXIS2_PLACEMENT_3D ( 'NONE', #29722, #40369, #33616 ) ;
#39335 = DIRECTION ( 'NONE',  ( 1.000000000000000000, 0.000000000000000000, 0.000000000000000000 ) ) ;
#39334 = CARTESIAN_POINT ( 'NONE',  ( 17.99999999999999645, -75.72520367775142347, 82.78868281115956052 ) ) ;
#39336 = TOROIDAL_SURFACE ( 'NONE', #17098, 19.59999999999999432, 0.4000000000000001887 ) ;
#39337 = FACE_OUTER_BOUND ( 'NONE', #20417, .T. ) ;
#39338 = ORIENTED_EDGE ( 'NONE', *, *, #12619, .T. ) ;
#39339 = CYLINDRICAL_SURFACE ( 'NONE', #36993, 100.0000000000000000 ) ;
#39340 = VERTEX_POINT ( 'NONE', #6882 ) ;
#39341 = SHAPE_REPRESENTATION_RELATIONSHIP ( 'NONE' , 'NONE' ,  #15194, #11465 ) ;
#39342 = AXIS2_PLACEMENT_3D ( 'NONE', #6651, #26529, #40451 ) ;
#39343 = FACE_OUTER_BOUND ( 'NONE', #13081, .T. ) ;
#39344 = CARTESIAN_POINT ( 'NONE',  ( -1.420922472151883646E-13, 9.833206111663764869E-13, 369.6955262170047831 ) ) ;
#39345 = EDGE_CURVE ( 'NONE', #28038, #22999, #11052, .T. ) ;
#39346 = CARTESIAN_POINT ( 'NONE',  ( 48.66231590553977071, 31.00000000000000000, -55.48862040801125062 ) ) ;
#39347 = EDGE_CURVE ( 'NONE', #16681, #42378, #4025, .T. ) ;
#39349 = DIRECTION ( 'NONE',  ( 0.000000000000000000, 1.000000000000000000, 0.000000000000000000 ) ) ;
#39348 = FACE_OUTER_BOUND ( 'NONE', #39700, .T. ) ;
#39350 = VERTEX_POINT ( 'NONE', #33937 ) ;
#39351 = EDGE_CURVE ( 'NONE', #26484, #38810, #21710, .T. ) ;
#39352 = EDGE_CURVE ( 'NONE', #41913, #42713, #11215, .T. ) ;
#39353 = VERTEX_POINT ( 'NONE', #7305 ) ;
#39354 = DIRECTION ( 'NONE',  ( 0.000000000000000000, 0.000000000000000000, -1.000000000000000000 ) ) ;
#39355 = CARTESIAN_POINT ( 'NONE',  ( 42.80287614962790599, -34.05525454449571754, 69.29271901957253021 ) ) ;
#39357 = CARTESIAN_POINT ( 'NONE',  ( 96.90013369365226481, 31.00000000000000000, -6.223598210838602540 ) ) ;
#39356 = AXIS2_PLACEMENT_3D ( 'NONE', #24597, #37635, #7544 ) ;
#39358 = CARTESIAN_POINT ( 'NONE',  ( 30.72743980831338462, 40.00000000000000000, -90.12673907452091271 ) ) ;
#39359 = AXIS2_PLACEMENT_3D ( 'NONE', #34363, #24588, #38487 ) ;
#39360 = DIRECTION ( 'NONE',  ( -1.000000000000000000, 0.000000000000000000, 0.000000000000000000 ) ) ;
#39361 = CIRCLE ( 'NONE', #7295, 13.60000000000000142 ) ;
#39362 = CIRCLE ( 'NONE', #12252, 59.00000000000000000 ) ;
#39363 = LINE ( 'NONE', #29808, #31161 ) ;
#39364 = ORIENTED_EDGE ( 'NONE', *, *, #24830, .T. ) ;
#39365 = CARTESIAN_POINT ( 'NONE',  ( 17.99999999999999645, -119.8996782608630838, 12.02323392193314966 ) ) ;
#39366 = ORIENTED_EDGE ( 'NONE', *, *, #26522, .T. ) ;
#39367 = LINE ( 'NONE', #12791, #38085 ) ;
#39368 = CIRCLE ( 'NONE', #22031, 59.00000000000000711 ) ;
#39369 = AXIS2_PLACEMENT_3D ( 'NONE', #23699, #10360, #4002 ) ;
#39370 = CARTESIAN_POINT ( 'NONE',  ( 8.999999999999998224, 101.1403355683146117, 56.80345518653519576 ) ) ;
#39371 = DIRECTION ( 'NONE',  ( 1.000000000000000000, 0.000000000000000000, 0.000000000000000000 ) ) ;
#39372 = VERTEX_POINT ( 'NONE', #7538 ) ;
#39373 = DIRECTION ( 'NONE',  ( 0.000000000000000000, 0.000000000000000000, 1.000000000000000000 ) ) ;
#39374 = CARTESIAN_POINT ( 'NONE',  ( -19.74979319748359430, 117.9447454555042754, 2.972870684497276539 ) ) ;
#39375 = AXIS2_PLACEMENT_3D ( 'NONE', #20599, #33870, #7901 ) ;
#39376 = EDGE_CURVE ( 'NONE', #28381, #26365, #34169, .T. ) ;
#39377 = DIRECTION ( 'NONE',  ( -1.000000000000000000, 0.000000000000000000, -0.000000000000000000 ) ) ;
#39379 = VERTEX_POINT ( 'NONE', #34147 ) ;
#39378 = CARTESIAN_POINT ( 'NONE',  ( -31.74999999999995737, 0.000000000000000000, 0.000000000000000000 ) ) ;
#39380 = CARTESIAN_POINT ( 'NONE',  ( 3.245924575715138705, 31.00000000000000355, -24.54795925723445649 ) ) ;
#39381 = EDGE_CURVE ( 'NONE', #17417, #553, #26521, .T. ) ;
#39382 = CARTESIAN_POINT ( 'NONE',  ( 0.000000000000000000, 116.0452958106484971, -32.46506308663343532 ) ) ;
#39383 = EDGE_CURVE ( 'NONE', #27149, #39261, #33709, .T. ) ;
#39385 = ORIENTED_EDGE ( 'NONE', *, *, #11472, .T. ) ;
#39384 = DIRECTION ( 'NONE',  ( -1.000000000000000000, 0.000000000000000000, 0.000000000000000000 ) ) ;
#39386 = VERTEX_POINT ( 'NONE', #40669 ) ;
#39387 = CARTESIAN_POINT ( 'NONE',  ( -10.50000000000000178, 1.285879139104721028E-15, 0.000000000000000000 ) ) ;
#39388 = DIRECTION ( 'NONE',  ( 0.000000000000000000, -0.4817536741017223179, 0.8763066800438596982 ) ) ;
#39389 = CARTESIAN_POINT ( 'NONE',  ( 12.49611804805956439, 40.00000000000000000, 37.00809541493615740 ) ) ;
#39390 = CARTESIAN_POINT ( 'NONE',  ( -101.1532682021072134, 17.11489954122026447, -3.256983028635321187 ) ) ;
#39391 = VECTOR ( 'NONE', #17363, 1000.000000000000000 ) ;
#39392 = FACE_OUTER_BOUND ( 'NONE', #25020, .T. ) ;
#39393 = CIRCLE ( 'NONE', #18575, 120.5010000000000190 ) ;
#39394 = CARTESIAN_POINT ( 'NONE',  ( 17.99999999999999645, 91.65951123222482977, 71.09524597798119316 ) ) ;
#39396 = EDGE_LOOP ( 'NONE', ( #20481, #34836, #11289, #23900 ) ) ;
#39395 = VECTOR ( 'NONE', #37097, 1000.000000000000000 ) ;
#39397 = CARTESIAN_POINT ( 'NONE',  ( 18.00000000000000355, -46.19362259308827845, -8.585149169758995669 ) ) ;
#39398 = CONICAL_SURFACE ( 'NONE', #35943, 2.041999999999999815, 1.047197551196591858 ) ;
#39399 = ORIENTED_EDGE ( 'NONE', *, *, #15188, .F. ) ;
#39400 = CIRCLE ( 'NONE', #42890, 59.00000000000000000 ) ;
#39401 = CARTESIAN_POINT ( 'NONE',  ( 17.99999999999999645, -71.21168426767047777, -86.70160608319397966 ) ) ;
#39402 = CARTESIAN_POINT ( 'NONE',  ( 1.798435537469519230E-14, -1.196353617197826191E-13, -44.99999999999999289 ) ) ;
#39403 = AXIS2_PLACEMENT_3D ( 'NONE', #26504, #19987, #19129 ) ;
#39404 = CARTESIAN_POINT ( 'NONE',  ( -22.94860596549062848, 31.00000000000000355, -46.53072237555588231 ) ) ;
#39406 = ORIENTED_EDGE ( 'NONE', *, *, #3906, .T. ) ;
#39405 =( GEOMETRIC_REPRESENTATION_CONTEXT ( 3 ) GLOBAL_UNCERTAINTY_ASSIGNED_CONTEXT ( ( #754 ) ) GLOBAL_UNIT_ASSIGNED_CONTEXT ( ( #18890, #10246, #32147 ) ) REPRESENTATION_CONTEXT ( 'NONE', 'WORKASPACE' ) );
#39407 = EDGE_CURVE ( 'NONE', #40263, #34617, #5645, .T. ) ;
#39408 = EDGE_CURVE ( 'NONE', #16293, #38951, #40897, .T. ) ;
#39409 = AXIS2_PLACEMENT_3D ( 'NONE', #4381, #2918, #42637 ) ;
#39410 = EDGE_CURVE ( 'NONE', #5566, #10311, #16834, .T. ) ;
#39412 = CIRCLE ( 'NONE', #1805, 13.59999999999999787 ) ;
#39411 = CARTESIAN_POINT ( 'NONE',  ( 17.99999999999999645, 0.000000000000000000, 0.000000000000000000 ) ) ;
#39413 = CARTESIAN_POINT ( 'NONE',  ( 61.87885091699251916, 31.00000000000000000, -70.55635664373320992 ) ) ;
#39414 = CARTESIAN_POINT ( 'NONE',  ( 0.000000000000000000, 75.03166794516924654, -94.29071961951432002 ) ) ;
#39415 = ORIENTED_EDGE ( 'NONE', *, *, #32149, .F. ) ;
#39416 = CARTESIAN_POINT ( 'NONE',  ( 28.99662776679064891, 31.00000000000000355, -58.58186007941694129 ) ) ;
#39417 = CARTESIAN_POINT ( 'NONE',  ( -4.113979049837106494, 40.00000000000000000, -64.40000927351898952 ) ) ;
#39418 = EDGE_CURVE ( 'NONE', #40010, #24356, #36997, .T. ) ;
#39419 = CARTESIAN_POINT ( 'NONE',  ( -99.14707074559267141, 40.00000000000000711, 13.06922382031732610 ) ) ;
#39420 = VERTEX_POINT ( 'NONE', #30241 ) ;
#39421 = DIRECTION ( 'NONE',  ( 0.000000000000000000, 0.000000000000000000, 1.000000000000000000 ) ) ;
#39422 = EDGE_CURVE ( 'NONE', #36553, #9338, #18935, .T. ) ;
#39423 = CARTESIAN_POINT ( 'NONE',  ( 0.000000000000000000, -104.0201923570372173, -51.34003878071168003 ) ) ;
#39424 = CARTESIAN_POINT ( 'NONE',  ( 17.99999999999999645, -31.11570115861491814, -4.898994019976963266 ) ) ;
#39425 = VECTOR ( 'NONE', #25749, 1000.000000000000000 ) ;
#39427 = VERTEX_POINT ( 'NONE', #36769 ) ;
#39426 = CYLINDRICAL_SURFACE ( 'NONE', #33868, 13.60000000000000142 ) ;
#39428 = AXIS2_PLACEMENT_3D ( 'NONE', #8257, #5181, #11113 ) ;
#39429 = CARTESIAN_POINT ( 'NONE',  ( 106.4195705685734623, 106.4195705685780524, 7.000000000000250466 ) ) ;
#39430 = CIRCLE ( 'NONE', #35238, 1.999999999999988010 ) ;
#39431 = PLANE ( 'NONE',  #16813 ) ;
#39432 = AXIS2_PLACEMENT_3D ( 'NONE', #36742, #40436, #39996 ) ;
#39433 = CARTESIAN_POINT ( 'NONE',  ( 50.46169669344906339, 40.00000000000000000, 57.51940134901310131 ) ) ;
#39434 = CYLINDRICAL_SURFACE ( 'NONE', #39583, 36.00000000000000000 ) ;
#39435 = AXIS2_PLACEMENT_3D ( 'NONE', #14463, #36907, #23423 ) ;
#39436 = ORIENTED_EDGE ( 'NONE', *, *, #27901, .T. ) ;
#39437 = AXIS2_PLACEMENT_3D ( 'NONE', #42132, #42357, #12505 ) ;
#39438 = DIRECTION ( 'NONE',  ( -1.000000000000000000, 0.000000000000000000, 0.000000000000000000 ) ) ;
#39439 = CARTESIAN_POINT ( 'NONE',  ( 0.000000000000000000, 13.57797752207923381, 33.34124362422479493 ) ) ;
#39440 = VERTEX_POINT ( 'NONE', #20239 ) ;
#39441 = EDGE_CURVE ( 'NONE', #8823, #39420, #33500, .T. ) ;
#39442 = ORIENTED_EDGE ( 'NONE', *, *, #17550, .T. ) ;
#39443 = CARTESIAN_POINT ( 'NONE',  ( -2.600000000000000533, -12.75000000000000000, -1.199999999999999956 ) ) ;
#39444 = EDGE_LOOP ( 'NONE', ( #21957, #38351, #41716, #38574 ) ) ;
#39445 = CYLINDRICAL_SURFACE ( 'NONE', #18228, 12.59999999999999964 ) ;
#39446 = CARTESIAN_POINT ( 'NONE',  ( 1.039096088315723056E-14, -6.912265343809663812E-14, -26.00000000000000355 ) ) ;
#39447 = CIRCLE ( 'NONE', #14423, 58.99999999999998579 ) ;
#39448 = LINE ( 'NONE', #32914, #34462 ) ;
#39449 = DIRECTION ( 'NONE',  ( 1.000000000000000000, -0.000000000000000000, -0.000000000000000000 ) ) ;
#39450 = ORIENTED_EDGE ( 'NONE', *, *, #10034, .F. ) ;
#39451 = CARTESIAN_POINT ( 'NONE',  ( 0.000000000000000000, 42.87700105098753056, -107.7847984684000551 ) ) ;
#39452 = VERTEX_POINT ( 'NONE', #307 ) ;
#39453 = CARTESIAN_POINT ( 'NONE',  ( 17.99999999999999645, 0.000000000000000000, 0.000000000000000000 ) ) ;
#39455 = ORIENTED_EDGE ( 'NONE', *, *, #13580, .F. ) ;
#39454 = VECTOR ( 'NONE', #14148, 1000.000000000000000 ) ;
#39456 = DIRECTION ( 'NONE',  ( 0.000000000000000000, 0.000000000000000000, -1.000000000000000000 ) ) ;
#39457 = ADVANCED_FACE ( 'NONE', ( #13673 ), #26973, .F. ) ;
#39458 = CARTESIAN_POINT ( 'NONE',  ( 17.99999999999999645, 19.12429268481864142, -114.4126803693777248 ) ) ;
#39459 = AXIS2_PLACEMENT_3D ( 'NONE', #21612, #34859, #4974 ) ;
#39460 = AXIS2_PLACEMENT_3D ( 'NONE', #16016, #35813, #42583 ) ;
#39461 = SHAPE_DEFINITION_REPRESENTATION ( #20401, #40225 ) ;
#39462 = LINE ( 'NONE', #16613, #21912 ) ;
#39463 = CARTESIAN_POINT ( 'NONE',  ( -38.74991464700507748, 31.00000000000000355, 44.18781823130588293 ) ) ;
#39464 = DIRECTION ( 'NONE',  ( 0.000000000000000000, 0.5963673585384969833, 0.8027116379309670036 ) ) ;
#39465 = ORIENTED_EDGE ( 'NONE', *, *, #16442, .T. ) ;
#39467 = CARTESIAN_POINT ( 'NONE',  ( -31.89861325429239258, 31.00000000000000355, 2.042328591206914012 ) ) ;
#39466 = AXIS2_PLACEMENT_3D ( 'NONE', #40707, #27885, #23541 ) ;
#39468 = CARTESIAN_POINT ( 'NONE',  ( 63.32575250126041055, 39.99999999999999289, 16.95471465585521997 ) ) ;
#39469 = ADVANCED_FACE ( 'NONE', ( #7092 ), #38280, .F. ) ;
#39470 = AXIS2_PLACEMENT_3D ( 'NONE', #5018, #35331, #38387 ) ;
#39471 = CIRCLE ( 'NONE', #20733, 116.0000000000000000 ) ;
#39472 = DIRECTION ( 'NONE',  ( -1.000000000000000000, 0.000000000000000000, 0.000000000000000000 ) ) ;
#39473 = EDGE_CURVE ( 'NONE', #7715, #26178, #16133, .T. ) ;
#39474 = CARTESIAN_POINT ( 'NONE',  ( 9.000000000000001776, -58.30069736313733131, 100.2847380560565256 ) ) ;
#39475 = CARTESIAN_POINT ( 'NONE',  ( 17.99999999999999645, 94.83915810436401728, 59.94836581341619564 ) ) ;
#39476 = DIRECTION ( 'NONE',  ( -1.000000000000000000, 0.000000000000000000, -0.000000000000000000 ) ) ;
#39477 = EDGE_LOOP ( 'NONE', ( #31454, #5653, #19853, #37352 ) ) ;
#39478 = CARTESIAN_POINT ( 'NONE',  ( 26.55430347651023837, 40.00000000000000000, -34.62409890758566178 ) ) ;
#39479 = DIRECTION ( 'NONE',  ( 0.000000000000000000, -0.4817536741017036661, -0.8763066800438700232 ) ) ;
#39480 = DIRECTION ( 'NONE',  ( 1.000000000000000000, 1.836909530733573776E-16, 0.000000000000000000 ) ) ;
#39481 = ORIENTED_EDGE ( 'NONE', *, *, #9795, .F. ) ;
#39482 = CIRCLE ( 'NONE', #12376, 20.00000000000000711 ) ;
#39483 = DIRECTION ( 'NONE',  ( -1.000000000000000000, -0.000000000000000000, -0.000000000000000000 ) ) ;
#39484 = CARTESIAN_POINT ( 'NONE',  ( 0.000000000000000000, -84.77518783075143460, 73.49448960231327987 ) ) ;
#39485 = ORIENTED_EDGE ( 'NONE', *, *, #16440, .F. ) ;
#39486 = CARTESIAN_POINT ( 'NONE',  ( 18.00000000000000355, -46.11014828289837197, -9.022736828081200144 ) ) ;
#39487 = EDGE_LOOP ( 'NONE', ( #84, #6191, #21822, #21129 ) ) ;
#39488 = AXIS2_PLACEMENT_3D ( 'NONE', #21034, #14896, #11616 ) ;
#39489 = AXIS2_PLACEMENT_3D ( 'NONE', #39697, #32950, #10038 ) ;
#39490 = EDGE_CURVE ( 'NONE', #36133, #5078, #25444, .T. ) ;
#39491 = ORIENTED_EDGE ( 'NONE', *, *, #33197, .F. ) ;
#39492 = AXIS2_PLACEMENT_3D ( 'NONE', #28626, #21470, #35359 ) ;
#39493 = CARTESIAN_POINT ( 'NONE',  ( -36.94957890273524725, -2.055254544495720648, 165.5452302238048503 ) ) ;
#39494 = CARTESIAN_POINT ( 'NONE',  ( -80.50242771303932443, 31.00000000000000711, -46.62292012068298419 ) ) ;
#39495 = ORIENTED_EDGE ( 'NONE', *, *, #38621, .F. ) ;
#39496 = LINE ( 'NONE', #39704, #4261 ) ;
#39497 = CIRCLE ( 'NONE', #40901, 120.5010000000000332 ) ;
#39498 = LINE ( 'NONE', #39270, #29622 ) ;
#39499 = DIRECTION ( 'NONE',  ( 0.000000000000000000, 0.000000000000000000, 1.000000000000000000 ) ) ;
#39500 = ORIENTED_EDGE ( 'NONE', *, *, #15192, .F. ) ;
#39501 = DIRECTION ( 'NONE',  ( -3.996523416598930318E-16, 2.658563593772947863E-15, 1.000000000000000000 ) ) ;
#39502 = APPLICATION_CONTEXT ( 'automotive_design' ) ;
#39503 = LINE ( 'NONE', #26014, #8781 ) ;
#39505 = DIRECTION ( 'NONE',  ( 0.000000000000000000, -1.287488025362403787E-15, -1.000000000000000000 ) ) ;
#39504 = DIRECTION ( 'NONE',  ( -1.000000000000000000, -0.000000000000000000, -0.000000000000000000 ) ) ;
#39506 = DIRECTION ( 'NONE',  ( 0.000000000000000000, 0.000000000000000000, 1.000000000000000000 ) ) ;
#39507 = EDGE_CURVE ( 'NONE', #880, #1858, #27976, .T. ) ;
#39508 = VERTEX_POINT ( 'NONE', #18272 ) ;
#39509 = DIRECTION ( 'NONE',  ( 1.000000000000000000, 0.000000000000000000, 0.000000000000000000 ) ) ;
#39510 = CARTESIAN_POINT ( 'NONE',  ( -14.08558183832706234, 31.00000000000000355, -28.55406316770863739 ) ) ;
#39511 = ORIENTED_EDGE ( 'NONE', *, *, #40753, .F. ) ;
#39512 = CARTESIAN_POINT ( 'NONE',  ( 17.99999999999999645, 12.42760411676086996, -33.78690065568411427 ) ) ;
#39513 = CARTESIAN_POINT ( 'NONE',  ( 17.99999999999999645, 46.12538073176499154, -111.3235835452206857 ) ) ;
#39514 = AXIS2_PLACEMENT_3D ( 'NONE', #3725, #23867, #684 ) ;
#39515 = ORIENTED_EDGE ( 'NONE', *, *, #16197, .T. ) ;
#39516 = LINE ( 'NONE', #6571, #29936 ) ;
#39517 = CARTESIAN_POINT ( 'NONE',  ( 16.30133787010129254, 40.00000000000000000, 33.04822796959624753 ) ) ;
#39518 = AXIS2_PLACEMENT_3D ( 'NONE', #27120, #39733, #26895 ) ;
#39519 = CARTESIAN_POINT ( 'NONE',  ( -30.89738163651703928, 40.00000000000000000, 40.13100860032159289 ) ) ;
#39520 = EDGE_CURVE ( 'NONE', #19587, #6806, #41160, .T. ) ;
#39521 = CIRCLE ( 'NONE', #15905, 116.0000000000000000 ) ;
#39522 = VECTOR ( 'NONE', #12508, 1000.000000000000000 ) ;
#39523 = VERTEX_POINT ( 'NONE', #34579 ) ;
#39524 = VERTEX_POINT ( 'NONE', #35222 ) ;
#39525 = DIRECTION ( 'NONE',  ( -1.000000000000000000, -0.000000000000000000, -0.000000000000000000 ) ) ;
#39526 = EDGE_CURVE ( 'NONE', #7422, #8430, #21742, .T. ) ;
#39527 = DIRECTION ( 'NONE',  ( -1.000000000000000000, 0.000000000000000000, -0.000000000000000000 ) ) ;
#39528 = AXIS2_PLACEMENT_3D ( 'NONE', #10743, #37129, #6818 ) ;
#39529 = ADVANCED_FACE ( 'NONE', ( #31974 ), #28286, .T. ) ;
#39530 = DIRECTION ( 'NONE',  ( 0.000000000000000000, 0.000000000000000000, 1.000000000000000000 ) ) ;
#39531 = CARTESIAN_POINT ( 'NONE',  ( 9.000000000000001776, -104.6166166098448826, 50.11350645393640235 ) ) ;
#39532 = DIRECTION ( 'NONE',  ( -3.009274222672345096E-17, -1.000000000000000000, 2.455023325076454960E-18 ) ) ;
#39533 = ORIENTED_EDGE ( 'NONE', *, *, #16561, .T. ) ;
#39534 = DIRECTION ( 'NONE',  ( 1.000000000000000000, 0.000000000000000000, -3.273063162220425331E-16 ) ) ;
#39535 = ORIENTED_EDGE ( 'NONE', *, *, #16347, .F. ) ;
#39536 = DIRECTION ( 'NONE',  ( 0.000000000000000000, -1.000000000000000000, 0.000000000000000000 ) ) ;
#39537 = DIRECTION ( 'NONE',  ( -1.000000000000000000, 0.000000000000000000, -0.000000000000000000 ) ) ;
#39538 = AXIS2_PLACEMENT_3D ( 'NONE', #12602, #13044, #25920 ) ;
#39539 = DIRECTION ( 'NONE',  ( 0.000000000000000000, 0.1837495178165706178, -0.9829730996839017854 ) ) ;
#39540 = DIRECTION ( 'NONE',  ( 1.000000000000000000, 0.000000000000000000, 0.000000000000000000 ) ) ;
#39541 = VERTEX_POINT ( 'NONE', #4458 ) ;
#39542 = LINE ( 'NONE', #13186, #38205 ) ;
#39543 = ORIENTED_EDGE ( 'NONE', *, *, #20931, .T. ) ;
#39544 = CARTESIAN_POINT ( 'NONE',  ( 0.000000000000000000, 0.000000000000000000, 0.000000000000000000 ) ) ;
#39545 = EDGE_CURVE ( 'NONE', #41964, #8913, #8453, .T. ) ;
#39546 = VERTEX_POINT ( 'NONE', #41553 ) ;
#39548 = ORIENTED_EDGE ( 'NONE', *, *, #14324, .F. ) ;
#39547 = CARTESIAN_POINT ( 'NONE',  ( 0.000000000000000000, 46.19362259308835661, 8.585149169758654608 ) ) ;
#39549 = CARTESIAN_POINT ( 'NONE',  ( 34.31975892712151222, 31.00000000000000355, 59.64049725130579560 ) ) ;
#39551 = EDGE_CURVE ( 'NONE', #10089, #1932, #31753, .T. ) ;
#39550 = ORIENTED_EDGE ( 'NONE', *, *, #18658, .F. ) ;
#39552 = CARTESIAN_POINT ( 'NONE',  ( 17.99999999999999645, -32.49609705003715732, 15.49205204337262565 ) ) ;
#39553 = AXIS2_PLACEMENT_3D ( 'NONE', #39484, #32739, #37084 ) ;
#39554 = CIRCLE ( 'NONE', #29818, 2.649999999999973266 ) ;
#39555 = ORIENTED_EDGE ( 'NONE', *, *, #15812, .T. ) ;
#39556 = CIRCLE ( 'NONE', #37488, 59.00000000000000000 ) ;
#39557 = CARTESIAN_POINT ( 'NONE',  ( -101.9959696149863788, 40.00000000000000711, -0.1269066430510139010 ) ) ;
#39558 = VERTEX_POINT ( 'NONE', #15415 ) ;
#39559 = AXIS2_PLACEMENT_3D ( 'NONE', #39083, #25400, #25617 ) ;
#39560 = CARTESIAN_POINT ( 'NONE',  ( -62.56443097449947288, 40.00000000000000000, -55.02758207457567607 ) ) ;
#39561 = AXIS2_PLACEMENT_3D ( 'NONE', #25594, #8975, #22322 ) ;
#39563 = CARTESIAN_POINT ( 'NONE',  ( 0.000000000000000000, -35.54274411427983438, -115.1399337407609949 ) ) ;
#39562 = FACE_OUTER_BOUND ( 'NONE', #19760, .T. ) ;
#39564 = DIRECTION ( 'NONE',  ( 1.000000000000000000, 0.000000000000000000, -0.000000000000000000 ) ) ;
#39565 = ORIENTED_EDGE ( 'NONE', *, *, #30862, .T. ) ;
#39566 = DIRECTION ( 'NONE',  ( 0.000000000000000000, 0.000000000000000000, 1.000000000000000000 ) ) ;
#39567 = EDGE_CURVE ( 'NONE', #40561, #16448, #5119, .T. ) ;
#39568 = ORIENTED_EDGE ( 'NONE', *, *, #6677, .F. ) ;
#39569 = DIRECTION ( 'NONE',  ( -1.000000000000000000, 0.000000000000000000, 0.000000000000000000 ) ) ;
#39570 = DIRECTION ( 'NONE',  ( 1.000000000000000000, 0.000000000000000000, 0.000000000000000000 ) ) ;
#39571 = CARTESIAN_POINT ( 'NONE',  ( 5.072363130230502115, 31.00000000000000355, 77.39583333421907696 ) ) ;
#39573 = DIRECTION ( 'NONE',  ( 1.000000000000000000, 0.000000000000000000, 0.000000000000000000 ) ) ;
#39572 = DIRECTION ( 'NONE',  ( -1.000000000000000000, -0.000000000000000000, -0.000000000000000000 ) ) ;
#39574 = VERTEX_POINT ( 'NONE', #11475 ) ;
#39575 =( LENGTH_UNIT ( ) NAMED_UNIT ( * ) SI_UNIT ( .MILLI., .METRE. ) );
#39576 = EDGE_CURVE ( 'NONE', #14112, #15592, #3265, .T. ) ;
#39577 = ORIENTED_EDGE ( 'NONE', *, *, #9955, .T. ) ;
#39578 = CARTESIAN_POINT ( 'NONE',  ( 18.00000000000000355, 0.000000000000000000, 0.000000000000000000 ) ) ;
#39579 = EDGE_CURVE ( 'NONE', #14947, #7950, #41888, .T. ) ;
#39580 = CARTESIAN_POINT ( 'NONE',  ( 17.99999999999999645, 40.13512380274120517, -113.6206972269517905 ) ) ;
#39581 = CIRCLE ( 'NONE', #37510, 120.5010000000000190 ) ;
#39582 = CARTESIAN_POINT ( 'NONE',  ( 24.72345498302141920, 31.00000000000000355, -91.84610802666480822 ) ) ;
#39583 = AXIS2_PLACEMENT_3D ( 'NONE', #16794, #13291, #29879 ) ;
#39584 = CARTESIAN_POINT ( 'NONE',  ( 77.87745995356456774, 39.99999999999999289, 59.89653754212418590 ) ) ;
#39585 = ADVANCED_FACE ( 'NONE', ( #24811 ), #41975, .F. ) ;
#39586 = CARTESIAN_POINT ( 'NONE',  ( 17.99999999999999645, 48.55277268144470781, -105.3500273609075180 ) ) ;
#39587 = CIRCLE ( 'NONE', #23601, 59.00000000000001421 ) ;
#39588 = DIRECTION ( 'NONE',  ( 0.000000000000000000, 0.000000000000000000, 1.000000000000000000 ) ) ;
#39589 = ORIENTED_EDGE ( 'NONE', *, *, #24667, .F. ) ;
#39590 = CARTESIAN_POINT ( 'NONE',  ( -10.00000000000000000, 0.000000000000000000, 0.000000000000000000 ) ) ;
#39591 = ORIENTED_EDGE ( 'NONE', *, *, #28694, .F. ) ;
#39592 = DIRECTION ( 'NONE',  ( -1.000000000000000000, -0.000000000000000000, -0.000000000000000000 ) ) ;
#39593 = LINE ( 'NONE', #39370, #22790 ) ;
#39594 = LINE ( 'NONE', #23708, #17102 ) ;
#39595 = VERTEX_POINT ( 'NONE', #38066 ) ;
#39596 = CARTESIAN_POINT ( 'NONE',  ( 0.000000000000000000, 29.60891106212788415, 37.14118181634774629 ) ) ;
#39597 = CARTESIAN_POINT ( 'NONE',  ( -15.99999999999997691, 40.00000000000000000, 5.571627607371296764E-15 ) ) ;
#39598 = CARTESIAN_POINT ( 'NONE',  ( 4.211399257449709665, -2.459727064652517114, -3.751161691472417736 ) ) ;
#39600 = ORIENTED_EDGE ( 'NONE', *, *, #18035, .T. ) ;
#39599 = FACE_OUTER_BOUND ( 'NONE', #31084, .T. ) ;
#39601 = EDGE_CURVE ( 'NONE', #39427, #10641, #1194, .T. ) ;
#39602 = CARTESIAN_POINT ( 'NONE',  ( -10.89792128226954127, 31.00000000000000355, -32.25956908330170592 ) ) ;
#39603 = ADVANCED_FACE ( 'NONE', ( #1624 ), #24587, .T. ) ;
#39604 = LINE ( 'NONE', #42449, #35710 ) ;
#39605 = EDGE_CURVE ( 'NONE', #24835, #38278, #34923, .T. ) ;
#39606 = ADVANCED_FACE ( 'NONE', ( #5974 ), #12981, .F. ) ;
#39608 = VERTEX_POINT ( 'NONE', #22821 ) ;
#39607 = DIRECTION ( 'NONE',  ( 0.000000000000000000, 0.000000000000000000, 1.000000000000000000 ) ) ;
#39609 = EDGE_LOOP ( 'NONE', ( #36373, #17567, #23754, #14771 ) ) ;
#39610 = CYLINDRICAL_SURFACE ( 'NONE', #30333, 31.49899999999999878 ) ;
#39611 = CARTESIAN_POINT ( 'NONE',  ( 8.999999999999998224, 0.000000000000000000, 0.000000000000000000 ) ) ;
#39612 = CARTESIAN_POINT ( 'NONE',  ( -13.02511903071888533, 40.00000000000000000, 48.29538318457647961 ) ) ;
#39613 = CARTESIAN_POINT ( 'NONE',  ( 0.000000000000000000, 29.09613215194512748, -21.19941258140292106 ) ) ;
#39614 = CIRCLE ( 'NONE', #8305, 58.99999999999999289 ) ;
#39615 = DIRECTION ( 'NONE',  ( 1.000000000000000000, 0.000000000000000000, 0.000000000000000000 ) ) ;
#39616 = CARTESIAN_POINT ( 'NONE',  ( -4.121423858225412573, -12.61643262889541184, -1.199999999999999956 ) ) ;
#39617 = ORIENTED_EDGE ( 'NONE', *, *, #5473, .T. ) ;
#39618 = VECTOR ( 'NONE', #5100, 1000.000000000000000 ) ;
#39619 = FACE_OUTER_BOUND ( 'NONE', #7026, .T. ) ;
#39620 = ORIENTED_EDGE ( 'NONE', *, *, #12156, .F. ) ;
#39621 = FACE_BOUND ( 'NONE', #9486, .T. ) ;
#39622 = CARTESIAN_POINT ( 'NONE',  ( -4.101948962585905356, -2.368261337751088824, -3.681124513963624167 ) ) ;
#39623 = CARTESIAN_POINT ( 'NONE',  ( -44.11856065373272173, 31.00000000000000355, -25.46949057303769948 ) ) ;
#39624 = CARTESIAN_POINT ( 'NONE',  ( -10.00000000000000000, 0.000000000000000000, 0.000000000000000000 ) ) ;
#39625 = ORIENTED_EDGE ( 'NONE', *, *, #3936, .T. ) ;
#39626 = CARTESIAN_POINT ( 'NONE',  ( -9.000000000000005329, 0.000000000000000000, 11.08000000000000007 ) ) ;
#39627 = EDGE_CURVE ( 'NONE', #26154, #19383, #23129, .T. ) ;
#39628 = CARTESIAN_POINT ( 'NONE',  ( -90.10416666596678681, 31.00000000000000711, -5.890486217120279200 ) ) ;
#39629 = ADVANCED_FACE ( 'NONE', ( #12759 ), #22602, .T. ) ;
#39630 = DIRECTION ( 'NONE',  ( 0.000000000000000000, -0.5528000653611835347, -0.8333139190825215037 ) ) ;
#39631 = VERTEX_POINT ( 'NONE', #25869 ) ;
#39632 = CARTESIAN_POINT ( 'NONE',  ( -8.314562429035724733, 31.00000000000000355, -63.88718494334916187 ) ) ;
#39633 = CARTESIAN_POINT ( 'NONE',  ( 66.75914267698914273, 39.99999999999999289, 8.899205196614580871 ) ) ;
#39634 = DIRECTION ( 'NONE',  ( 1.000000000000000000, 0.000000000000000000, 0.000000000000000000 ) ) ;
#39635 = ORIENTED_EDGE ( 'NONE', *, *, #28549, .T. ) ;
#39636 = DIRECTION ( 'NONE',  ( 0.000000000000000000, 0.000000000000000000, 1.000000000000000000 ) ) ;
#39637 = DIRECTION ( 'NONE',  ( 0.000000000000000000, 0.000000000000000000, 1.000000000000000000 ) ) ;
#39638 = DIRECTION ( 'NONE',  ( -1.000000000000000000, 0.000000000000000000, -0.000000000000000000 ) ) ;
#39639 = AXIS2_PLACEMENT_3D ( 'NONE', #41765, #8184, #7745 ) ;
#39640 = CIRCLE ( 'NONE', #34808, 59.00000000000000000 ) ;
#39642 = ORIENTED_EDGE ( 'NONE', *, *, #19396, .F. ) ;
#39641 = DIRECTION ( 'NONE',  ( 1.000000000000000000, -0.000000000000000000, -0.000000000000000000 ) ) ;
#39643 = DIRECTION ( 'NONE',  ( 0.000000000000000000, 0.000000000000000000, -1.000000000000000000 ) ) ;
#39644 = VERTEX_POINT ( 'NONE', #23033 ) ;
#39645 = DIRECTION ( 'NONE',  ( 1.000000000000000000, -1.373900992973642263E-15, -3.996523416598957436E-16 ) ) ;
#39646 = AXIS2_PLACEMENT_3D ( 'NONE', #27784, #27333, #34082 ) ;
#39647 = CARTESIAN_POINT ( 'NONE',  ( -71.24862878704732339, 40.00000000000000711, 35.13526414049667324 ) ) ;
#39648 = CARTESIAN_POINT ( 'NONE',  ( 9.000000000000001776, -39.64889472655706015, -33.64468972902550092 ) ) ;
#39649 = ORIENTED_EDGE ( 'NONE', *, *, #14600, .T. ) ;
#39650 = EDGE_CURVE ( 'NONE', #25132, #1568, #29343, .T. ) ;
#39651 = DIRECTION ( 'NONE',  ( 0.000000000000000000, 0.000000000000000000, 1.000000000000000000 ) ) ;
#39652 = EDGE_CURVE ( 'NONE', #27819, #33813, #31448, .T. ) ;
#39653 = DIRECTION ( 'NONE',  ( -1.000000000000000000, -0.000000000000000000, -0.000000000000000000 ) ) ;
#39654 = EDGE_CURVE ( 'NONE', #36637, #18411, #3527, .T. ) ;
#39655 = EDGE_CURVE ( 'NONE', #19094, #41276, #29364, .T. ) ;
#39656 = EDGE_LOOP ( 'NONE', ( #28859, #40951, #42947, #18851 ) ) ;
#39657 = EDGE_CURVE ( 'NONE', #22441, #27845, #3100, .T. ) ;
#39658 = ORIENTED_EDGE ( 'NONE', *, *, #6347, .F. ) ;
#39659 = CARTESIAN_POINT ( 'NONE',  ( -19.99999999999999645, 40.00000000000000000, 0.000000000000000000 ) ) ;
#39660 = ORIENTED_EDGE ( 'NONE', *, *, #39760, .F. ) ;
#39661 = DIRECTION ( 'NONE',  ( 1.000000000000000000, 0.000000000000000000, 0.000000000000000000 ) ) ;
#39662 = CYLINDRICAL_SURFACE ( 'NONE', #19319, 31.49899999999999878 ) ;
#39663 = DIRECTION ( 'NONE',  ( -1.000000000000000000, 0.000000000000000000, 0.000000000000000000 ) ) ;
#39664 = EDGE_CURVE ( 'NONE', #32792, #22071, #19632, .T. ) ;
#39665 = CARTESIAN_POINT ( 'NONE',  ( 4.000000000000000000, -2.309401076758514915, -3.433295621305383349 ) ) ;
#39666 = ORIENTED_EDGE ( 'NONE', *, *, #13058, .F. ) ;
#39667 = CYLINDRICAL_SURFACE ( 'NONE', #14029, 59.00000000000000000 ) ;
#39668 = VERTEX_POINT ( 'NONE', #5758 ) ;
#39669 = CIRCLE ( 'NONE', #40382, 59.00000000000000000 ) ;
#39670 = FACE_OUTER_BOUND ( 'NONE', #19936, .T. ) ;
#39672 = CARTESIAN_POINT ( 'NONE',  ( -19.47536345555549886, 31.00000000000000355, -6.605835105517199324 ) ) ;
#39671 = AXIS2_PLACEMENT_3D ( 'NONE', #18422, #27795, #14700 ) ;
#39673 = ORIENTED_EDGE ( 'NONE', *, *, #30528, .T. ) ;
#39674 = DIRECTION ( 'NONE',  ( 0.000000000000000000, 0.000000000000000000, -1.000000000000000000 ) ) ;
#39675 = DIRECTION ( 'NONE',  ( 0.000000000000000000, -0.2631025642275088838, -0.9647678688145193693 ) ) ;
#39676 = CARTESIAN_POINT ( 'NONE',  ( 4.154306624731035846, -2.398490048085128556, -3.721999068284417955 ) ) ;
#39677 = CARTESIAN_POINT ( 'NONE',  ( -46.87443272357899815, 31.00000000000000355, 35.96965017775951878 ) ) ;
#39678 = VERTEX_POINT ( 'NONE', #39557 ) ;
#39679 = CARTESIAN_POINT ( 'NONE',  ( -23.27229071023271700, 31.00000000000000355, 20.35677778009614869 ) ) ;
#39680 = CARTESIAN_POINT ( 'NONE',  ( 32.44529481510334534, 40.00000000000000000, -65.82339768528792945 ) ) ;
#39681 = CARTESIAN_POINT ( 'NONE',  ( 17.99999999999999645, 0.000000000000000000, 0.000000000000000000 ) ) ;
#39682 = DIRECTION ( 'NONE',  ( -1.000000000000000000, 0.000000000000000000, 0.000000000000000000 ) ) ;
#39683 = DIRECTION ( 'NONE',  ( -1.000000000000000000, -0.000000000000000000, -0.000000000000000000 ) ) ;
#39684 = ORIENTED_EDGE ( 'NONE', *, *, #14881, .F. ) ;
#39685 = CARTESIAN_POINT ( 'NONE',  ( 20.73284993368543638, 40.00000000000000000, 42.03655757353646294 ) ) ;
#39686 = CARTESIAN_POINT ( 'NONE',  ( 9.000000000000001776, -115.6826031496111398, -8.575274253898639287 ) ) ;
#39687 = DIRECTION ( 'NONE',  ( -1.000000000000000000, 0.000000000000000000, 0.000000000000000000 ) ) ;
#39688 = AXIS2_PLACEMENT_3D ( 'NONE', #30272, #4275, #14350 ) ;
#39689 = ORIENTED_EDGE ( 'NONE', *, *, #42791, .T. ) ;
#39690 = AXIS2_PLACEMENT_3D ( 'NONE', #6984, #20341, #33824 ) ;
#39691 = CARTESIAN_POINT ( 'NONE',  ( 0.000000000000000000, -46.83041522348565167, 101.9567785075599744 ) ) ;
#39692 = DIRECTION ( 'NONE',  ( 0.000000000000000000, -0.1253332335642904638, -0.9921147013144796523 ) ) ;
#39693 = ADVANCED_FACE ( 'NONE', ( #36283 ), #6401, .T. ) ;
#39694 = EDGE_CURVE ( 'NONE', #33164, #13228, #28655, .T. ) ;
#39695 = VECTOR ( 'NONE', #36636, 1000.000000000000000 ) ;
#39696 = ORIENTED_EDGE ( 'NONE', *, *, #28772, .F. ) ;
#39697 = CARTESIAN_POINT ( 'NONE',  ( 17.99999999999999645, 0.000000000000000000, 0.000000000000000000 ) ) ;
#39698 = ORIENTED_EDGE ( 'NONE', *, *, #24716, .F. ) ;
#39699 = EDGE_CURVE ( 'NONE', #39242, #6807, #39752, .T. ) ;
#39700 = EDGE_LOOP ( 'NONE', ( #42512, #8050, #6422, #18647 ) ) ;
#39701 = DIRECTION ( 'NONE',  ( 1.000000000000000000, 0.000000000000000000, 0.000000000000000000 ) ) ;
#39702 = CARTESIAN_POINT ( 'NONE',  ( -89.42636861580037078, 31.00000000000000711, -24.07434901466544730 ) ) ;
#39703 = VERTEX_POINT ( 'NONE', #39764 ) ;
#39704 = CARTESIAN_POINT ( 'NONE',  ( 9.000000000000001776, 51.19683565102444334, 9.104066087303641197 ) ) ;
#39705 = CARTESIAN_POINT ( 'NONE',  ( 22.90854556226710415, -34.05525454449573175, -74.83297477053821467 ) ) ;
#39706 = CARTESIAN_POINT ( 'NONE',  ( 17.99999999999999645, -94.83915810436360516, -59.94836581341685644 ) ) ;
#39707 = ORIENTED_EDGE ( 'NONE', *, *, #24388, .T. ) ;
#39708 = ADVANCED_FACE ( 'NONE', ( #35441 ), #2681, .T. ) ;
#39709 = CARTESIAN_POINT ( 'NONE',  ( 18.00000000000000355, 30.03615769709733740, 42.44795908868999135 ) ) ;
#39710 = CARTESIAN_POINT ( 'NONE',  ( 0.000000000000000000, -11.58753559615507100, 29.77419532459258278 ) ) ;
#39711 = ADVANCED_FACE ( 'NONE', ( #19115, #32172, #28915, #12340, #38922, #9039, #15827, #27148, #40618, #34102 ), #14061, .F. ) ;
#39712 = CIRCLE ( 'NONE', #28620, 58.99999999999998579 ) ;
#39714 = DIRECTION ( 'NONE',  ( 0.000000000000000000, 0.000000000000000000, 1.000000000000000000 ) ) ;
#39713 = DIRECTION ( 'NONE',  ( 0.000000000000000000, 0.000000000000000000, 1.000000000000000000 ) ) ;
#39715 = CIRCLE ( 'NONE', #27944, 116.0000000000000000 ) ;
#39716 = DIRECTION ( 'NONE',  ( -1.000000000000000000, 0.000000000000000000, 0.000000000000000000 ) ) ;
#39717 = ORIENTED_EDGE ( 'NONE', *, *, #39192, .T. ) ;
#39718 = PRESENTATION_STYLE_ASSIGNMENT (( #16424 ) ) ;
#39719 = CARTESIAN_POINT ( 'NONE',  ( 8.699408683037360035, 31.00000000000000355, 25.59862650653646909 ) ) ;
#39720 = AXIS2_PLACEMENT_3D ( 'NONE', #6242, #12594, #33296 ) ;
#39721 = VERTEX_POINT ( 'NONE', #40411 ) ;
#39722 = DIRECTION ( 'NONE',  ( -1.000000000000000000, -0.000000000000000000, -0.000000000000000000 ) ) ;
#39723 = AXIS2_PLACEMENT_3D ( 'NONE', #23720, #36982, #40461 ) ;
#39724 = AXIS2_PLACEMENT_3D ( 'NONE', #21212, #34254, #4349 ) ;
#39725 = CARTESIAN_POINT ( 'NONE',  ( 0.000000000000000000, 111.8797445107944810, -8.437727291343108504 ) ) ;
#39726 = ORIENTED_EDGE ( 'NONE', *, *, #39207, .F. ) ;
#39727 = AXIS2_PLACEMENT_3D ( 'NONE', #625, #10686, #30123 ) ;
#39728 = LINE ( 'NONE', #13163, #7611 ) ;
#39729 = CARTESIAN_POINT ( 'NONE',  ( 35.10416666475790493, 40.00000000000000000, 2.290744634698880233 ) ) ;
#39730 = CARTESIAN_POINT ( 'NONE',  ( 31.88898475262399401, 40.00000000000000000, 36.48290236124523744 ) ) ;
#39731 = VERTEX_POINT ( 'NONE', #40846 ) ;
#39732 = VERTEX_POINT ( 'NONE', #6611 ) ;
#39733 = DIRECTION ( 'NONE',  ( 1.000000000000000000, 0.000000000000000000, 0.000000000000000000 ) ) ;
#39734 = DIRECTION ( 'NONE',  ( 0.000000000000000000, 0.000000000000000000, 1.000000000000000000 ) ) ;
#39735 = DIRECTION ( 'NONE',  ( 1.000000000000000000, 0.000000000000000000, 0.000000000000000000 ) ) ;
#39736 = FACE_OUTER_BOUND ( 'NONE', #36795, .T. ) ;
#39737 = EDGE_LOOP ( 'NONE', ( #11738, #1351 ) ) ;
#39738 = DIRECTION ( 'NONE',  ( 0.000000000000000000, 0.9980267284282716700, -0.06279051952930995995 ) ) ;
#39739 = VERTEX_POINT ( 'NONE', #16701 ) ;
#39740 = CARTESIAN_POINT ( 'NONE',  ( -30.61154013076160751, 40.00000000000002842, 25.77968906985393716 ) ) ;
#39741 = DIRECTION ( 'NONE',  ( 1.000000000000000000, 0.000000000000000000, 0.000000000000000000 ) ) ;
#39742 = VECTOR ( 'NONE', #20966, 1000.000000000000000 ) ;
#39743 = ORIENTED_EDGE ( 'NONE', *, *, #17284, .T. ) ;
#39744 = DIRECTION ( 'NONE',  ( -1.000000000000000000, -0.000000000000000000, -0.000000000000000000 ) ) ;
#39745 = ADVANCED_FACE ( 'NONE', ( #488 ), #10548, .T. ) ;
#39746 = CARTESIAN_POINT ( 'NONE',  ( 0.000000000000000000, -64.58410930313591791, 101.7319213743680422 ) ) ;
#39747 = ORIENTED_EDGE ( 'NONE', *, *, #20661, .F. ) ;
#39748 = CYLINDRICAL_SURFACE ( 'NONE', #38886, 13.59999999999999964 ) ;
#39749 = EDGE_LOOP ( 'NONE', ( #1755, #31797, #5781, #24921 ) ) ;
#39750 = CIRCLE ( 'NONE', #21015, 47.49900000000000233 ) ;
#39751 = DIRECTION ( 'NONE',  ( -1.000000000000000000, -0.000000000000000000, 0.000000000000000000 ) ) ;
#39752 = CIRCLE ( 'NONE', #21021, 13.59999999999999964 ) ;
#39753 = VERTEX_POINT ( 'NONE', #13627 ) ;
#39755 = ORIENTED_EDGE ( 'NONE', *, *, #15315, .F. ) ;
#39754 = CARTESIAN_POINT ( 'NONE',  ( 0.000000000000000000, 0.000000000000000000, 0.000000000000000000 ) ) ;
#39756 = CIRCLE ( 'NONE', #14020, 15.00000000000000000 ) ;
#39757 = CARTESIAN_POINT ( 'NONE',  ( 30.38134496340387969, 31.00000000000000355, 61.85720693093856681 ) ) ;
#39758 = ORIENTED_EDGE ( 'NONE', *, *, #12258, .T. ) ;
#39759 = LINE ( 'NONE', #26487, #9810 ) ;
#39760 = EDGE_CURVE ( 'NONE', #42037, #38673, #24101, .T. ) ;
#39761 = AXIS2_PLACEMENT_3D ( 'NONE', #8646, #28327, #41594 ) ;
#39762 = VERTEX_POINT ( 'NONE', #20400 ) ;
#39763 = EDGE_CURVE ( 'NONE', #35448, #28827, #31479, .T. ) ;
#39764 = CARTESIAN_POINT ( 'NONE',  ( 17.99999999999999645, 75.03166794516801019, 94.29071961951534320 ) ) ;
#39765 = ORIENTED_EDGE ( 'NONE', *, *, #11710, .T. ) ;
#39766 = CARTESIAN_POINT ( 'NONE',  ( 42.86165537668587433, 40.00000000000000000, -73.99543480067944756 ) ) ;
#39767 = VECTOR ( 'NONE', #42185, 1000.000000000000000 ) ;
#39768 = EDGE_CURVE ( 'NONE', #38321, #2759, #12670, .T. ) ;
#39770 = CARTESIAN_POINT ( 'NONE',  ( 17.99999999999999645, 68.61497464550593861, 99.05794392877625398 ) ) ;
#39769 = CARTESIAN_POINT ( 'NONE',  ( -6.004904395537136175, 2.351321854362917684E-15, -19.19999999999999574 ) ) ;
#39771 = CIRCLE ( 'NONE', #16851, 20.00000000000000355 ) ;
#39772 = DIRECTION ( 'NONE',  ( -1.000000000000000000, -0.000000000000000000, 0.000000000000000000 ) ) ;
#39773 = ORIENTED_EDGE ( 'NONE', *, *, #23667, .F. ) ;
#39774 = CARTESIAN_POINT ( 'NONE',  ( 0.000000000000000000, 0.000000000000000000, 0.000000000000000000 ) ) ;
#39775 = ORIENTED_EDGE ( 'NONE', *, *, #21333, .F. ) ;
#39776 = PRODUCT_CONTEXT ( 'NONE', #33406, 'mechanical' ) ;
#39777 = CARTESIAN_POINT ( 'NONE',  ( 2.649999999999993694, -150.5000000000000284, 6.999999999999998224 ) ) ;
#39778 = CARTESIAN_POINT ( 'NONE',  ( 74.72486387243833406, 31.00000000000000000, 9.837939412698395003 ) ) ;
#39780 = CARTESIAN_POINT ( 'NONE',  ( -19.99999999999999645, 40.00000000000000000, 0.000000000000000000 ) ) ;
#39779 = DIRECTION ( 'NONE',  ( -1.000000000000000000, -0.000000000000000000, 0.000000000000000000 ) ) ;
#39781 = ORIENTED_EDGE ( 'NONE', *, *, #22685, .F. ) ;
#39782 = EDGE_CURVE ( 'NONE', #14255, #9587, #4194, .T. ) ;
#39783 = PLANE ( 'NONE',  #10108 ) ;
#39785 = EDGE_CURVE ( 'NONE', #30670, #35008, #3976, .T. ) ;
#39784 = CIRCLE ( 'NONE', #9161, 116.0000000000000000 ) ;
#39786 = ORIENTED_EDGE ( 'NONE', *, *, #28964, .F. ) ;
#39787 = DIRECTION ( 'NONE',  ( 0.000000000000000000, -0.8183027759081743513, 0.5747874102143992747 ) ) ;
#39788 = EDGE_CURVE ( 'NONE', #9587, #31709, #23834, .T. ) ;
#39789 = CARTESIAN_POINT ( 'NONE',  ( 0.000000000000000000, 91.65951123222582453, -71.09524597797991419 ) ) ;
#39790 = DIRECTION ( 'NONE',  ( -0.000000000000000000, -0.000000000000000000, 1.000000000000000000 ) ) ;
#39791 = CIRCLE ( 'NONE', #21062, 120.5010000000000332 ) ;
#39792 = CARTESIAN_POINT ( 'NONE',  ( 17.99999999999999645, 0.000000000000000000, 0.000000000000000000 ) ) ;
#39793 = CARTESIAN_POINT ( 'NONE',  ( 32.30287614962725229, -35.35525454449572180, 69.29271901957299917 ) ) ;
#39794 = ORIENTED_EDGE ( 'NONE', *, *, #43104, .T. ) ;
#39795 = CARTESIAN_POINT ( 'NONE',  ( -31.75000000000000000, 18.77999999999999048, 0.000000000000000000 ) ) ;
#39796 = ORIENTED_EDGE ( 'NONE', *, *, #35311, .F. ) ;
#39797 = CIRCLE ( 'NONE', #6360, 24.99999999999998934 ) ;
#39798 = DIRECTION ( 'NONE',  ( 1.000000000000000000, 1.836909530733573776E-16, 0.000000000000000000 ) ) ;
#39799 = CARTESIAN_POINT ( 'NONE',  ( 17.99999999999999645, 46.12538073176499154, -111.3235835452206857 ) ) ;
#39800 = CARTESIAN_POINT ( 'NONE',  ( 17.99999999999999645, 0.000000000000000000, 0.000000000000000000 ) ) ;
#39801 = VERTEX_POINT ( 'NONE', #20851 ) ;
#39802 = DIRECTION ( 'NONE',  ( -1.000000000000000000, -0.000000000000000000, -0.000000000000000000 ) ) ;
#39803 = EDGE_CURVE ( 'NONE', #6408, #23271, #2868, .T. ) ;
#39804 = CARTESIAN_POINT ( 'NONE',  ( 18.00000000000000355, 0.000000000000000000, 0.000000000000000000 ) ) ;
#39805 = DIRECTION ( 'NONE',  ( -1.000000000000000000, -0.000000000000000000, -0.000000000000000000 ) ) ;
#39807 = ORIENTED_EDGE ( 'NONE', *, *, #34347, .F. ) ;
#39806 = LINE ( 'NONE', #34142, #17404 ) ;
#39808 = CARTESIAN_POINT ( 'NONE',  ( -24.93870012978733541, 31.00000000000000355, -21.94074674037795702 ) ) ;
#39809 = FACE_OUTER_BOUND ( 'NONE', #32361, .T. ) ;
#39810 = EDGE_CURVE ( 'NONE', #21330, #31605, #42591, .T. ) ;
#39812 = VERTEX_POINT ( 'NONE', #36717 ) ;
#39811 = CARTESIAN_POINT ( 'NONE',  ( 18.00000000000000355, 46.19362259308845609, -8.585149169757988474 ) ) ;
#39813 = ORIENTED_EDGE ( 'NONE', *, *, #21172, .T. ) ;
#39814 = FACE_OUTER_BOUND ( 'NONE', #20997, .T. ) ;
#39815 = CARTESIAN_POINT ( 'NONE',  ( 0.000000000000000000, 25.46650492921924425, -19.29328419707757547 ) ) ;
#39816 = CARTESIAN_POINT ( 'NONE',  ( 42.13926417418816328, 40.00000000000000000, -36.83769365845790134 ) ) ;
#39817 = DIRECTION ( 'NONE',  ( 0.000000000000000000, 0.7980172272802408262, -0.6026346363792547400 ) ) ;
#39818 =( REPRESENTATION_RELATIONSHIP ('NONE','NONE', #330, #19391 ) REPRESENTATION_RELATIONSHIP_WITH_TRANSFORMATION ( #29676 )SHAPE_REPRESENTATION_RELATIONSHIP( ) );
#39819 = CIRCLE ( 'NONE', #9164, 20.00000000000000355 ) ;
#39820 = LINE ( 'NONE', #2528, #14516 ) ;
#39821 = AXIS2_PLACEMENT_3D ( 'NONE', #30774, #37299, #3900 ) ;
#39822 = EDGE_CURVE ( 'NONE', #36818, #14078, #10570, .T. ) ;
#39823 = CARTESIAN_POINT ( 'NONE',  ( 18.00000000000000355, 22.43957647427220081, -41.27978878573604504 ) ) ;
#39824 = VERTEX_POINT ( 'NONE', #27573 ) ;
#39825 = LINE ( 'NONE', #7315, #27239 ) ;
#39826 = EDGE_LOOP ( 'NONE', ( #2248, #22281, #15452, #30167, #22739, #13585, #195 ) ) ;
#39827 = AXIS2_PLACEMENT_3D ( 'NONE', #16917, #30419, #27359 ) ;
#39828 = DIRECTION ( 'NONE',  ( 0.000000000000000000, 0.9407002666710320149, 0.3392388661180340548 ) ) ;
#39829 = CARTESIAN_POINT ( 'NONE',  ( 0.000000000000000000, -150.5000000000000284, 6.999999999999998224 ) ) ;
#39830 = CARTESIAN_POINT ( 'NONE',  ( 44.91824650936478491, 31.00000000000000355, 5.910997147197376123 ) ) ;
#39831 = LINE ( 'NONE', #23526, #25348 ) ;
#39832 = ORIENTED_EDGE ( 'NONE', *, *, #29118, .T. ) ;
#39833 = B_SPLINE_SURFACE_WITH_KNOTS ( 'NONE', 1, 3, ( 
 ( #3353, #16721, #34121, #40865, #21080, #4658, #11019, #28250, #34331, #934, #37601, #21730, #41076, #11442, #25210, #1594, #14946, #41516, #7504, #4425, #4214, #31296, #14513, #24347, #11664, #11228, #14729, #17799, #41738, #28474, #34771, #1381, #34979, #27820, #18449, #5088, #14284, #20867, #11882, #38251, #31072, #27592, #28033, #41295, #18242, #31716, #15170, #7716, #17583, #25008, #8367, #24777, #38031, #1160, #8159, #1812, #24560, #37812, #30856, #21523, #7931, #4881, #31506, #21295, #34546, #18034, #25833, #36037, #39295, #32563, #12726, #42375, #8795, #16217, #12304, #15793, #19505, #9430, #35607, #29099, #25629, #12519, #38454, #41943, #35188, #38671, #29514, #28881, #16010, #5726, #22153, #2650, #39095, #9215, #26030, #21933, #22566, #2223, #2430, #5934, #29309, #5311, #38893, #35808, #19292, #42577, #6161, #42782, #25412, #12093, #42147, #22783, #35411, #12943, #5526, #18680, #32774, #2857, #9009, #15581, #8573, #2019, #28677, #31942, #18883, #32345, #32142, #22360, #15383, #19083, #7015, #6802, #17091, #23002, #458, #40381, #10073, #13379, #33630, #29955, #30602, #10301, #23645, #16434, #32981, #27117, #10517, #36903, #26892, #3062, #3507, #36246, #13819, #26671, #33852, #667, #23852, #19939, #20163, #13594, #6573, #39940, #19717, #20367, #29738, #221, #16884, #30166, #16670, #39730, #40162, #37117, #9657, #23418, #13165, #7225, #20581, #3940, #6369, #17325, #30380, #3712, #26248, #39519, #33208, #43010, #26458, #9857, #33422, #9, #36679, #23209, #36458, #3291, #14462, #17977, #31663, #1109, #14236, #31248, #24514, #7665, #10966, #1333, #24953, #21031, #11178, #14676, #27988, #20815, #14893, #34282, #21676, #38203, #27772, #28192, #34074, #37336, #4374, #41246, #37763, #11389, #30807, #883, #24298, #34720, #41029, #37978, #27540, #11612, #7882, #31458, #34932, #21240, #17748, #41462, #40814, #8319, #21469, #5041, #4833, #34493, #18401, #40590, #4158, #37556, #4604, #17533, #18190, #31019, #7450, #24723, #14028, #8104, #1545, #27323, #10728, #24068, #9760, #20058, #42481, #28419, #26143, #9322, #5838, #36360, #6059, #9555, #29210, #36574, #23315, #29631, #39417, #29865, #22679, #13277, #43126, #9117, #1759, #6698, #33096, #12626, #22470, #22910, #36149, #13066, #16559, #9966, #35711, #41693, #39633, #23114, #6269, #19616, #19194, #32883, #26571, #39199, #32677, #25741, #2962, #39843, #16325, #42905, #26368, #6472, #15118, #19830, #12423, #3183, #38995, #32462, #2550, #15916, #25938, #2757, #35931, #19411, #16119, #29419, #42685, #12834, #10186, #27430, #40050, #40489, #14136, #23535, #7340, #10627, #37226, #23746, #3616, #20701, #20923, #16779, #30495, #20268, #14349, #27659, #34177, #120, #11079, #37448, #33966, #782, #996, #27009, #40926, #7565, #4274, #13923, #37017, #7123, #40699, #24405, #574, #33740, #4054, #7779, #20478, #17645, #17429, #16986, #37658, #3828, #23959, #33325, #30909, #27220, #30707, #17210, #10852, #3408, #36803, #30067, #33531, #13488, #24183, #26778, #6906, #30271, #341, #13705, #40281, #10411, #4485, #41581, #28088, #28315, #31784, #15236, #31137, #21581, #8427, #21790, #25068, #31995, #12149, #7990, #24617, #24841, #5373, #37869, #25470, #21355, #1226, #15441, #28531, #34827, #41351, #41796, #27878, #11284, #38307, #34607, #15005, #4722, #18090, #35247, #1652, #1873, #11731, #11942, #17863, #38512, #18737, #4940, #8222, #25264, #38094, #38732, #5145, #18507, #31351, #41135, #21988, #2074, #8632, #35037, #1436, #28735, #14575, #41998, #18298, #21137, #34385, #14788, #11501, #31559, #2705, #35667, #42430, #32200, #22417, #9498, #29162, #26094, #12369, #29577, #25894, #6220, #13011, #12575, #5785, #2916, #25690, #42847, #39358, #26314, #22853, #9274, #32833, #35465, #28941, #38947, #39152, #42211, #36101, #9065, #2277, #19141, #16276, #32408, #19357, #23060, #19562, #39584, #9714, #8858, #2494, #5581, #22630, #15859, #35873, #22214, #6005, #16066, #32628, #18941, #15637, #29371, #42634, #12784, #24990, #15566, #32126, #11427, #4640, #8997, #35394, #1579, #24761, #28454 ),
 ( #22341, #34965, #22135, #8558, #18226, #25613, #21712, #25193, #28863, #18865, #1797, #38440, #5073, #21917, #18016, #8142, #1365, #4863, #38871, #38236, #25395, #15155, #31493, #12077, #35168, #5291, #5511, #31282, #18665, #11649, #11866, #15363, #41928, #14714, #18434, #31922, #2006, #28658, #42129, #28019, #34757, #21504, #8351, #2208, #14928, #41278, #28233, #38014, #12287, #38652, #31697, #41725, #8776, #41498, #9605, #32722, #36198, #39679, #13116, #2600, #39891, #2803, #3457, #20112, #39467, #10018, #15964, #19240, #29468, #42955, #6316, #9806, #12675, #25984, #6108, #16617, #26191, #19882, #39243, #36625, #22956, #13327, #16831, #19666, #16167, #23363, #9371, #33371, #3238, #6749, #29910, #32932, #30115, #22521, #29260, #22727, #3010, #42524, #43173, #35983, #32512, #19458, #171, #42729, #26414, #13538, #33151, #26619, #39041, #9166, #12885, #35753, #16377, #29682, #23160, #5884, #36409, #6520, #10463, #17918, #4540, #10906, #20758, #11127, #3882, #37707, #24454, #33580, #26832, #31193, #14401, #23797, #3663, #7393, #34018, #37503, #40978, #34437, #17036, #23589, #20972, #34227, #4106, #30754, #30324, #17477, #7827, #20528, #13971, #6959, #832, #21185, #14182, #24241, #27481, #17692, #1280, #40755, #40104, #27714, #4321, #10242, #7612, #30961, #36855, #27268, #20316, #1049, #40538, #396, #13760, #27062, #40330, #37067, #7172, #33793, #17268, #30549, #37277, #617, #10676, #24014, #8475, #28785, #8272, #1702, #37922, #21837, #25526, #1923, #41845, #35085, #5426, #32248, #15286, #12202, #15489, #8685, #35513, #28577, #22045, #42046, #15060, #14625, #5198, #28366, #8043, #18563, #21410, #34665, #35302, #4781, #31836, #14838, #11995, #25113, #21628, #11553, #5629, #41637, #34876, #11784, #25314, #38560, #18140, #38782, #4991, #22265, #8915, #38359, #18991, #31403, #1488, #18347, #18788, #32043, #2126, #28135, #41405, #24896, #27932, #41187, #11335, #38150, #24666, #31606, #19829, #9965, #32675, #9321, #29864, #32461, #26570, #9759, #13276, #23113, #26142, #3182, #28997, #35709, #15914, #42683, #5837, #36359, #29209, #38994, #2549, #16558, #35930, #6267, #20057, #39632, #6471, #33095, #2327, #42480, #42265, #39416, #22678, #19193, #43125, #6058, #9554, #12625, #36572, #23314, #29630, #22909, #39842, #19410, #6697, #15693, #9116, #12422, #25740, #22469, #25937, #39197, #36148, #19615, #13065, #2756, #16118, #29418, #12833, #32882, #2961, #16324, #42904, #26367, #40048, #34176, #4273, #17428, #33965, #10185, #10626, #119, #7564, #33739, #40925, #7778, #17644, #27008, #13922, #20700, #13704, #3826, #26777, #14135, #23534, #7338, #23958, #37225, #23745, #3615, #4053, #20922, #16778, #30494, #20267, #14347, #27658, #30908, #13487, #11078, #37447, #30706, #781, #995, #40280, #24404, #37657, #33324, #27219, #37016, #7122, #40698, #3407, #573, #17209, #27429, #30066, #20477, #36802, #10850, #16985, #6905, #40488, #24182, #33530, #30270, #340, #10410, #8221, #11730, #21136, #24616, #17861, #21354, #41997, #11500, #41795, #31558, #34606, #28530, #38306, #25067, #8631, #4484, #41580, #28087, #28313, #41134, #11941, #8426, #2073, #21789, #35036, #5144, #31994, #12148, #7989, #37868, #24839, #5372, #4721, #25469, #18089, #1225, #15440, #25263, #21580, #41350, #15235, #27877, #11283, #18506, #31350, #15004, #1435, #14787, #35245, #1651, #1872, #31782, #38511, #31136, #21987, #18736, #4939, #34826, #28734, #38093, #38730, #34384, #14574, #18297, #38946, #23059, #42429, #12783, #26514, #2915, #16275, #29576, #8857, #5784, #35464, #32626, #15858, #12368, #42846, #12574, #16065, #35666, #43072, #29806, #36099, #2704, #36308, #29160, #19776, #6425, #15636, #22213, #13225, #39582, #19140, #28940, #29370, #42633, #19561, #33040, #16503, #42209, #5580, #13009, #26313, #26093, #39357, #25689, #9496, #3125, #2493, #39151, #32199, #22852, #18940, #6219, #32832, #9713, #2276, #9064, #22416, #32407, #25893, #9273, #22629, #35872, #6003, #19356, #26949, #14289, #30439, #40224, #33272, #3769, #3358, #16725, #33912, #30015, #17150, #39997 ) ),
 .UNSPECIFIED., .F., .F., .F.,
 ( 2, 2 ),
 ( 4, 2, 2, 2, 2, 2, 2, 2, 2, 2, 2, 2, 2, 2, 2, 2, 2, 2, 2, 2, 2, 2, 2, 2, 2, 2, 2, 2, 2, 2, 2, 2, 2, 2, 2, 2, 2, 2, 2, 2, 2, 2, 2, 2, 2, 2, 2, 2, 2, 2, 2, 2, 2, 2, 2, 2, 2, 2, 2, 2, 2, 2, 2, 2, 2, 2, 2, 2, 2, 2, 2, 2, 2, 2, 2, 2, 2, 2, 2, 2, 2, 2, 2, 2, 2, 2, 2, 2, 2, 2, 2, 2, 2, 2, 2, 2, 2, 2, 2, 2, 2, 2, 2, 2, 2, 2, 2, 2, 2, 2, 2, 2, 2, 2, 2, 2, 2, 2, 2, 2, 2, 2, 2, 2, 2, 2, 2, 2, 2, 2, 2, 2, 2, 2, 2, 2, 2, 2, 2, 2, 2, 2, 2, 2, 2, 2, 2, 2, 2, 2, 2, 2, 2, 2, 2, 2, 2, 2, 2, 2, 2, 2, 2, 2, 2, 2, 2, 2, 2, 2, 2, 2, 2, 2, 2, 2, 2, 2, 2, 2, 2, 2, 2, 2, 2, 2, 2, 2, 2, 2, 2, 2, 2, 2, 2, 2, 2, 2, 2, 2, 2, 2, 2, 2, 2, 2, 2, 2, 2, 2, 2, 2, 2, 2, 2, 2, 2, 2, 2, 2, 2, 2, 2, 2, 2, 2, 2, 2, 2, 2, 2, 2, 2, 2, 2, 2, 2, 2, 2, 2, 2, 2, 2, 2, 2, 2, 2, 2, 2, 2, 2, 2, 2, 2, 2, 2, 4 ),
 ( 0.5000000000000002220, 0.9090909090909090606 ),
 ( 0.000000000000000000, 0.003906250000000000000, 0.007812500000000000000, 0.01171875000000000000, 0.01562500000000000000, 0.01953125000000000000, 0.02343750000000000000, 0.02734375000000000000, 0.03125000000000000000, 0.03515625000000000000, 0.03906250000000000000, 0.04296875000000000000, 0.04687500000000000000, 0.05078125000000000000, 0.05468750000000000000, 0.05859375000000000000, 0.06250000000000000000, 0.06640625000000000000, 0.07031250000000000000, 0.07421875000000000000, 0.07812500000000000000, 0.08203125000000000000, 0.08593750000000000000, 0.08984375000000000000, 0.09375000000000000000, 0.09765625000000000000, 0.1015625000000000000, 0.1054687500000000000, 0.1093750000000000000, 0.1132812500000000000, 0.1171875000000000000, 0.1210937500000000000, 0.1250000000000000000, 0.1289062500000000000, 0.1328125000000000000, 0.1367187500000000000, 0.1406250000000000000, 0.1445312500000000000, 0.1484375000000000000, 0.1523437500000000000, 0.1562500000000000000, 0.1601562500000000000, 0.1640625000000000000, 0.1679687500000000000, 0.1718750000000000000, 0.1757812500000000000, 0.1796875000000000000, 0.1835937500000000000, 0.1875000000000000000, 0.1914062500000000000, 0.1953125000000000000, 0.1992187500000000000, 0.2031250000000000000, 0.2070312500000000000, 0.2109375000000000000, 0.2148437500000000000, 0.2187500000000000000, 0.2226562500000000000, 0.2265625000000000000, 0.2304687500000000000, 0.2343750000000000000, 0.2382812500000000000, 0.2421875000000000000, 0.2460937500000000000, 0.2500000000000000000, 0.2539062500000000000, 0.2578125000000000000, 0.2617187500000000000, 0.2656250000000000000, 0.2695312500000000000, 0.2734375000000000000, 0.2773437500000000000, 0.2812500000000000000, 0.2851562500000000000, 0.2890625000000000000, 0.2929687500000000000, 0.2968750000000000000, 0.3007812500000000000, 0.3046875000000000000, 0.3085937500000000000, 0.3125000000000000000, 0.3164062500000000000, 0.3203125000000000000, 0.3242187500000000000, 0.3281250000000000000, 0.3320312500000000000, 0.3359375000000000000, 0.3398437500000000000, 0.3437500000000000000, 0.3476562500000000000, 0.3515625000000000000, 0.3554687500000000000, 0.3593750000000000000, 0.3632812500000000000, 0.3671875000000000000, 0.3710937500000000000, 0.3750000000000000000, 0.3789062500000000000, 0.3828125000000000000, 0.3867187500000000000, 0.3906250000000000000, 0.3945312500000000000, 0.3984375000000000000, 0.4023437500000000000, 0.4062500000000000000, 0.4101562500000000000, 0.4140625000000000000, 0.4179687500000000000, 0.4218750000000000000, 0.4257812500000000000, 0.4296875000000000000, 0.4335937500000000000, 0.4375000000000000000, 0.4414062500000000000, 0.4453125000000000000, 0.4492187500000000000, 0.4531250000000000000, 0.4570312500000000000, 0.4609375000000000000, 0.4648437500000000000, 0.4687500000000000000, 0.4726562500000000000, 0.4765625000000000000, 0.4804687500000000000, 0.4843750000000000000, 0.4882812500000000000, 0.4921875000000000000, 0.4960937500000000000, 0.5000000000000000000, 0.5039062500000000000, 0.5078125000000000000, 0.5117187500000000000, 0.5156250000000000000, 0.5195312500000000000, 0.5234375000000000000, 0.5273437500000000000, 0.5312500000000000000, 0.5351562500000000000, 0.5390625000000000000, 0.5429687500000000000, 0.5468750000000000000, 0.5507812500000000000, 0.5546875000000000000, 0.5585937500000000000, 0.5625000000000000000, 0.5664062500000000000, 0.5703125000000000000, 0.5742187500000000000, 0.5781250000000000000, 0.5820312500000000000, 0.5859375000000000000, 0.5898437500000000000, 0.5937500000000000000, 0.5976562500000000000, 0.6015625000000000000, 0.6054687500000000000, 0.6093750000000000000, 0.6132812500000000000, 0.6171875000000000000, 0.6210937500000000000, 0.6250000000000000000, 0.6289062500000000000, 0.6328125000000000000, 0.6367187500000000000, 0.6406250000000000000, 0.6445312500000000000, 0.6484375000000000000, 0.6523437500000000000, 0.6562500000000000000, 0.6601562500000000000, 0.6640625000000000000, 0.6679687500000000000, 0.6718750000000000000, 0.6757812500000000000, 0.6796875000000000000, 0.6835937500000000000, 0.6875000000000000000, 0.6914062500000000000, 0.6953125000000000000, 0.6992187500000000000, 0.7031250000000000000, 0.7070312500000000000, 0.7109375000000000000, 0.7148437500000000000, 0.7187500000000000000, 0.7226562500000000000, 0.7265625000000000000, 0.7304687500000000000, 0.7343750000000000000, 0.7382812500000000000, 0.7421875000000000000, 0.7460937500000000000, 0.7500000000000000000, 0.7539062500000000000, 0.7578125000000000000, 0.7617187500000000000, 0.7656250000000000000, 0.7695312500000000000, 0.7734375000000000000, 0.7773437500000000000, 0.7812500000000000000, 0.7851562500000000000, 0.7890625000000000000, 0.7929687500000000000, 0.7968750000000000000, 0.8007812500000000000, 0.8046875000000000000, 0.8085937500000000000, 0.8125000000000000000, 0.8164062500000000000, 0.8203125000000000000, 0.8242187500000000000, 0.8281250000000000000, 0.8320312500000000000, 0.8359375000000000000, 0.8398437500000000000, 0.8437500000000000000, 0.8476562500000000000, 0.8515625000000000000, 0.8554687500000000000, 0.8593750000000000000, 0.8632812500000000000, 0.8671875000000000000, 0.8710937500000000000, 0.8750000000000000000, 0.8789062500000000000, 0.8828125000000000000, 0.8867187500000000000, 0.8906250000000000000, 0.8945312500000000000, 0.8984375000000000000, 0.9023437500000000000, 0.9062500000000000000, 0.9101562500000000000, 0.9140625000000000000, 0.9179687500000000000, 0.9218750000000000000, 0.9257812500000000000, 0.9296875000000000000, 0.9335937500000000000, 0.9375000000000000000, 0.9414062500000000000, 0.9453125000000000000, 0.9492187500000000000, 0.9531250000000000000, 0.9570312500000000000, 0.9609375000000000000, 0.9648437500000000000, 0.9687500000000000000, 0.9726562500000000000, 0.9765625000000000000, 0.9804687500000000000, 0.9843750000000000000, 0.9882812500000000000, 0.9921875000000000000, 0.9960937500000000000, 1.000000000000000000 ),
 .UNSPECIFIED. ) ;
#39834 = CYLINDRICAL_SURFACE ( 'NONE', #23358, 20.00000000000000355 ) ;
#39835 = ORIENTED_EDGE ( 'NONE', *, *, #16812, .F. ) ;
#39836 = CARTESIAN_POINT ( 'NONE',  ( -94.39576909109665337, 31.00000000000000711, 32.06004391471374504 ) ) ;
#39837 = ADVANCED_FACE ( 'NONE', ( #26704 ), #16914, .T. ) ;
#39838 = ORIENTED_EDGE ( 'NONE', *, *, #18135, .T. ) ;
#39839 = ADVANCED_FACE ( 'NONE', ( #36490 ), #29988, .F. ) ;
#39840 = DIRECTION ( 'NONE',  ( 1.000000000000000000, 0.000000000000000000, 0.000000000000000000 ) ) ;
#39841 = ORIENTED_EDGE ( 'NONE', *, *, #28423, .F. ) ;
#39842 = CARTESIAN_POINT ( 'NONE',  ( 66.90003082756123831, 31.00000000000000000, -4.275635516647131595 ) ) ;
#39843 = CARTESIAN_POINT ( 'NONE',  ( 22.12550800842195287, 40.00000000000000000, 65.48657384633656875 ) ) ;
#39844 = CARTESIAN_POINT ( 'NONE',  ( 0.000000000000000000, 150.5000000000000284, 9.999999999999998224 ) ) ;
#39845 = VERTEX_POINT ( 'NONE', #10102 ) ;
#39846 = ORIENTED_EDGE ( 'NONE', *, *, #14553, .T. ) ;
#39847 = CARTESIAN_POINT ( 'NONE',  ( -3.472371940586054251, -2.614027278893156669, -3.320322319202162031 ) ) ;
#39848 = DIRECTION ( 'NONE',  ( 0.000000000000000000, 0.000000000000000000, 1.000000000000000000 ) ) ;
#39849 = DIRECTION ( 'NONE',  ( -1.000000000000000000, -0.000000000000000000, -0.000000000000000000 ) ) ;
#39850 = VECTOR ( 'NONE', #12854, 1000.000000000000000 ) ;
#39852 = ORIENTED_EDGE ( 'NONE', *, *, #12745, .F. ) ;
#39851 = FACE_OUTER_BOUND ( 'NONE', #33661, .T. ) ;
#39853 = CARTESIAN_POINT ( 'NONE',  ( 17.99999999999999645, 119.0898412705474385, 18.38751498043773935 ) ) ;
#39854 = ORIENTED_EDGE ( 'NONE', *, *, #2795, .F. ) ;
#39855 = CARTESIAN_POINT ( 'NONE',  ( 2.339412683011424576, -2.055254544495723756, -89.04250581823735899 ) ) ;
#39856 = EDGE_CURVE ( 'NONE', #4224, #22493, #6836, .T. ) ;
#39857 = CARTESIAN_POINT ( 'NONE',  ( 55.27058341129635721, 39.99999999999999289, -63.02248852588876105 ) ) ;
#39858 = CARTESIAN_POINT ( 'NONE',  ( 18.00000000000000355, 42.03146605346817921, -22.12489237027272893 ) ) ;
#39859 = VECTOR ( 'NONE', #21664, 1000.000000000000000 ) ;
#39860 = ORIENTED_EDGE ( 'NONE', *, *, #5364, .F. ) ;
#39861 = LINE ( 'NONE', #10207, #30416 ) ;
#39862 = CARTESIAN_POINT ( 'NONE',  ( 8.999999999999998224, 74.56001736500617483, 88.86396238369059120 ) ) ;
#39863 = ORIENTED_EDGE ( 'NONE', *, *, #8240, .T. ) ;
#39864 = EDGE_CURVE ( 'NONE', #19368, #28359, #41914, .T. ) ;
#39865 = EDGE_LOOP ( 'NONE', ( #22568, #7134 ) ) ;
#39866 = CARTESIAN_POINT ( 'NONE',  ( 17.99999999999999645, -18.35539002514308038, -110.6858262410711831 ) ) ;
#39867 = ORIENTED_EDGE ( 'NONE', *, *, #13119, .T. ) ;
#39868 = CARTESIAN_POINT ( 'NONE',  ( 16.96065435355295392, 40.00000000000000000, -19.31014141889295743 ) ) ;
#39869 = CARTESIAN_POINT ( 'NONE',  ( -91.96080130434580724, -34.05525454449571043, 14.45886780445738218 ) ) ;
#39870 = CARTESIAN_POINT ( 'NONE',  ( 17.99999999999999645, 0.000000000000000000, 0.000000000000000000 ) ) ;
#39871 = ADVANCED_FACE ( 'NONE', ( #21500 ), #41723, .F. ) ;
#39872 = DIRECTION ( 'NONE',  ( 0.000000000000000000, 0.8477344278896721264, -0.5304209081197405196 ) ) ;
#39873 = FACE_OUTER_BOUND ( 'NONE', #25592, .T. ) ;
#39874 = VERTEX_POINT ( 'NONE', #7695 ) ;
#39875 = CARTESIAN_POINT ( 'NONE',  ( 0.000000000000000000, 51.85248208264517444, 3.914090171286374265 ) ) ;
#39876 = ORIENTED_EDGE ( 'NONE', *, *, #9111, .T. ) ;
#39877 = AXIS2_PLACEMENT_3D ( 'NONE', #41175, #1476, #11115 ) ;
#39878 = DIRECTION ( 'NONE',  ( 0.000000000000000000, 1.234887898152981424E-13, -1.000000000000000000 ) ) ;
#39879 = DIRECTION ( 'NONE',  ( -1.000000000000000000, -0.000000000000000000, -0.000000000000000000 ) ) ;
#39880 = EDGE_LOOP ( 'NONE', ( #30422, #15099 ) ) ;
#39881 = DIRECTION ( 'NONE',  ( -1.000000000000000000, -0.000000000000000000, 0.000000000000000000 ) ) ;
#39882 = AXIS2_PLACEMENT_3D ( 'NONE', #26593, #2344, #6079 ) ;
#39883 = CARTESIAN_POINT ( 'NONE',  ( 17.99999999999999645, -13.57797752207947006, 33.34124362422470256 ) ) ;
#39884 = SHAPE_DEFINITION_REPRESENTATION ( #6402, #10434 ) ;
#39885 = CARTESIAN_POINT ( 'NONE',  ( 4.024499207728657879, -2.323545700935587988, -3.572172305156509964 ) ) ;
#39886 = CARTESIAN_POINT ( 'NONE',  ( -53.60515337853228601, 31.00000000000000355, -47.01024902908782366 ) ) ;
#39887 = AXIS2_PLACEMENT_3D ( 'NONE', #17029, #33143, #6953 ) ;
#39888 = EDGE_CURVE ( 'NONE', #1360, #2343, #16162, .T. ) ;
#39889 = EDGE_CURVE ( 'NONE', #1858, #40010, #40506, .T. ) ;
#39890 = ORIENTED_EDGE ( 'NONE', *, *, #43076, .F. ) ;
#39891 = CARTESIAN_POINT ( 'NONE',  ( -28.12618851199096781, 31.00000000000000355, 13.81902982503210708 ) ) ;
#39892 = EDGE_CURVE ( 'NONE', #14569, #36642, #14494, .T. ) ;
#39893 = ADVANCED_FACE ( 'NONE', ( #27806 ), #25189, .T. ) ;
#39894 = CARTESIAN_POINT ( 'NONE',  ( -63.57631528421845957, 40.00000000000000711, -31.33741679916209222 ) ) ;
#39895 = DIRECTION ( 'NONE',  ( -1.000000000000000000, 0.000000000000000000, -0.000000000000000000 ) ) ;
#39896 = CYLINDRICAL_SURFACE ( 'NONE', #43008, 31.49899999999999878 ) ;
#39897 = EDGE_LOOP ( 'NONE', ( #11704, #33884, #41635, #19317 ) ) ;
#39898 = DIRECTION ( 'NONE',  ( 1.000000000000000000, 0.000000000000000000, 0.000000000000000000 ) ) ;
#39899 = CARTESIAN_POINT ( 'NONE',  ( 9.000000000000001776, -0.6819280456820884240, -115.9979955608738607 ) ) ;
#39900 = CIRCLE ( 'NONE', #12786, 120.5010000000000332 ) ;
#39901 = ORIENTED_EDGE ( 'NONE', *, *, #6907, .T. ) ;
#39902 = CARTESIAN_POINT ( 'NONE',  ( -40.10416666498607441, 40.00000000000000000, -2.617993869485698344 ) ) ;
#39903 = CARTESIAN_POINT ( 'NONE',  ( -10.00000000000000000, 0.000000000000000000, 0.000000000000000000 ) ) ;
#39904 = CARTESIAN_POINT ( 'NONE',  ( 0.000000000000000000, -31.80866420683992857, 16.59709355804118402 ) ) ;
#39905 = VERTEX_POINT ( 'NONE', #14924 ) ;
#39906 = DIRECTION ( 'NONE',  ( -1.000000000000000000, 0.000000000000000000, -0.000000000000000000 ) ) ;
#39907 = LINE ( 'NONE', #12905, #25055 ) ;
#39908 = ORIENTED_EDGE ( 'NONE', *, *, #7476, .F. ) ;
#39909 = DIRECTION ( 'NONE',  ( -1.000000000000000000, 0.000000000000000000, -0.000000000000000000 ) ) ;
#39910 = ORIENTED_EDGE ( 'NONE', *, *, #33800, .F. ) ;
#39911 = PRESENTATION_LAYER_ASSIGNMENT (  '', '', ( #23250 ) ) ;
#39912 = AXIS2_PLACEMENT_3D ( 'NONE', #18079, #21572, #14995 ) ;
#39913 = ORIENTED_EDGE ( 'NONE', *, *, #30448, .F. ) ;
#39914 = DIRECTION ( 'NONE',  ( 3.009274222672345096E-17, 1.000000000000000000, -2.455023325076454960E-18 ) ) ;
#39915 = CARTESIAN_POINT ( 'NONE',  ( 5.735608225908778834, 31.00000000000000355, 89.40012361740336644 ) ) ;
#39916 = ORIENTED_EDGE ( 'NONE', *, *, #7410, .F. ) ;
#39917 = DIRECTION ( 'NONE',  ( -1.000000000000000000, 0.000000000000000000, 0.000000000000000000 ) ) ;
#39918 = EDGE_CURVE ( 'NONE', #10403, #10198, #8478, .T. ) ;
#39919 = CARTESIAN_POINT ( 'NONE',  ( 0.000000000000000000, 2.357898499370431722, -2.818925648462311528E-15 ) ) ;
#39920 = CARTESIAN_POINT ( 'NONE',  ( 0.000000000000000000, 0.000000000000000000, 0.000000000000000000 ) ) ;
#39921 = ORIENTED_EDGE ( 'NONE', *, *, #30036, .T. ) ;
#39922 = DIRECTION ( 'NONE',  ( 1.000000000000000000, 0.000000000000000000, 0.000000000000000000 ) ) ;
#39923 = DIRECTION ( 'NONE',  ( 0.000000000000000000, 0.000000000000000000, 1.000000000000000000 ) ) ;
#39925 = DIRECTION ( 'NONE',  ( 1.000000000000000000, 0.000000000000000000, 0.000000000000000000 ) ) ;
#39924 = DIRECTION ( 'NONE',  ( -1.000000000000000000, -0.000000000000000000, -0.000000000000000000 ) ) ;
#39926 = AXIS2_PLACEMENT_3D ( 'NONE', #31880, #38191, #1967 ) ;
#39927 = DIRECTION ( 'NONE',  ( 0.000000000000000000, 0.000000000000000000, -1.000000000000000000 ) ) ;
#39928 = ORIENTED_EDGE ( 'NONE', *, *, #38677, .T. ) ;
#39929 = SURFACE_SIDE_STYLE ('',( #42569 ) ) ;
#39930 = VECTOR ( 'NONE', #36635, 1000.000000000000000 ) ;
#39931 = CARTESIAN_POINT ( 'NONE',  ( 4.274771203358150196, 31.00000000000000355, -32.49882260841580006 ) ) ;
#39932 = ORIENTED_EDGE ( 'NONE', *, *, #21061, .F. ) ;
#39933 = DIRECTION ( 'NONE',  ( -1.000000000000000000, -0.000000000000000000, 0.000000000000000000 ) ) ;
#39934 = DIRECTION ( 'NONE',  ( 0.000000000000000000, 0.000000000000000000, 1.000000000000000000 ) ) ;
#39935 = VERTEX_POINT ( 'NONE', #34313 ) ;
#39936 = EDGE_CURVE ( 'NONE', #6132, #11201, #41215, .T. ) ;
#39937 = ADVANCED_FACE ( 'NONE', ( #8137 ), #18221, .T. ) ;
#39938 = DIRECTION ( 'NONE',  ( 1.000000000000000000, 0.000000000000000000, 0.000000000000000000 ) ) ;
#39939 = CARTESIAN_POINT ( 'NONE',  ( -35.29531037056285214, 40.00000000000000000, 17.40921588598563119 ) ) ;
#39940 = CARTESIAN_POINT ( 'NONE',  ( 47.09643503918425012, 40.00000000000000000, 3.164684800459844904 ) ) ;
#39941 = EDGE_CURVE ( 'NONE', #14485, #4058, #5672, .T. ) ;
#39942 = AXIS2_PLACEMENT_3D ( 'NONE', #3347, #37547, #9906 ) ;
#39943 = ORIENTED_EDGE ( 'NONE', *, *, #11194, .T. ) ;
#39944 = VERTEX_POINT ( 'NONE', #41495 ) ;
#39945 = CARTESIAN_POINT ( 'NONE',  ( 5.200000000000002842, 0.000000000000000000, 0.000000000000000000 ) ) ;
#39946 = CARTESIAN_POINT ( 'NONE',  ( 0.000000000000000000, -88.56657216608662964, 68.87840567545892156 ) ) ;
#39947 = CYLINDRICAL_SURFACE ( 'NONE', #31508, 130.0000000000000000 ) ;
#39948 = CARTESIAN_POINT ( 'NONE',  ( 17.99999999999999645, -7.220349212960696761, 35.26849241522662481 ) ) ;
#39949 = ORIENTED_EDGE ( 'NONE', *, *, #28659, .F. ) ;
#39950 = CARTESIAN_POINT ( 'NONE',  ( -106.4195705685741871, -106.4195705685773135, 6.999999999999754863 ) ) ;
#39951 = ORIENTED_EDGE ( 'NONE', *, *, #9342, .F. ) ;
#39952 = FACE_OUTER_BOUND ( 'NONE', #26292, .T. ) ;
#39953 = CARTESIAN_POINT ( 'NONE',  ( 1.828356344711641102, 3.563200125723180900, -5.433716356636336675E-16 ) ) ;
#39954 = EDGE_CURVE ( 'NONE', #4807, #7922, #15464, .T. ) ;
#39955 = ORIENTED_EDGE ( 'NONE', *, *, #38434, .F. ) ;
#39956 = CARTESIAN_POINT ( 'NONE',  ( 17.99999999999999645, 22.66088087769180603, 21.87856208362564914 ) ) ;
#39957 = AXIS2_PLACEMENT_3D ( 'NONE', #41450, #11601, #24942 ) ;
#39958 = FACE_OUTER_BOUND ( 'NONE', #1380, .T. ) ;
#39959 = ORIENTED_EDGE ( 'NONE', *, *, #25501, .T. ) ;
#39960 = CARTESIAN_POINT ( 'NONE',  ( 17.99999999999999645, -28.62203781743013664, 14.19692359621445199 ) ) ;
#39961 = VERTEX_POINT ( 'NONE', #38232 ) ;
#39962 = CARTESIAN_POINT ( 'NONE',  ( 0.000000000000000000, 0.000000000000000000, 0.000000000000000000 ) ) ;
#39963 = AXIS2_PLACEMENT_3D ( 'NONE', #24252, #30560, #40763 ) ;
#39964 = ORIENTED_EDGE ( 'NONE', *, *, #24254, .F. ) ;
#39966 = ORIENTED_EDGE ( 'NONE', *, *, #16912, .T. ) ;
#39965 = DIRECTION ( 'NONE',  ( -1.000000000000000000, -0.000000000000000000, -0.000000000000000000 ) ) ;
#39967 = CARTESIAN_POINT ( 'NONE',  ( 43.45541166190962912, 31.00000000000000355, -49.38773770141698805 ) ) ;
#39968 = ORIENTED_EDGE ( 'NONE', *, *, #41605, .T. ) ;
#39969 = CARTESIAN_POINT ( 'NONE',  ( 17.99999999999999645, 0.000000000000000000, 0.000000000000000000 ) ) ;
#39970 = AXIS2_PLACEMENT_3D ( 'NONE', #34815, #37851, #16819 ) ;
#39971 = ORIENTED_EDGE ( 'NONE', *, *, #33377, .T. ) ;
#39973 = AXIS2_PLACEMENT_3D ( 'NONE', #33416, #36897, #16878 ) ;
#39972 = DIRECTION ( 'NONE',  ( 0.000000000000000000, 0.000000000000000000, 1.000000000000000000 ) ) ;
#39974 = VERTEX_POINT ( 'NONE', #8348 ) ;
#39975 = CARTESIAN_POINT ( 'NONE',  ( -35.65230965300054322, 40.00000000000000000, 72.05959145982365044 ) ) ;
#39977 = CARTESIAN_POINT ( 'NONE',  ( 17.99999999999999645, 107.1354928292869744, 44.47455650398100602 ) ) ;
#39976 = CARTESIAN_POINT ( 'NONE',  ( -0.2142857142857142738, -10.49781318335647917, -1.199999999999999956 ) ) ;
#39978 = LINE ( 'NONE', #3982, #39391 ) ;
#39979 = ORIENTED_EDGE ( 'NONE', *, *, #21615, .T. ) ;
#39980 = DIRECTION ( 'NONE',  ( -1.000000000000000000, 0.000000000000000000, -0.000000000000000000 ) ) ;
#39981 = AXIS2_PLACEMENT_3D ( 'NONE', #2988, #12650, #9784 ) ;
#39982 = ORIENTED_EDGE ( 'NONE', *, *, #23798, .T. ) ;
#39983 = SHAPE_REPRESENTATION_RELATIONSHIP ( 'NONE' , 'NONE' ,  #40225, #38478 ) ;
#39984 = AXIS2_PLACEMENT_3D ( 'NONE', #37819, #40872, #38463 ) ;
#39985 = DIRECTION ( 'NONE',  ( 0.000000000000000000, 0.000000000000000000, 1.000000000000000000 ) ) ;
#39986 = CARTESIAN_POINT ( 'NONE',  ( 34.02738612458995959, 31.00000000000000355, 69.00154638599002510 ) ) ;
#39988 = CARTESIAN_POINT ( 'NONE',  ( 2.742827927723449299, 3.035229711104609596, -3.433252694550591233 ) ) ;
#39987 = CARTESIAN_POINT ( 'NONE',  ( 56.05503971749756431, -2.055254544495723756, 8.006123197671259462 ) ) ;
#39989 = ORIENTED_EDGE ( 'NONE', *, *, #34228, .T. ) ;
#39990 = AXIS2_PLACEMENT_3D ( 'NONE', #39411, #38987, #9112 ) ;
#39991 = EDGE_CURVE ( 'NONE', #40772, #40246, #798, .T. ) ;
#39992 = DIRECTION ( 'NONE',  ( 0.000000000000000000, 0.000000000000000000, 1.000000000000000000 ) ) ;
#39993 = VECTOR ( 'NONE', #23548, 1000.000000000000000 ) ;
#39994 = ORIENTED_EDGE ( 'NONE', *, *, #9767, .F. ) ;
#39995 = CARTESIAN_POINT ( 'NONE',  ( 0.000000000000000000, 86.84764344322962870, 76.89919913989776035 ) ) ;
#39996 = DIRECTION ( 'NONE',  ( 0.000000000000000000, 0.000000000000000000, 1.000000000000000000 ) ) ;
#39997 = CARTESIAN_POINT ( 'NONE',  ( -101.9959696149863646, 31.00000000000000711, -0.1269066430510134569 ) ) ;
#39998 = EDGE_CURVE ( 'NONE', #6210, #19145, #32879, .T. ) ;
#39999 = CARTESIAN_POINT ( 'NONE',  ( -9.000000000000005329, 0.000000000000000000, -13.40000000000000213 ) ) ;
#40000 = EDGE_CURVE ( 'NONE', #7485, #3574, #39784, .T. ) ;
#40001 = CIRCLE ( 'NONE', #17807, 59.00000000000000711 ) ;
#40002 = VERTEX_POINT ( 'NONE', #31052 ) ;
#40003 = DIRECTION ( 'NONE',  ( 1.000000000000000000, 0.000000000000000000, 0.000000000000000000 ) ) ;
#40004 = VERTEX_POINT ( 'NONE', #1143 ) ;
#40005 = DIRECTION ( 'NONE',  ( 0.000000000000000000, 0.000000000000000000, 1.000000000000000000 ) ) ;
#40006 = EDGE_CURVE ( 'NONE', #7826, #14755, #23155, .T. ) ;
#40007 = DIRECTION ( 'NONE',  ( 1.000000000000000000, 0.000000000000000000, 0.000000000000000000 ) ) ;
#40008 = DIRECTION ( 'NONE',  ( 0.000000000000000000, 0.000000000000000000, 1.000000000000000000 ) ) ;
#40009 = EDGE_LOOP ( 'NONE', ( #33881, #26500, #40442, #20210 ) ) ;
#40010 = VERTEX_POINT ( 'NONE', #34525 ) ;
#40011 = DIRECTION ( 'NONE',  ( -1.000000000000000000, -0.000000000000000000, -0.000000000000000000 ) ) ;
#40012 = VECTOR ( 'NONE', #32653, 1000.000000000000000 ) ;
#40013 = DIRECTION ( 'NONE',  ( -1.000000000000000000, 0.000000000000000000, 0.000000000000000000 ) ) ;
#40014 = FACE_OUTER_BOUND ( 'NONE', #41264, .T. ) ;
#40015 = CIRCLE ( 'NONE', #298, 59.00000000000000000 ) ;
#40017 = VERTEX_POINT ( 'NONE', #32545 ) ;
#40016 = DIRECTION ( 'NONE',  ( 1.000000000000000000, 0.000000000000000000, 0.000000000000000000 ) ) ;
#40018 = CARTESIAN_POINT ( 'NONE',  ( -24.64063138600606351, 31.00000000000000355, 18.85097431369995746 ) ) ;
#40019 = DIRECTION ( 'NONE',  ( -1.000000000000000000, -0.000000000000000000, 0.000000000000000000 ) ) ;
#40020 = VECTOR ( 'NONE', #6420, 1000.000000000000000 ) ;
#40022 = ORIENTED_EDGE ( 'NONE', *, *, #31071, .T. ) ;
#40021 = DIRECTION ( 'NONE',  ( -1.000000000000000000, -0.000000000000000000, -0.000000000000000000 ) ) ;
#40023 = VECTOR ( 'NONE', #17815, 1000.000000000000000 ) ;
#40024 = ORIENTED_EDGE ( 'NONE', *, *, #10352, .T. ) ;
#40025 = FACE_OUTER_BOUND ( 'NONE', #4868, .T. ) ;
#40026 = ADVANCED_FACE ( 'NONE', ( #12285 ), #12707, .T. ) ;
#40027 = DIRECTION ( 'NONE',  ( 0.000000000000000000, 0.000000000000000000, 1.000000000000000000 ) ) ;
#40028 = CARTESIAN_POINT ( 'NONE',  ( 54.55067978551168295, 40.00000000000000000, 18.62288743479739495 ) ) ;
#40029 = CARTESIAN_POINT ( 'NONE',  ( 18.00000000000000355, -35.20873326984057883, -31.88259874184068465 ) ) ;
#40030 = CARTESIAN_POINT ( 'NONE',  ( 17.99999999999999645, -6.007673836297749759, -35.49518073030004217 ) ) ;
#40031 = CYLINDRICAL_SURFACE ( 'NONE', #29713, 7.500000000000000000 ) ;
#40032 = VERTEX_POINT ( 'NONE', #38649 ) ;
#40033 = DIRECTION ( 'NONE',  ( -1.000000000000000000, -0.000000000000000000, -0.000000000000000000 ) ) ;
#40034 = ORIENTED_EDGE ( 'NONE', *, *, #37465, .T. ) ;
#40035 = DIRECTION ( 'NONE',  ( -1.000000000000000000, -0.000000000000000000, -0.000000000000000000 ) ) ;
#40036 = CYLINDRICAL_SURFACE ( 'NONE', #8746, 59.00000000000000000 ) ;
#40037 = CARTESIAN_POINT ( 'NONE',  ( -24.21661388771557100, 31.00000000000000355, 41.94898165618241137 ) ) ;
#40038 = DIRECTION ( 'NONE',  ( -1.000000000000000000, 0.000000000000000000, 0.000000000000000000 ) ) ;
#40039 = ORIENTED_EDGE ( 'NONE', *, *, #35482, .F. ) ;
#40040 = VECTOR ( 'NONE', #6885, 1000.000000000000000 ) ;
#40041 = ADVANCED_FACE ( 'NONE', ( #42351 ), #39072, .T. ) ;
#40042 = DIRECTION ( 'NONE',  ( 0.000000000000000000, -0.4132121857683668797, -0.9106347728549183396 ) ) ;
#40043 = EDGE_LOOP ( 'NONE', ( #33227, #35420 ) ) ;
#40044 = CARTESIAN_POINT ( 'NONE',  ( 11.68784703496123711, 40.00000000000000000, -20.25319168173327355 ) ) ;
#40045 = CIRCLE ( 'NONE', #33092, 7.500000000000000000 ) ;
#40046 = ORIENTED_EDGE ( 'NONE', *, *, #5217, .F. ) ;
#40047 = CARTESIAN_POINT ( 'NONE',  ( 0.000000000000000000, -5.919241748379376666, -31.39643714728462953 ) ) ;
#40048 = CARTESIAN_POINT ( 'NONE',  ( -35.33737842959504150, 31.00000000000000355, 60.98257694382487415 ) ) ;
#40050 = CARTESIAN_POINT ( 'NONE',  ( -68.78002826189113250, 40.00000000000000711, -23.46745878763887916 ) ) ;
#40049 = VECTOR ( 'NONE', #20873, 1000.000000000000000 ) ;
#40051 = CARTESIAN_POINT ( 'NONE',  ( 17.99999999999999645, -22.66088087769164972, -21.87856208362581256 ) ) ;
#40052 = ADVANCED_FACE ( 'NONE', ( #42559 ), #22339, .F. ) ;
#40053 = ORIENTED_EDGE ( 'NONE', *, *, #9275, .T. ) ;
#40054 = ORIENTED_EDGE ( 'NONE', *, *, #1711, .T. ) ;
#40055 = DIRECTION ( 'NONE',  ( 3.009274222672345096E-17, 1.000000000000000000, -2.455023325076454960E-18 ) ) ;
#40056 = DIRECTION ( 'NONE',  ( 0.000000000000000000, 0.000000000000000000, -1.000000000000000000 ) ) ;
#40057 = CARTESIAN_POINT ( 'NONE',  ( -10.00000000000000000, 0.000000000000000000, 0.000000000000000000 ) ) ;
#40059 = EDGE_LOOP ( 'NONE', ( #27898, #13522, #11253, #30800 ) ) ;
#40058 = CYLINDRICAL_SURFACE ( 'NONE', #20709, 116.0000000000000000 ) ;
#40060 = ADVANCED_FACE ( 'NONE', ( #3042 ), #26011, .F. ) ;
#40061 = CARTESIAN_POINT ( 'NONE',  ( 17.99999999999999645, 40.37724737310206535, -104.6802291180863023 ) ) ;
#40062 = VERTEX_POINT ( 'NONE', #25392 ) ;
#40063 = LINE ( 'NONE', #6711, #1437 ) ;
#40064 = CARTESIAN_POINT ( 'NONE',  ( -10.77850749866037816, 40.00000000000000000, -81.75987728344749428 ) ) ;
#40065 = LINE ( 'NONE', #3631, #15271 ) ;
#40066 = CIRCLE ( 'NONE', #14330, 25.00000000000002132 ) ;
#40067 = APPLICATION_CONTEXT ( 'automotive_design' ) ;
#40068 = ORIENTED_EDGE ( 'NONE', *, *, #14612, .F. ) ;
#40069 = FACE_OUTER_BOUND ( 'NONE', #6814, .T. ) ;
#40070 = DIRECTION ( 'NONE',  ( -0.000000000000000000, -0.000000000000000000, 1.000000000000000000 ) ) ;
#40071 = CIRCLE ( 'NONE', #7324, 2.649999999999999467 ) ;
#40072 = ORIENTED_EDGE ( 'NONE', *, *, #7526, .F. ) ;
#40073 = AXIS2_PLACEMENT_3D ( 'NONE', #41219, #14658, #863 ) ;
#40074 = AXIS2_PLACEMENT_3D ( 'NONE', #28199, #21473, #38622 ) ;
#40075 = ORIENTED_EDGE ( 'NONE', *, *, #4325, .F. ) ;
#40076 = DIRECTION ( 'NONE',  ( -0.000000000000000000, -1.060184893785364939E-15, -1.000000000000000000 ) ) ;
#40078 = ORIENTED_EDGE ( 'NONE', *, *, #17270, .T. ) ;
#40077 = EDGE_CURVE ( 'NONE', #31266, #2932, #13362, .T. ) ;
#40079 = CARTESIAN_POINT ( 'NONE',  ( -18.31940394017777862, 40.00000000000000000, -14.05611420671344014 ) ) ;
#40080 = DIRECTION ( 'NONE',  ( 0.000000000000000000, 0.6845471059286846183, 0.7289686274214153272 ) ) ;
#40081 = CARTESIAN_POINT ( 'NONE',  ( 17.99999999999999645, 0.000000000000000000, 0.000000000000000000 ) ) ;
#40082 = AXIS2_PLACEMENT_3D ( 'NONE', #27205, #27413, #40686 ) ;
#40083 = ADVANCED_FACE ( 'NONE', ( #15995 ), #12500, .T. ) ;
#40084 = AXIS2_PLACEMENT_3D ( 'NONE', #36858, #22161, #12098 ) ;
#40085 = CARTESIAN_POINT ( 'NONE',  ( 146.1418929693599580, -12.05525454449572820, -53.89157828313137344 ) ) ;
#40086 = VECTOR ( 'NONE', #10054, 1000.000000000000000 ) ;
#40087 = CARTESIAN_POINT ( 'NONE',  ( 4.000000000000000000, 2.309401076758497151, -3.433295621305379353 ) ) ;
#40088 = ORIENTED_EDGE ( 'NONE', *, *, #25283, .F. ) ;
#40090 = DIRECTION ( 'NONE',  ( 0.000000000000000000, -0.9714298932647122964, 0.2373266998711055509 ) ) ;
#40089 = CARTESIAN_POINT ( 'NONE',  ( 0.000000000000000000, 82.63181128086733906, 81.41243003647002752 ) ) ;
#40092 = VERTEX_POINT ( 'NONE', #25817 ) ;
#40091 = CIRCLE ( 'NONE', #38706, 116.0000000000000000 ) ;
#40093 = DIRECTION ( 'NONE',  ( 0.000000000000000000, 0.9574220383620062336, -0.2886919473396183933 ) ) ;
#40094 = CARTESIAN_POINT ( 'NONE',  ( -18.63466726053507472, 31.00000000000000355, -9.179856479542758407 ) ) ;
#40095 = ORIENTED_EDGE ( 'NONE', *, *, #13272, .F. ) ;
#40096 = DIRECTION ( 'NONE',  ( 0.000000000000000000, 0.5076658003388351270, 0.8615540813938089570 ) ) ;
#40097 = DIRECTION ( 'NONE',  ( -1.000000000000000000, -0.000000000000000000, -0.000000000000000000 ) ) ;
#40098 = CONTEXT_DEPENDENT_SHAPE_REPRESENTATION ( #7204, #9176 ) ;
#40099 = EDGE_CURVE ( 'NONE', #22186, #38131, #7760, .T. ) ;
#40100 = CYLINDRICAL_SURFACE ( 'NONE', #2334, 47.49900000000000233 ) ;
#40101 = CARTESIAN_POINT ( 'NONE',  ( 59.08215048199704711, 31.00000000000000000, 29.12166076728773589 ) ) ;
#40103 = ORIENTED_EDGE ( 'NONE', *, *, #7327, .F. ) ;
#40102 = CIRCLE ( 'NONE', #10159, 20.00000000000000711 ) ;
#40104 = CARTESIAN_POINT ( 'NONE',  ( 45.11287655886648906, 31.00000000000000355, -12.00022417491544324 ) ) ;
#40105 = CARTESIAN_POINT ( 'NONE',  ( -34.66105084696506822, 40.00000000000000000, 70.31756248751102589 ) ) ;
#40106 = AXIS2_PLACEMENT_3D ( 'NONE', #15516, #32275, #29238 ) ;
#40107 = CIRCLE ( 'NONE', #1794, 14.70000000000000107 ) ;
#40108 = EDGE_CURVE ( 'NONE', #42317, #26674, #32155, .T. ) ;
#40109 = DIRECTION ( 'NONE',  ( 1.000000000000000000, 0.000000000000000000, 0.000000000000000000 ) ) ;
#40110 = AXIS2_PLACEMENT_3D ( 'NONE', #2266, #28077, #8842 ) ;
#40111 = CARTESIAN_POINT ( 'NONE',  ( -102.4608013043457362, -34.05525454449571043, 14.45886780445633946 ) ) ;
#40112 = EDGE_CURVE ( 'NONE', #40515, #12272, #2406, .T. ) ;
#40113 = STYLED_ITEM ( 'NONE', ( #12838 ), #28662 ) ;
#40114 = AXIS2_PLACEMENT_3D ( 'NONE', #40791, #10948, #36888 ) ;
#40115 = ORIENTED_EDGE ( 'NONE', *, *, #40677, .F. ) ;
#40116 = ADVANCED_FACE ( 'NONE', ( #38868 ), #9199, .F. ) ;
#40117 = CARTESIAN_POINT ( 'NONE',  ( 17.99999999999999645, 97.89532456239568603, -54.81585448086097045 ) ) ;
#40118 = CARTESIAN_POINT ( 'NONE',  ( -6.473970235329672780E-16, -4.862606272033106691, -3.745885042887442395 ) ) ;
#40119 = CIRCLE ( 'NONE', #28353, 59.00000000000000000 ) ;
#40120 = VERTEX_POINT ( 'NONE', #39274 ) ;
#40121 = CARTESIAN_POINT ( 'NONE',  ( 28.40420691229738281, 40.00000000000000000, 49.17333623205379922 ) ) ;
#40122 = CYLINDRICAL_SURFACE ( 'NONE', #13848, 120.5010000000000190 ) ;
#40123 = DIRECTION ( 'NONE',  ( -1.000000000000000000, -0.000000000000000000, 0.000000000000000000 ) ) ;
#40124 = ORIENTED_EDGE ( 'NONE', *, *, #40432, .T. ) ;
#40125 = DIRECTION ( 'NONE',  ( 0.000000000000000000, 0.000000000000000000, 1.000000000000000000 ) ) ;
#40126 = CARTESIAN_POINT ( 'NONE',  ( 17.99999999999999645, 106.5605152861902951, 56.26142179985861702 ) ) ;
#40127 = ORIENTED_EDGE ( 'NONE', *, *, #11703, .T. ) ;
#40128 = CARTESIAN_POINT ( 'NONE',  ( 0.000000000000000000, 0.000000000000000000, 0.000000000000000000 ) ) ;
#40129 = VERTEX_POINT ( 'NONE', #9405 ) ;
#40130 = ORIENTED_EDGE ( 'NONE', *, *, #20256, .F. ) ;
#40131 = DIRECTION ( 'NONE',  ( -1.000000000000000000, -0.000000000000000000, -0.000000000000000000 ) ) ;
#40132 = ADVANCED_FACE ( 'NONE', ( #6142 ), #35788, .F. ) ;
#40133 = CARTESIAN_POINT ( 'NONE',  ( 63.29164158772582027, 31.00000000000000000, -71.97807289022838972 ) ) ;
#40134 = ORIENTED_EDGE ( 'NONE', *, *, #1542, .F. ) ;
#40135 = CARTESIAN_POINT ( 'NONE',  ( 0.000000000000000000, 0.000000000000000000, 0.000000000000000000 ) ) ;
#40136 = ADVANCED_FACE ( 'NONE', ( #42761 ), #16412, .T. ) ;
#40137 = AXIS2_PLACEMENT_3D ( 'NONE', #26375, #22479, #32257 ) ;
#40138 = EDGE_CURVE ( 'NONE', #15922, #4444, #12696, .T. ) ;
#40139 = EDGE_CURVE ( 'NONE', #43139, #29204, #18995, .T. ) ;
#40140 = DIRECTION ( 'NONE',  ( 0.000000000000000000, 0.000000000000000000, 1.000000000000000000 ) ) ;
#40141 = AXIS2_PLACEMENT_3D ( 'NONE', #21823, #31593, #27916 ) ;
#40143 = CARTESIAN_POINT ( 'NONE',  ( 0.000000000000000000, -21.48775762007842260, -23.64423737150161031 ) ) ;
#40142 = AXIS2_PLACEMENT_3D ( 'NONE', #41827, #11980, #41618 ) ;
#40144 = ORIENTED_EDGE ( 'NONE', *, *, #2072, .T. ) ;
#40145 = AXIS2_PLACEMENT_3D ( 'NONE', #37817, #37392, #7509 ) ;
#40146 = DIRECTION ( 'NONE',  ( -1.000000000000000000, 0.000000000000000000, -0.000000000000000000 ) ) ;
#40147 = DIRECTION ( 'NONE',  ( 1.000000000000000000, 0.000000000000000000, -0.000000000000000000 ) ) ;
#40149 = CARTESIAN_POINT ( 'NONE',  ( 17.99999999999999645, -26.29521155129861398, 17.34211205339337880 ) ) ;
#40148 = DIRECTION ( 'NONE',  ( -0.000000000000000000, 1.000000000000000000, 1.224646799147353207E-16 ) ) ;
#40150 = CIRCLE ( 'NONE', #42954, 120.5010000000000048 ) ;
#40151 = DIRECTION ( 'NONE',  ( -1.000000000000000000, 0.000000000000000000, 0.000000000000000000 ) ) ;
#40152 = ORIENTED_EDGE ( 'NONE', *, *, #17446, .F. ) ;
#40153 = VECTOR ( 'NONE', #25138, 1000.000000000000000 ) ;
#40154 = CARTESIAN_POINT ( 'NONE',  ( -27.33276042269523387, 31.00000000000000355, -31.15086293565511966 ) ) ;
#40155 = ORIENTED_EDGE ( 'NONE', *, *, #4159, .T. ) ;
#40156 = DIRECTION ( 'NONE',  ( 0.000000000000000000, 0.000000000000000000, 1.000000000000000000 ) ) ;
#40157 = CIRCLE ( 'NONE', #17340, 2.649999999999979039 ) ;
#40158 = CARTESIAN_POINT ( 'NONE',  ( 17.99999999999999645, -29.02167576844032482, -108.3790330702172611 ) ) ;
#40159 = ORIENTED_EDGE ( 'NONE', *, *, #34960, .F. ) ;
#40160 = DIRECTION ( 'NONE',  ( -1.000000000000000000, -0.000000000000000000, -0.000000000000000000 ) ) ;
#40161 = CARTESIAN_POINT ( 'NONE',  ( -44.11856065373272173, 40.00000000000000000, -25.46949057303769948 ) ) ;
#40162 = CARTESIAN_POINT ( 'NONE',  ( 29.49207856986237530, 40.00000000000000000, 38.57905506995709288 ) ) ;
#40163 = ADVANCED_FACE ( 'NONE', ( #19916 ), #10280, .F. ) ;
#40164 = ORIENTED_EDGE ( 'NONE', *, *, #23368, .T. ) ;
#40165 = DIRECTION ( 'NONE',  ( -1.000000000000000000, 0.000000000000000000, -0.000000000000000000 ) ) ;
#40166 = DIRECTION ( 'NONE',  ( 1.000000000000000000, 0.000000000000000000, 0.000000000000000000 ) ) ;
#40167 = EDGE_CURVE ( 'NONE', #8333, #37461, #9871, .T. ) ;
#40168 = CIRCLE ( 'NONE', #42263, 20.00000000000000711 ) ;
#40169 = CARTESIAN_POINT ( 'NONE',  ( 17.99999999999999645, 57.69704296431325474, -105.7900857083224224 ) ) ;
#40170 = CIRCLE ( 'NONE', #34621, 13.59999999999999964 ) ;
#40171 = VERTEX_POINT ( 'NONE', #10763 ) ;
#40172 = CARTESIAN_POINT ( 'NONE',  ( -19.76500330823589735, 40.00000000000000000, -5.286999072153966139 ) ) ;
#40173 = ORIENTED_EDGE ( 'NONE', *, *, #36402, .F. ) ;
#40174 = CARTESIAN_POINT ( 'NONE',  ( 31.80287614962791665, -14.05525454449571754, 69.29271901957253021 ) ) ;
#40175 = DIRECTION ( 'NONE',  ( 0.000000000000000000, 0.000000000000000000, 1.000000000000000000 ) ) ;
#40176 = AXIS2_PLACEMENT_3D ( 'NONE', #31251, #41465, #28421 ) ;
#40177 = AXIS2_PLACEMENT_3D ( 'NONE', #28748, #42225, #7842 ) ;
#40178 = ORIENTED_EDGE ( 'NONE', *, *, #6370, .T. ) ;
#40179 = CIRCLE ( 'NONE', #29796, 116.0000000000000000 ) ;
#40180 = DIRECTION ( 'NONE',  ( 0.000000000000000000, -0.9980267284282723361, 0.06279051952930260472 ) ) ;
#40181 = DIRECTION ( 'NONE',  ( -1.000000000000000000, -0.000000000000000000, -0.000000000000000000 ) ) ;
#40182 = VERTEX_POINT ( 'NONE', #203 ) ;
#40183 = FACE_OUTER_BOUND ( 'NONE', #19315, .T. ) ;
#40184 = CONICAL_SURFACE ( 'NONE', #4668, 5.560781378645573980, 1.221730476396046816 ) ;
#40185 = ORIENTED_EDGE ( 'NONE', *, *, #33377, .F. ) ;
#40186 = CARTESIAN_POINT ( 'NONE',  ( 17.99999999999999645, 21.55123232222474172, 118.5581519187672654 ) ) ;
#40187 = AXIS2_PLACEMENT_3D ( 'NONE', #24074, #22988, #23194 ) ;
#40188 = ORIENTED_EDGE ( 'NONE', *, *, #9409, .F. ) ;
#40190 = VERTEX_POINT ( 'NONE', #14005 ) ;
#40189 = CARTESIAN_POINT ( 'NONE',  ( 1.598609366639573350E-14, -1.063425437509180407E-13, -40.00000000000000000 ) ) ;
#40191 = CIRCLE ( 'NONE', #3275, 4.000000000000000000 ) ;
#40192 = CARTESIAN_POINT ( 'NONE',  ( 51.26988013555838819, 31.00000000000000355, 45.10883117380814866 ) ) ;
#40193 = VERTEX_POINT ( 'NONE', #16652 ) ;
#40194 = CYLINDRICAL_SURFACE ( 'NONE', #2144, 59.00000000000000000 ) ;
#40195 = EDGE_CURVE ( 'NONE', #35175, #21953, #37744, .T. ) ;
#40196 = ADVANCED_FACE ( 'NONE', ( #33188 ), #33612, .F. ) ;
#40197 = EDGE_CURVE ( 'NONE', #32209, #41913, #34981, .T. ) ;
#40198 = VERTEX_POINT ( 'NONE', #36887 ) ;
#40199 = CARTESIAN_POINT ( 'NONE',  ( 9.000000000000001776, -7.162210897276081845, 51.50439529848825515 ) ) ;
#40200 = PRODUCT_DEFINITION_SHAPE ( 'NONE', 'NONE',  #43185 ) ;
#40201 = EDGE_CURVE ( 'NONE', #20548, #41700, #22473, .T. ) ;
#40202 = VERTEX_POINT ( 'NONE', #39709 ) ;
#40203 = CARTESIAN_POINT ( 'NONE',  ( 77.59064570039033981, 39.99999999999999289, -38.12735739512951483 ) ) ;
#40204 = CIRCLE ( 'NONE', #36032, 13.59999999999999787 ) ;
#40206 = DIRECTION ( 'NONE',  ( 1.000000000000000000, 0.000000000000000000, 0.000000000000000000 ) ) ;
#40205 = CARTESIAN_POINT ( 'NONE',  ( 9.000000000000000000, 18.42432724429473012, 30.92804820216009176 ) ) ;
#40207 = CARTESIAN_POINT ( 'NONE',  ( 18.00000000000000355, 0.000000000000000000, 0.000000000000000000 ) ) ;
#40208 = ORIENTED_EDGE ( 'NONE', *, *, #30862, .F. ) ;
#40209 = DIRECTION ( 'NONE',  ( 0.000000000000000000, 1.000000000000000000, -1.060184893785364939E-15 ) ) ;
#40210 = AXIS2_PLACEMENT_3D ( 'NONE', #12475, #41696, #15120 ) ;
#40211 = ORIENTED_EDGE ( 'NONE', *, *, #13301, .F. ) ;
#40212 = AXIS2_PLACEMENT_3D ( 'NONE', #25177, #34740, #15553 ) ;
#40213 = CYLINDRICAL_SURFACE ( 'NONE', #35915, 47.49900000000000233 ) ;
#40214 = AXIS2_PLACEMENT_3D ( 'NONE', #42216, #35254, #5149 ) ;
#40215 = CARTESIAN_POINT ( 'NONE',  ( 130.0000000000000284, 1.638195277402996435E-14, -20.00000000000000000 ) ) ;
#40216 = CIRCLE ( 'NONE', #3264, 125.9999999999993605 ) ;
#40217 = CARTESIAN_POINT ( 'NONE',  ( -6.054110834496889026, 31.00000000000000355, -92.39583333400220511 ) ) ;
#40218 = CARTESIAN_POINT ( 'NONE',  ( 4.175002511812151873, 2.208363329454889445, -3.469254087858244073 ) ) ;
#40219 = ORIENTED_EDGE ( 'NONE', *, *, #23937, .T. ) ;
#40220 = DIRECTION ( 'NONE',  ( 1.000000000000000000, -1.373900992973642263E-15, -3.016910393003158636E-16 ) ) ;
#40221 = VERTEX_POINT ( 'NONE', #30357 ) ;
#40222 = DIRECTION ( 'NONE',  ( 0.000000000000000000, 0.1590634960190655256, 0.9872683547213456645 ) ) ;
#40223 = DIRECTION ( 'NONE',  ( -1.000000000000000000, 0.000000000000000000, -0.000000000000000000 ) ) ;
#40224 = CARTESIAN_POINT ( 'NONE',  ( -76.05825820879897492, 31.00000000000000711, 66.55365856249082412 ) ) ;
#40225 = SHAPE_REPRESENTATION ( 'spur gear_iso_ISO - Spur gear 2M 34T 20PA 18FW ---S34A75H50L30.0N', ( #13552 ), #32277 ) ;
#40226 = CARTESIAN_POINT ( 'NONE',  ( 8.919999999999998153, 0.000000000000000000, 0.000000000000000000 ) ) ;
#40227 = ADVANCED_FACE ( 'NONE', ( #6556 ), #23399, .F. ) ;
#40228 = EDGE_CURVE ( 'NONE', #15115, #42828, #28035, .T. ) ;
#40229 = ORIENTED_EDGE ( 'NONE', *, *, #10027, .T. ) ;
#40230 = DIRECTION ( 'NONE',  ( 0.000000000000000000, -0.9618256431728159361, -0.2736629900720938813 ) ) ;
#40231 = ORIENTED_EDGE ( 'NONE', *, *, #13562, .F. ) ;
#40232 = CARTESIAN_POINT ( 'NONE',  ( -10.00000000000000000, 0.000000000000000000, 0.000000000000000000 ) ) ;
#40233 = CIRCLE ( 'NONE', #2604, 20.00000000000000711 ) ;
#40234 = DIRECTION ( 'NONE',  ( 0.000000000000000000, 0.000000000000000000, 1.000000000000000000 ) ) ;
#40235 = CARTESIAN_POINT ( 'NONE',  ( -153.1499999999986699, -2.921326824731409465E-13, 7.000000000000041744 ) ) ;
#40236 = ORIENTED_EDGE ( 'NONE', *, *, #24361, .F. ) ;
#40237 = EDGE_LOOP ( 'NONE', ( #32144, #32007, #34457, #13581 ) ) ;
#40238 = DIRECTION ( 'NONE',  ( 0.000000000000000000, -0.9911528310040085277, 0.1327255272837126188 ) ) ;
#40239 = VECTOR ( 'NONE', #9377, 1000.000000000000000 ) ;
#40240 = DIRECTION ( 'NONE',  ( 0.000000000000000000, 0.000000000000000000, 1.000000000000000000 ) ) ;
#40241 = AXIS2_PLACEMENT_3D ( 'NONE', #20549, #37730, #27736 ) ;
#40242 = CYLINDRICAL_SURFACE ( 'NONE', #43135, 47.49900000000000233 ) ;
#40243 = AXIS2_PLACEMENT_3D ( 'NONE', #28868, #35173, #5300 ) ;
#40244 = VECTOR ( 'NONE', #35421, 1000.000000000000000 ) ;
#40246 = VERTEX_POINT ( 'NONE', #13361 ) ;
#40245 = DIRECTION ( 'NONE',  ( -1.000000000000000000, -0.000000000000000000, 0.000000000000000000 ) ) ;
#40247 = CARTESIAN_POINT ( 'NONE',  ( -7.793954689941437586, 31.00000000000000355, 28.94896179907300748 ) ) ;
#40248 = CARTESIAN_POINT ( 'NONE',  ( 17.99999999999999645, -103.4151313792866489, -61.85306461934516875 ) ) ;
#40249 = AXIS2_PLACEMENT_3D ( 'NONE', #33594, #13553, #23173 ) ;
#40250 = EDGE_CURVE ( 'NONE', #1826, #35253, #2194, .T. ) ;
#40252 = ORIENTED_EDGE ( 'NONE', *, *, #36054, .F. ) ;
#40251 = CARTESIAN_POINT ( 'NONE',  ( 17.99999999999999645, 61.59243992711585491, -93.77976230225978327 ) ) ;
#40253 = ADVANCED_FACE ( 'NONE', ( #10496 ), #26655, .T. ) ;
#40254 = ORIENTED_EDGE ( 'NONE', *, *, #33726, .F. ) ;
#40255 = DIRECTION ( 'NONE',  ( 0.1305261922200512403, -0.9914448613738104932, 0.000000000000000000 ) ) ;
#40256 = LINE ( 'NONE', #10387, #9873 ) ;
#40257 = CARTESIAN_POINT ( 'NONE',  ( 6.367266499441480931, 40.00000000000000000, 48.98256792610028754 ) ) ;
#40258 = LINE ( 'NONE', #16758, #41677 ) ;
#40259 = DIRECTION ( 'NONE',  ( 0.000000000000000000, 0.000000000000000000, 1.000000000000000000 ) ) ;
#40260 = ORIENTED_EDGE ( 'NONE', *, *, #41983, .F. ) ;
#40261 = DIRECTION ( 'NONE',  ( 0.000000000000000000, 0.000000000000000000, -1.000000000000000000 ) ) ;
#40262 = EDGE_CURVE ( 'NONE', #848, #1445, #7793, .T. ) ;
#40263 = VERTEX_POINT ( 'NONE', #37316 ) ;
#40264 = CARTESIAN_POINT ( 'NONE',  ( 17.99999999999999645, 0.000000000000000000, 0.000000000000000000 ) ) ;
#40265 = CARTESIAN_POINT ( 'NONE',  ( 0.000000000000000000, -101.1403355683142422, -56.80345518653591341 ) ) ;
#40266 = EDGE_CURVE ( 'NONE', #41379, #30344, #30151, .T. ) ;
#40267 = CARTESIAN_POINT ( 'NONE',  ( 21.71086051706764763, 31.00000000000000355, -37.60982366119799991 ) ) ;
#40268 = AXIS2_PLACEMENT_3D ( 'NONE', #24740, #41478, #21691 ) ;
#40269 = DIRECTION ( 'NONE',  ( 0.000000000000000000, 0.000000000000000000, 1.000000000000000000 ) ) ;
#40270 = ORIENTED_EDGE ( 'NONE', *, *, #35383, .F. ) ;
#40271 = CIRCLE ( 'NONE', #42362, 13.59999999999999787 ) ;
#40272 = DIRECTION ( 'NONE',  ( -1.000000000000000000, 0.000000000000000000, 0.000000000000000000 ) ) ;
#40273 = ORIENTED_EDGE ( 'NONE', *, *, #23694, .T. ) ;
#40274 = CARTESIAN_POINT ( 'NONE',  ( -20.10416666680962550, 40.00000000000000000, -1.308996940106889273 ) ) ;
#40275 = AXIS2_PLACEMENT_3D ( 'NONE', #27582, #27813, #41065 ) ;
#40276 = ORIENTED_EDGE ( 'NONE', *, *, #33807, .F. ) ;
#40277 = CYLINDRICAL_SURFACE ( 'NONE', #7527, 20.00000000000000355 ) ;
#40278 = CARTESIAN_POINT ( 'NONE',  ( 0.000000000000000000, 0.000000000000000000, 0.000000000000000000 ) ) ;
#40280 = CARTESIAN_POINT ( 'NONE',  ( 74.15939217261870908, 31.00000000000000000, -19.75058139460982432 ) ) ;
#40279 = AXIS2_PLACEMENT_3D ( 'NONE', #22641, #5798, #16083 ) ;
#40281 = CARTESIAN_POINT ( 'NONE',  ( -81.90010630563853056, 40.00000000000000711, 5.248159452637418454 ) ) ;
#40282 = DIRECTION ( 'NONE',  ( -1.000000000000000000, 0.000000000000000000, 0.000000000000000000 ) ) ;
#40283 = EDGE_LOOP ( 'NONE', ( #14599, #8492, #15109, #29833 ) ) ;
#40284 = CARTESIAN_POINT ( 'NONE',  ( 0.000000000000000000, 0.000000000000000000, -25.00000000000000000 ) ) ;
#40285 = VERTEX_POINT ( 'NONE', #3921 ) ;
#40286 = LINE ( 'NONE', #27666, #22128 ) ;
#40287 = CARTESIAN_POINT ( 'NONE',  ( -4.000000000000000000, 2.309401076758498483, -3.433295621305379353 ) ) ;
#40289 = ORIENTED_EDGE ( 'NONE', *, *, #31413, .T. ) ;
#40288 = DIRECTION ( 'NONE',  ( 1.000000000000000000, -0.000000000000000000, -0.000000000000000000 ) ) ;
#40290 = DIRECTION ( 'NONE',  ( 0.000000000000000000, 0.000000000000000000, 1.000000000000000000 ) ) ;
#40291 = ORIENTED_EDGE ( 'NONE', *, *, #2638, .T. ) ;
#40292 = CARTESIAN_POINT ( 'NONE',  ( 18.00000000000000355, 0.000000000000000000, 0.000000000000000000 ) ) ;
#40293 = CARTESIAN_POINT ( 'NONE',  ( -26.42126989340051324, 40.00000000000000000, -77.78956226056263290 ) ) ;
#40294 = CARTESIAN_POINT ( 'NONE',  ( 17.99999999999999645, -52.19040376560500505, 99.31985817764160629 ) ) ;
#40295 = ORIENTED_EDGE ( 'NONE', *, *, #1644, .F. ) ;
#40296 = CARTESIAN_POINT ( 'NONE',  ( 0.000000000000000000, 0.000000000000000000, 0.000000000000000000 ) ) ;
#40297 = CIRCLE ( 'NONE', #43071, 116.0000000000000000 ) ;
#40298 = DIRECTION ( 'NONE',  ( -1.000000000000000000, 0.000000000000000000, 0.000000000000000000 ) ) ;
#40299 = AXIS2_PLACEMENT_3D ( 'NONE', #37885, #18103, #40505 ) ;
#40300 = ADVANCED_FACE ( 'NONE', ( #20795 ), #34052, .F. ) ;
#40301 = VERTEX_POINT ( 'NONE', #26441 ) ;
#40302 = AXIS2_PLACEMENT_3D ( 'NONE', #24788, #18046, #1176 ) ;
#40303 = ADVANCED_FACE ( 'NONE', ( #23192 ), #20145, .T. ) ;
#40304 = CARTESIAN_POINT ( 'NONE',  ( 18.00000000000000355, 8.053585752062561554, -46.81126742072013514 ) ) ;
#40305 = VERTEX_POINT ( 'NONE', #11370 ) ;
#40306 = CARTESIAN_POINT ( 'NONE',  ( 0.000000000000000000, 18.35539002514383711, 110.6858262410710410 ) ) ;
#40307 = ORIENTED_EDGE ( 'NONE', *, *, #24164, .T. ) ;
#40308 = CARTESIAN_POINT ( 'NONE',  ( 22.27703560431449148, 40.00000000000000000, 17.12883495622503816 ) ) ;
#40309 = DIRECTION ( 'NONE',  ( -1.000000000000000000, -0.000000000000000000, -0.000000000000000000 ) ) ;
#40310 = CYLINDRICAL_SURFACE ( 'NONE', #9466, 47.49900000000000233 ) ;
#40311 = DIRECTION ( 'NONE',  ( -1.000000000000000000, 0.000000000000000000, -0.000000000000000000 ) ) ;
#40312 = DIRECTION ( 'NONE',  ( 1.000000000000000000, 0.000000000000000000, 0.000000000000000000 ) ) ;
#40313 = VERTEX_POINT ( 'NONE', #24490 ) ;
#40315 = DIRECTION ( 'NONE',  ( 0.000000000000000000, 0.2631025642275217069, -0.9647678688145158166 ) ) ;
#40314 = CARTESIAN_POINT ( 'NONE',  ( 0.000000000000000000, 42.41764978026607480, -20.20639853260305685 ) ) ;
#40316 = ADVANCED_FACE ( 'NONE', ( #1739 ), #8509, .F. ) ;
#40317 = ORIENTED_EDGE ( 'NONE', *, *, #14801, .F. ) ;
#40318 = CARTESIAN_POINT ( 'NONE',  ( -19.99999999999999645, 31.00000000000000355, -7.355690625810191807E-15 ) ) ;
#40319 = EDGE_CURVE ( 'NONE', #959, #35337, #92, .T. ) ;
#40320 = CARTESIAN_POINT ( 'NONE',  ( 0.000000000000000000, 5.871425383722279179, -51.66745943012274722 ) ) ;
#40321 = ORIENTED_EDGE ( 'NONE', *, *, #14758, .T. ) ;
#40322 = CYLINDRICAL_SURFACE ( 'NONE', #6452, 20.00000000000001066 ) ;
#40323 = CARTESIAN_POINT ( 'NONE',  ( -3.999999999999999112, 1.539600717838996324, -3.300726591567078039 ) ) ;
#40324 = CONTEXT_DEPENDENT_SHAPE_REPRESENTATION ( #37033, #25589 ) ;
#40325 = CARTESIAN_POINT ( 'NONE',  ( 17.99999999999999645, -72.00556975657644898, -86.04342158279462183 ) ) ;
#40326 = CARTESIAN_POINT ( 'NONE',  ( 17.40022565512299479, 31.00000000000000355, 64.93645345284011228 ) ) ;
#40327 = AXIS2_PLACEMENT_3D ( 'NONE', #13889, #299, #36534 ) ;
#40328 = ORIENTED_EDGE ( 'NONE', *, *, #34593, .F. ) ;
#40329 = CIRCLE ( 'NONE', #11792, 52.00000000000000000 ) ;
#40330 = CARTESIAN_POINT ( 'NONE',  ( 21.53706125532763593, 31.00000000000000355, 43.87245753946415761 ) ) ;
#40331 = CARTESIAN_POINT ( 'NONE',  ( 5.072363130230502115, 40.00000000000000000, 77.39583333421907696 ) ) ;
#40332 = AXIS2_PLACEMENT_3D ( 'NONE', #39054, #22320, #5691 ) ;
#40333 = ADVANCED_FACE ( 'NONE', ( #37743 ), #4812, .F. ) ;
#40334 = CARTESIAN_POINT ( 'NONE',  ( 0.000000000000000000, -73.51007459736368332, -89.73443560133438268 ) ) ;
#40335 = CARTESIAN_POINT ( 'NONE',  ( 18.00000000000000355, -3.840921266749491192, -47.34345070675175293 ) ) ;
#40336 = EDGE_CURVE ( 'NONE', #19113, #35135, #37958, .T. ) ;
#40337 = ORIENTED_EDGE ( 'NONE', *, *, #28452, .F. ) ;
#40338 = DIRECTION ( 'NONE',  ( 0.000000000000000000, -0.7164567402983210709, 0.6976315211349786161 ) ) ;
#40339 = DIRECTION ( 'NONE',  ( 0.000000000000000000, 0.000000000000000000, 1.000000000000000000 ) ) ;
#40340 = VERTEX_POINT ( 'NONE', #24700 ) ;
#40341 = CARTESIAN_POINT ( 'NONE',  ( -51.34291522965900612, 40.00000000000000000, 29.65708359768123970 ) ) ;
#40342 = DIRECTION ( 'NONE',  ( -1.000000000000000000, -0.000000000000000000, 0.000000000000000000 ) ) ;
#40343 = DIRECTION ( 'NONE',  ( 0.000000000000000000, -1.000000000000000000, 0.000000000000000000 ) ) ;
#40344 = EDGE_LOOP ( 'NONE', ( #36515, #6555, #5695, #3720 ) ) ;
#40345 = CARTESIAN_POINT ( 'NONE',  ( 0.000000000000000000, -38.92705108641749945, 27.21837053747784552 ) ) ;
#40346 = CYLINDRICAL_SURFACE ( 'NONE', #21571, 59.00000000000000000 ) ;
#40347 = VERTEX_POINT ( 'NONE', #1314 ) ;
#40348 = FACE_OUTER_BOUND ( 'NONE', #5589, .T. ) ;
#40349 = ORIENTED_EDGE ( 'NONE', *, *, #33087, .T. ) ;
#40350 = ADVANCED_FACE ( 'NONE', ( #41673, #14660 ), #8081, .T. ) ;
#40351 = DIRECTION ( 'NONE',  ( -1.000000000000000000, -0.000000000000000000, 0.000000000000000000 ) ) ;
#40353 = ORIENTED_EDGE ( 'NONE', *, *, #1113, .F. ) ;
#40352 = AXIS2_PLACEMENT_3D ( 'NONE', #18971, #35063, #32228 ) ;
#40354 = DIRECTION ( 'NONE',  ( 0.000000000000000000, 0.000000000000000000, 1.000000000000000000 ) ) ;
#40355 = CARTESIAN_POINT ( 'NONE',  ( 12.87762912550514827, 31.00000000000000355, 98.66289914823325091 ) ) ;
#40356 = ORIENTED_EDGE ( 'NONE', *, *, #10593, .F. ) ;
#40357 = DIRECTION ( 'NONE',  ( -1.000000000000000000, -0.000000000000000000, -0.000000000000000000 ) ) ;
#40358 = CIRCLE ( 'NONE', #22296, 116.0000000000000000 ) ;
#40359 = CIRCLE ( 'NONE', #20901, 116.0000000000000000 ) ;
#40360 = DIRECTION ( 'NONE',  ( 0.000000000000000000, 0.5264321628773568351, -0.8502171357296134380 ) ) ;
#40361 = CARTESIAN_POINT ( 'NONE',  ( 17.99999999999999645, 111.7974656912330005, 9.465682155095883843 ) ) ;
#40362 = AXIS2_PLACEMENT_3D ( 'NONE', #33384, #2816, #9618 ) ;
#40363 = ORIENTED_EDGE ( 'NONE', *, *, #38884, .F. ) ;
#40364 = DIRECTION ( 'NONE',  ( -1.000000000000000000, -0.000000000000000000, -0.000000000000000000 ) ) ;
#40365 = ADVANCED_FACE ( 'NONE', ( #25142 ), #21449, .T. ) ;
#40366 = DIRECTION ( 'NONE',  ( 0.000000000000000000, 0.000000000000000000, 1.000000000000000000 ) ) ;
#40367 = EDGE_CURVE ( 'NONE', #19368, #29604, #34699, .T. ) ;
#40369 = DIRECTION ( 'NONE',  ( -1.000000000000000000, -0.000000000000000000, 0.000000000000000000 ) ) ;
#40368 = CARTESIAN_POINT ( 'NONE',  ( 0.000000000000000000, 0.000000000000000000, 0.000000000000000000 ) ) ;
#40370 = DIRECTION ( 'NONE',  ( -1.000000000000000000, 0.000000000000000000, 0.000000000000000000 ) ) ;
#40371 = EDGE_LOOP ( 'NONE', ( #13612, #42602 ) ) ;
#40372 = DIRECTION ( 'NONE',  ( -6.123233995736766036E-17, 1.000000000000000000, 4.275831445896958607E-31 ) ) ;
#40373 = CARTESIAN_POINT ( 'NONE',  ( -17.77999999999999758, 0.000000000000000000, 0.000000000000000000 ) ) ;
#40374 = CARTESIAN_POINT ( 'NONE',  ( -12.24460912605626106, 31.00000000000000355, 36.08157028455360660 ) ) ;
#40375 = VERTEX_POINT ( 'NONE', #17955 ) ;
#40376 = CARTESIAN_POINT ( 'NONE',  ( -150.4999999999986926, -2.921102061156358310E-13, 10.00000000000004441 ) ) ;
#40377 = FACE_OUTER_BOUND ( 'NONE', #2392, .T. ) ;
#40378 = VERTEX_POINT ( 'NONE', #14872 ) ;
#40379 = CARTESIAN_POINT ( 'NONE',  ( 17.99999999999999645, 25.52601536738619714, -19.21447964122670626 ) ) ;
#40380 = CARTESIAN_POINT ( 'NONE',  ( 43.19851606872948935, 40.00000000000000000, 14.66122656362567689 ) ) ;
#40381 = CARTESIAN_POINT ( 'NONE',  ( -34.17541447290003020, 40.00000000000000000, -26.31327426976606887 ) ) ;
#40382 = AXIS2_PLACEMENT_3D ( 'NONE', #32438, #25094, #38972 ) ;
#40383 = ORIENTED_EDGE ( 'NONE', *, *, #14270, .F. ) ;
#40384 = LINE ( 'NONE', #10520, #22835 ) ;
#40385 = DIRECTION ( 'NONE',  ( 0.000000000000000000, 0.000000000000000000, 1.000000000000000000 ) ) ;
#40387 = EDGE_CURVE ( 'NONE', #31578, #27751, #8511, .T. ) ;
#40386 = CIRCLE ( 'NONE', #7670, 13.59999999999999964 ) ;
#40388 = ADVANCED_FACE ( 'NONE', ( #30787 ), #11817, .T. ) ;
#40389 = CARTESIAN_POINT ( 'NONE',  ( 9.000000000000001776, 35.11945359308163717, -38.34871548465978464 ) ) ;
#40390 = ORIENTED_EDGE ( 'NONE', *, *, #37568, .T. ) ;
#40391 = CARTESIAN_POINT ( 'NONE',  ( -17.40445659762299968, 40.00000000000000000, 22.69748452323785060 ) ) ;
#40392 = ORIENTED_EDGE ( 'NONE', *, *, #26401, .F. ) ;
#40393 = DIRECTION ( 'NONE',  ( 0.000000000000000000, 0.000000000000000000, 1.000000000000000000 ) ) ;
#40394 = DIRECTION ( 'NONE',  ( 0.000000000000000000, -0.4817536741017223179, 0.8763066800438598092 ) ) ;
#40395 = ORIENTED_EDGE ( 'NONE', *, *, #32026, .T. ) ;
#40396 = CARTESIAN_POINT ( 'NONE',  ( 17.99999999999999645, 16.86122981692017930, 27.13802899033298388 ) ) ;
#40397 = DIRECTION ( 'NONE',  ( 1.000000000000000000, -0.000000000000000000, 0.000000000000000000 ) ) ;
#40398 = EDGE_LOOP ( 'NONE', ( #9309, #13664, #18092, #17204 ) ) ;
#40399 = CARTESIAN_POINT ( 'NONE',  ( -99.91857577502598531, 17.11489954122026447, -1.280628618496984839 ) ) ;
#40400 = ORIENTED_EDGE ( 'NONE', *, *, #7050, .T. ) ;
#40401 = CARTESIAN_POINT ( 'NONE',  ( 2.500000000000000000, 2.629050547790028946E-15, 2.042000000000000259 ) ) ;
#40402 = ADVANCED_FACE ( 'NONE', ( #34260 ), #8301, .F. ) ;
#40403 = EDGE_CURVE ( 'NONE', #17987, #19733, #21660, .T. ) ;
#40404 = ORIENTED_EDGE ( 'NONE', *, *, #38606, .T. ) ;
#40406 = ORIENTED_EDGE ( 'NONE', *, *, #4703, .T. ) ;
#40405 = DIRECTION ( 'NONE',  ( 1.000000000000000000, 0.000000000000000000, 0.000000000000000000 ) ) ;
#40407 = CARTESIAN_POINT ( 'NONE',  ( 4.329677741076777053, 31.00000000000000355, -64.59417075179258916 ) ) ;
#40408 = EDGE_LOOP ( 'NONE', ( #20172, #6679, #11893, #30177 ) ) ;
#40409 = CARTESIAN_POINT ( 'NONE',  ( -132.0000507999999968, 0.000000000000000000, 0.000000000000000000 ) ) ;
#40410 = ORIENTED_EDGE ( 'NONE', *, *, #38798, .F. ) ;
#40411 = CARTESIAN_POINT ( 'NONE',  ( 17.99999999999999645, 25.18647942089895153, -113.2326863338525271 ) ) ;
#40412 = ADVANCED_FACE ( 'NONE', ( #40790 ), #34913, .F. ) ;
#40413 = ORIENTED_EDGE ( 'NONE', *, *, #11040, .T. ) ;
#40414 = CARTESIAN_POINT ( 'NONE',  ( -65.95487968126425926, 40.00000000000000711, -50.74205456615700882 ) ) ;
#40415 = AXIS2_PLACEMENT_3D ( 'NONE', #17698, #20767, #34026 ) ;
#40416 = AXIS2_PLACEMENT_3D ( 'NONE', #30037, #34146, #3583 ) ;
#40417 = EDGE_CURVE ( 'NONE', #23271, #26141, #27334, .T. ) ;
#40418 = AXIS2_PLACEMENT_3D ( 'NONE', #2578, #2351, #41874 ) ;
#40420 = DIRECTION ( 'NONE',  ( 1.000000000000000000, 0.000000000000000000, 0.000000000000000000 ) ) ;
#40419 = LINE ( 'NONE', #24336, #32842 ) ;
#40421 = VECTOR ( 'NONE', #24909, 1000.000000000000000 ) ;
#40422 = DIRECTION ( 'NONE',  ( 1.000000000000000000, 0.000000000000000000, -0.000000000000000000 ) ) ;
#40423 = ORIENTED_EDGE ( 'NONE', *, *, #6733, .T. ) ;
#40424 = DIRECTION ( 'NONE',  ( -1.000000000000000000, -0.000000000000000000, -0.000000000000000000 ) ) ;
#40425 = ORIENTED_EDGE ( 'NONE', *, *, #38912, .F. ) ;
#40426 = DIRECTION ( 'NONE',  ( 0.000000000000000000, 0.4610925014493206242, 0.8873520750565743187 ) ) ;
#40427 = LINE ( 'NONE', #37595, #34449 ) ;
#40428 = CARTESIAN_POINT ( 'NONE',  ( -66.93673649651354651, 31.00000000000000711, 58.72203107584222437 ) ) ;
#40429 = DIRECTION ( 'NONE',  ( -3.009274222672345096E-17, -1.000000000000000000, 2.455023325076454960E-18 ) ) ;
#40430 = EDGE_LOOP ( 'NONE', ( #1535, #15929 ) ) ;
#40431 = DIRECTION ( 'NONE',  ( 1.000000000000000000, 0.000000000000000000, 0.000000000000000000 ) ) ;
#40432 = EDGE_CURVE ( 'NONE', #28925, #34983, #34473, .T. ) ;
#40433 = AXIS2_PLACEMENT_3D ( 'NONE', #12879, #6954, #29675 ) ;
#40434 = ORIENTED_EDGE ( 'NONE', *, *, #27130, .T. ) ;
#40435 = DIRECTION ( 'NONE',  ( -1.000000000000000000, 0.000000000000000000, 0.000000000000000000 ) ) ;
#40436 = DIRECTION ( 'NONE',  ( -1.000000000000000000, -0.000000000000000000, 0.000000000000000000 ) ) ;
#40437 = EDGE_CURVE ( 'NONE', #36312, #40855, #23181, .T. ) ;
#40438 = ADVANCED_FACE ( 'NONE', ( #19443 ), #34262, .T. ) ;
#40439 = ADVANCED_FACE ( 'NONE', ( #32078 ), #32707, .F. ) ;
#40440 = CARTESIAN_POINT ( 'NONE',  ( 17.99999999999999645, -105.7179949885865256, -37.57629584241794163 ) ) ;
#40441 = CIRCLE ( 'NONE', #13300, 47.49899999999999523 ) ;
#40442 = ORIENTED_EDGE ( 'NONE', *, *, #21797, .F. ) ;
#40443 = DIRECTION ( 'NONE',  ( -1.000000000000000000, -0.000000000000000000, 0.000000000000000000 ) ) ;
#40444 = ORIENTED_EDGE ( 'NONE', *, *, #31388, .F. ) ;
#40445 = VECTOR ( 'NONE', #17616, 1000.000000000000000 ) ;
#40446 = DIRECTION ( 'NONE',  ( -0.000000000000000000, -0.000000000000000000, 1.000000000000000000 ) ) ;
#40447 = VECTOR ( 'NONE', #3324, 999.9999999999998863 ) ;
#40448 = AXIS2_PLACEMENT_3D ( 'NONE', #10884, #31381, #4085 ) ;
#40449 = CARTESIAN_POINT ( 'NONE',  ( 0.000000000000000000, -5.822172717930031993, -31.41458249383147106 ) ) ;
#40450 = CIRCLE ( 'NONE', #2810, 59.00000000000000000 ) ;
#40451 = DIRECTION ( 'NONE',  ( 0.000000000000000000, 0.000000000000000000, 1.000000000000000000 ) ) ;
#40452 = ORIENTED_EDGE ( 'NONE', *, *, #9139, .T. ) ;
#40453 = ORIENTED_EDGE ( 'NONE', *, *, #28716, .T. ) ;
#40454 = CYLINDRICAL_SURFACE ( 'NONE', #10545, 116.0000000000000000 ) ;
#40455 = CARTESIAN_POINT ( 'NONE',  ( 17.99999999999999645, 107.2703412112694963, 32.88383143828500721 ) ) ;
#40456 = DIRECTION ( 'NONE',  ( -1.000000000000000000, 0.000000000000000000, 0.000000000000000000 ) ) ;
#40457 = CIRCLE ( 'NONE', #16115, 13.60000000000000320 ) ;
#40459 = ORIENTED_EDGE ( 'NONE', *, *, #36695, .F. ) ;
#40458 = CARTESIAN_POINT ( 'NONE',  ( 0.000000000000000000, 0.000000000000000000, 0.000000000000000000 ) ) ;
#40460 = CARTESIAN_POINT ( 'NONE',  ( -15.23573235977617379, 31.00000000000000355, 26.30445775087292404 ) ) ;
#40461 = DIRECTION ( 'NONE',  ( 0.000000000000000000, 0.000000000000000000, 1.000000000000000000 ) ) ;
#40463 = EDGE_LOOP ( 'NONE', ( #18673, #163, #33004, #12796 ) ) ;
#40462 = CARTESIAN_POINT ( 'NONE',  ( 17.99999999999999645, -111.2721026680461733, 14.38025178762581469 ) ) ;
#40464 = VERTEX_POINT ( 'NONE', #25770 ) ;
#40465 = CARTESIAN_POINT ( 'NONE',  ( 17.99999999999999645, -31.11570115861498920, 4.898994019976531611 ) ) ;
#40466 = CARTESIAN_POINT ( 'NONE',  ( -39.97893566998936876, 40.00000000000000000, -35.18630237794886995 ) ) ;
#40467 = EDGE_CURVE ( 'NONE', #33268, #18842, #33527, .T. ) ;
#40468 = CARTESIAN_POINT ( 'NONE',  ( 18.00000000000000355, 39.78933988720149273, -24.98727647984960498 ) ) ;
#40469 = CARTESIAN_POINT ( 'NONE',  ( 0.000000000000000000, -46.12538073176274622, -111.3235835452215952 ) ) ;
#40470 = ORIENTED_EDGE ( 'NONE', *, *, #829, .F. ) ;
#40471 = DIRECTION ( 'NONE',  ( 0.000000000000000000, 0.000000000000000000, 1.000000000000000000 ) ) ;
#40472 = ORIENTED_EDGE ( 'NONE', *, *, #21375, .F. ) ;
#40473 = AXIS2_PLACEMENT_3D ( 'NONE', #41771, #28062, #14977 ) ;
#40474 = DIRECTION ( 'NONE',  ( 0.000000000000000000, 0.000000000000000000, 1.000000000000000000 ) ) ;
#40475 = CYLINDRICAL_SURFACE ( 'NONE', #42860, 120.5010000000000190 ) ;
#40476 = AXIS2_PLACEMENT_3D ( 'NONE', #12494, #28649, #32322 ) ;
#40477 = CARTESIAN_POINT ( 'NONE',  ( 25.16436199730139123, 31.00000000000000355, 51.02488717759543135 ) ) ;
#40478 = LINE ( 'NONE', #10172, #38529 ) ;
#40479 = ORIENTED_EDGE ( 'NONE', *, *, #40934, .T. ) ;
#40480 = CIRCLE ( 'NONE', #24511, 120.5010000000000190 ) ;
#40481 = DIRECTION ( 'NONE',  ( 1.000000000000000000, 0.000000000000000000, -0.000000000000000000 ) ) ;
#40482 = VERTEX_POINT ( 'NONE', #6094 ) ;
#40483 = CARTESIAN_POINT ( 'NONE',  ( 42.89041025189590783, 31.00000000000000355, 86.97820559439793442 ) ) ;
#40484 = AXIS2_PLACEMENT_3D ( 'NONE', #34211, #37905, #34421 ) ;
#40485 = ORIENTED_EDGE ( 'NONE', *, *, #13653, .F. ) ;
#40486 = CARTESIAN_POINT ( 'NONE',  ( 9.000000000000001776, -29.86146781000025285, 112.0905559814577970 ) ) ;
#40487 = LINE ( 'NONE', #780, #37324 ) ;
#40488 = CARTESIAN_POINT ( 'NONE',  ( 5.085823974618866039, 31.00000000000000355, 79.40009828669005287 ) ) ;
#40489 = CARTESIAN_POINT ( 'NONE',  ( -65.32047834219908111, 40.00000000000000711, -32.32491738442255524 ) ) ;
#40490 = EDGE_CURVE ( 'NONE', #6927, #24346, #45, .T. ) ;
#40491 = ADVANCED_FACE ( 'NONE', ( #22293 ), #28815, .T. ) ;
#40492 = FACE_OUTER_BOUND ( 'NONE', #40009, .T. ) ;
#40493 = EDGE_CURVE ( 'NONE', #9120, #17669, #39230, .T. ) ;
#40494 = VERTEX_POINT ( 'NONE', #28609 ) ;
#40495 = CARTESIAN_POINT ( 'NONE',  ( 0.000000000000000000, 46.83041522348496954, 101.9567785075603155 ) ) ;
#40496 = VERTEX_POINT ( 'NONE', #29031 ) ;
#40497 = LINE ( 'NONE', #1658, #41573 ) ;
#40498 = FACE_OUTER_BOUND ( 'NONE', #35797, .T. ) ;
#40500 = ORIENTED_EDGE ( 'NONE', *, *, #19004, .F. ) ;
#40499 = CARTESIAN_POINT ( 'NONE',  ( 0.000000000000000000, -1.178949249685214307, 2.042000000000001592 ) ) ;
#40501 = CARTESIAN_POINT ( 'NONE',  ( 0.000000000000000000, 5.871425383721554425, 51.66745943012284670 ) ) ;
#40502 = VERTEX_POINT ( 'NONE', #1958 ) ;
#40503 = DIRECTION ( 'NONE',  ( 0.000000000000000000, 0.000000000000000000, 1.000000000000000000 ) ) ;
#40504 = CARTESIAN_POINT ( 'NONE',  ( -80.23695839127151430, 40.00000000000000711, 39.56677620416681407 ) ) ;
#40505 = DIRECTION ( 'NONE',  ( 0.000000000000000000, -0.3681245526846854133, 0.9297764858882485717 ) ) ;
#40506 = CIRCLE ( 'NONE', #7066, 0.5155456020628804703 ) ;
#40507 = VECTOR ( 'NONE', #15032, 1000.000000000000000 ) ;
#40508 = VERTEX_POINT ( 'NONE', #12234 ) ;
#40509 = EDGE_CURVE ( 'NONE', #36319, #15350, #12028, .T. ) ;
#40510 = CARTESIAN_POINT ( 'NONE',  ( 4.121423858225410797, -12.61643262889541006, -1.199999999999999956 ) ) ;
#40511 = DIRECTION ( 'NONE',  ( 0.000000000000000000, 0.000000000000000000, 1.000000000000000000 ) ) ;
#40512 = AXIS2_PLACEMENT_3D ( 'NONE', #14534, #37618, #14305 ) ;
#40513 = ORIENTED_EDGE ( 'NONE', *, *, #11378, .T. ) ;
#40514 = CYLINDRICAL_SURFACE ( 'NONE', #42072, 125.9999999999993605 ) ;
#40515 = VERTEX_POINT ( 'NONE', #5867 ) ;
#40516 = DIRECTION ( 'NONE',  ( 0.000000000000000000, 0.000000000000000000, 1.000000000000000000 ) ) ;
#40517 = ORIENTED_EDGE ( 'NONE', *, *, #8687, .T. ) ;
#40519 = CARTESIAN_POINT ( 'NONE',  ( -22.06642698273767067, 40.00000000000000000, -2.901557744773887393 ) ) ;
#40518 = VECTOR ( 'NONE', #38874, 1000.000000000000000 ) ;
#40520 = CARTESIAN_POINT ( 'NONE',  ( 0.000000000000000000, -44.25018368420722936, -27.31155879685226395 ) ) ;
#40521 = CARTESIAN_POINT ( 'NONE',  ( 0.000000000000000000, -27.83061035786878890, -117.2431154827800270 ) ) ;
#40522 = DIRECTION ( 'NONE',  ( 1.000000000000000000, -1.373900992973642460E-15, -3.469446951953632924E-16 ) ) ;
#40523 = EDGE_LOOP ( 'NONE', ( #28954, #15450, #18072, #33867 ) ) ;
#40525 = DIRECTION ( 'NONE',  ( 1.000000000000000000, 0.000000000000000000, 0.000000000000000000 ) ) ;
#40524 = DIRECTION ( 'NONE',  ( -1.000000000000000000, -0.000000000000000000, 0.000000000000000000 ) ) ;
#40526 = ORIENTED_EDGE ( 'NONE', *, *, #29956, .F. ) ;
#40527 = CARTESIAN_POINT ( 'NONE',  ( 17.99999999999999645, 64.58410930313523579, 101.7319213743684685 ) ) ;
#40528 = CARTESIAN_POINT ( 'NONE',  ( -17.40445659762299968, 31.00000000000000355, 22.69748452323785060 ) ) ;
#40529 = ORIENTED_EDGE ( 'NONE', *, *, #5658, .F. ) ;
#40530 = FACE_OUTER_BOUND ( 'NONE', #22529, .T. ) ;
#40531 = LINE ( 'NONE', #27704, #2131 ) ;
#40532 = DIRECTION ( 'NONE',  ( -1.000000000000000000, 0.000000000000000000, 0.000000000000000000 ) ) ;
#40533 = VECTOR ( 'NONE', #25971, 1000.000000000000000 ) ;
#40534 = CARTESIAN_POINT ( 'NONE',  ( 32.44529481510334534, 31.00000000000000355, -65.82339768528792945 ) ) ;
#40535 = AXIS2_PLACEMENT_3D ( 'NONE', #30998, #41221, #27519 ) ;
#40536 = AXIS2_PLACEMENT_3D ( 'NONE', #14036, #20825, #27121 ) ;
#40537 = ORIENTED_EDGE ( 'NONE', *, *, #11125, .F. ) ;
#40538 = CARTESIAN_POINT ( 'NONE',  ( 36.21668514974006570, 31.00000000000000355, 31.87730689759005287 ) ) ;
#40539 = AXIS2_PLACEMENT_3D ( 'NONE', #12646, #19852, #22489 ) ;
#40540 = EDGE_CURVE ( 'NONE', #11261, #21531, #1475, .T. ) ;
#40541 = CARTESIAN_POINT ( 'NONE',  ( -10.77850749866037816, 40.00000000000000000, -81.75987728344749428 ) ) ;
#40542 = CIRCLE ( 'NONE', #9202, 59.00000000000000000 ) ;
#40543 = CARTESIAN_POINT ( 'NONE',  ( 0.000000000000000000, -94.52951811191513798, -67.23221107124996365 ) ) ;
#40544 = DIRECTION ( 'NONE',  ( -1.000000000000000000, -0.000000000000000000, -0.000000000000000000 ) ) ;
#40545 = CARTESIAN_POINT ( 'NONE',  ( 17.99999999999999645, 0.000000000000000000, 0.000000000000000000 ) ) ;
#40546 = EDGE_CURVE ( 'NONE', #32806, #39315, #23815, .T. ) ;
#40547 = ORIENTED_EDGE ( 'NONE', *, *, #23162, .F. ) ;
#40548 = DIRECTION ( 'NONE',  ( 0.000000000000000000, -0.8477344278896650209, -0.5304209081197521769 ) ) ;
#40549 = CARTESIAN_POINT ( 'NONE',  ( -4.211140560182196957, -2.431303136016552013, -3.745885042887436178 ) ) ;
#40550 = EDGE_CURVE ( 'NONE', #20273, #27122, #41879, .T. ) ;
#40551 = ORIENTED_EDGE ( 'NONE', *, *, #30393, .T. ) ;
#40552 = CARTESIAN_POINT ( 'NONE',  ( 32.65420139560029611, 40.00000000000000000, -42.57517516360295673 ) ) ;
#40553 = DIRECTION ( 'NONE',  ( 0.000000000000000000, 0.000000000000000000, 1.000000000000000000 ) ) ;
#40554 = DIRECTION ( 'NONE',  ( 0.000000000000000000, 0.000000000000000000, 1.000000000000000000 ) ) ;
#40555 = EDGE_LOOP ( 'NONE', ( #18322, #33522, #38976, #39635 ) ) ;
#40556 = ADVANCED_FACE ( 'NONE', ( #15319 ), #25347, .T. ) ;
#40557 = DIRECTION ( 'NONE',  ( -1.000000000000000000, 0.000000000000000000, -0.000000000000000000 ) ) ;
#40558 = FACE_OUTER_BOUND ( 'NONE', #22413, .T. ) ;
#40559 = ORIENTED_EDGE ( 'NONE', *, *, #21357, .T. ) ;
#40560 = CARTESIAN_POINT ( 'NONE',  ( 0.000000000000000000, 59.07817985939001915, 105.0250430397510968 ) ) ;
#40561 = VERTEX_POINT ( 'NONE', #32496 ) ;
#40562 = AXIS2_PLACEMENT_3D ( 'NONE', #27919, #37910, #38347 ) ;
#40563 = LINE ( 'NONE', #21439, #3692 ) ;
#40564 = VERTEX_POINT ( 'NONE', #38598 ) ;
#40565 = LINE ( 'NONE', #10702, #7700 ) ;
#40566 = VECTOR ( 'NONE', #19617, 1000.000000000000000 ) ;
#40567 = CARTESIAN_POINT ( 'NONE',  ( 5.657435538624008755E-15, 4.615443851143735910E-16, 0.000000000000000000 ) ) ;
#40568 = ORIENTED_EDGE ( 'NONE', *, *, #28964, .T. ) ;
#40569 = CIRCLE ( 'NONE', #42684, 20.00000000000001066 ) ;
#40570 = DIRECTION ( 'NONE',  ( 0.000000000000000000, 1.000000000000000000, 0.000000000000000000 ) ) ;
#40571 = CYLINDRICAL_SURFACE ( 'NONE', #35212, 19.19999999999999574 ) ;
#40572 = EDGE_LOOP ( 'NONE', ( #12902, #30984, #38436, #5946 ) ) ;
#40573 = CARTESIAN_POINT ( 'NONE',  ( 0.000000000000000000, 0.000000000000000000, 0.000000000000000000 ) ) ;
#40574 = EDGE_CURVE ( 'NONE', #40561, #2965, #25204, .T. ) ;
#40575 = CIRCLE ( 'NONE', #5742, 51.99999999999999289 ) ;
#40576 = DIRECTION ( 'NONE',  ( 0.000000000000000000, 0.6736956436465532105, 0.7390089172206627532 ) ) ;
#40577 = DIRECTION ( 'NONE',  ( -0.000000000000000000, -0.000000000000000000, 1.000000000000000000 ) ) ;
#40578 = LINE ( 'NONE', #37541, #1231 ) ;
#40579 = ORIENTED_EDGE ( 'NONE', *, *, #3636, .F. ) ;
#40580 = CARTESIAN_POINT ( 'NONE',  ( 36.42574649280186350, 1.212214612624460644E-26, -75.69124779287314198 ) ) ;
#40581 = DIRECTION ( 'NONE',  ( 0.000000000000000000, -0.6845471059286792892, -0.7289686274214203232 ) ) ;
#40582 = CARTESIAN_POINT ( 'NONE',  ( 13.85568741775851542, 31.00000000000000355, -40.82620080729295609 ) ) ;
#40583 = ORIENTED_EDGE ( 'NONE', *, *, #16536, .T. ) ;
#40584 = DIRECTION ( 'NONE',  ( -1.000000000000000000, 0.000000000000000000, -0.000000000000000000 ) ) ;
#40585 = CARTESIAN_POINT ( 'NONE',  ( 0.000000000000000000, 0.000000000000000000, -4.000000000000000000 ) ) ;
#40586 = ORIENTED_EDGE ( 'NONE', *, *, #2149, .T. ) ;
#40587 = CYLINDRICAL_SURFACE ( 'NONE', #30366, 59.00000000000000000 ) ;
#40588 = CARTESIAN_POINT ( 'NONE',  ( -44.28363997456384737, 40.00000000000000000, 21.84072794957603492 ) ) ;
#40589 = EDGE_CURVE ( 'NONE', #11369, #27530, #22714, .T. ) ;
#40590 = CARTESIAN_POINT ( 'NONE',  ( -15.62887661519555493, 40.00000000000000000, 57.97203279869352599 ) ) ;
#40591 = VERTEX_POINT ( 'NONE', #39451 ) ;
#40592 = CYLINDRICAL_SURFACE ( 'NONE', #42242, 11.00000000000023448 ) ;
#40593 = CARTESIAN_POINT ( 'NONE',  ( 17.99999999999999645, 74.56001736500736854, -88.86396238368961065 ) ) ;
#40594 = CARTESIAN_POINT ( 'NONE',  ( -130.0000000000000000, 1.285559651900026877E-13, -40.00000000000004974 ) ) ;
#40595 = DIRECTION ( 'NONE',  ( 1.000000000000000000, 0.000000000000000000, 0.000000000000000000 ) ) ;
#40596 = EDGE_CURVE ( 'NONE', #35106, #30536, #11252, .T. ) ;
#40597 = ORIENTED_EDGE ( 'NONE', *, *, #29656, .T. ) ;
#40598 = CARTESIAN_POINT ( 'NONE',  ( 24.21999397792122366, 40.00000000000000000, 8.216913396989165008 ) ) ;
#40599 = ORIENTED_EDGE ( 'NONE', *, *, #13535, .F. ) ;
#40600 = CARTESIAN_POINT ( 'NONE',  ( 0.000000000000000000, 117.9424311864589185, 24.69967462999075991 ) ) ;
#40601 = CIRCLE ( 'NONE', #29487, 58.99999999999999289 ) ;
#40602 = CARTESIAN_POINT ( 'NONE',  ( -8.749793197483594298, -12.05525454449572464, 2.972870684497274762 ) ) ;
#40603 = ORIENTED_EDGE ( 'NONE', *, *, #32844, .F. ) ;
#40604 = DIRECTION ( 'NONE',  ( 1.000000000000000000, 0.000000000000000000, 0.000000000000000000 ) ) ;
#40605 = CARTESIAN_POINT ( 'NONE',  ( 18.00000000000000355, 42.60732521687599217, -19.80331771201614544 ) ) ;
#40606 = EDGE_LOOP ( 'NONE', ( #1338, #36585, #34651, #20860 ) ) ;
#40607 = DIRECTION ( 'NONE',  ( 0.000000000000000000, 0.9048270524660175784, 0.4257792915650767673 ) ) ;
#40608 = ORIENTED_EDGE ( 'NONE', *, *, #13791, .F. ) ;
#40609 = CARTESIAN_POINT ( 'NONE',  ( 17.99999999999999645, 6.486220790508443912, 112.0098273076987567 ) ) ;
#40610 = EDGE_LOOP ( 'NONE', ( #6547, #15554, #40832, #36522 ) ) ;
#40612 = ORIENTED_EDGE ( 'NONE', *, *, #42792, .T. ) ;
#40611 = CARTESIAN_POINT ( 'NONE',  ( 0.000000000000000000, -19.12429268481792732, 114.4126803693778669 ) ) ;
#40613 = CARTESIAN_POINT ( 'NONE',  ( 46.16409756963976463, 31.00000000000000355, -59.99419878592187416 ) ) ;
#40614 = ORIENTED_EDGE ( 'NONE', *, *, #5351, .F. ) ;
#40615 = DIRECTION ( 'NONE',  ( 3.009274222672345096E-17, 1.000000000000000000, -2.455023325076455345E-18 ) ) ;
#40616 = CIRCLE ( 'NONE', #22586, 36.00000000000000000 ) ;
#40617 = ORIENTED_EDGE ( 'NONE', *, *, #35614, .F. ) ;
#40618 = FACE_BOUND ( 'NONE', #23672, .T. ) ;
#40619 = EDGE_LOOP ( 'NONE', ( #19472, #24510, #19052, #518, #41313 ) ) ;
#40620 = AXIS2_PLACEMENT_3D ( 'NONE', #42961, #12477, #42533 ) ;
#40621 = CARTESIAN_POINT ( 'NONE',  ( 12.51314706078825090, 40.00000000000000000, -94.07914177280382262 ) ) ;
#40622 = EDGE_CURVE ( 'NONE', #37185, #1059, #29346, .T. ) ;
#40623 = EDGE_CURVE ( 'NONE', #23910, #14276, #36182, .T. ) ;
#40625 = DIRECTION ( 'NONE',  ( -1.000000000000000000, -0.000000000000000000, -0.000000000000000000 ) ) ;
#40624 = FACE_OUTER_BOUND ( 'NONE', #30880, .T. ) ;
#40626 = CARTESIAN_POINT ( 'NONE',  ( 18.00000000000000355, 0.000000000000000000, 0.000000000000000000 ) ) ;
#40627 = PLANE ( 'NONE',  #11740 ) ;
#40628 = MECHANICAL_DESIGN_GEOMETRIC_PRESENTATION_REPRESENTATION (  '', ( #6505 ), #33701 ) ;
#40629 = VERTEX_POINT ( 'NONE', #3867 ) ;
#40630 = SHAPE_DEFINITION_REPRESENTATION ( #10252, #330 ) ;
#40631 = CARTESIAN_POINT ( 'NONE',  ( 0.000000000000000000, -63.55543939553828636, 97.03971415477303708 ) ) ;
#40632 = STYLED_ITEM ( 'NONE', ( #6049 ), #42324 ) ;
#40633 = CARTESIAN_POINT ( 'NONE',  ( 6.004904395537136175, 0.000000000000000000, 0.000000000000000000 ) ) ;
#40634 = CARTESIAN_POINT ( 'NONE',  ( 50.95389515256417923, 31.00000000000000355, -66.42840393140320998 ) ) ;
#40635 = DIRECTION ( 'NONE',  ( 1.000000000000000000, 0.000000000000000000, 0.000000000000000000 ) ) ;
#40636 = EDGE_LOOP ( 'NONE', ( #14358, #1217, #18812, #7984 ) ) ;
#40637 = AXIS2_PLACEMENT_3D ( 'NONE', #1305, #27085, #638 ) ;
#40638 = EDGE_CURVE ( 'NONE', #252, #40190, #13341, .T. ) ;
#40639 = DIRECTION ( 'NONE',  ( -3.009274222672345096E-17, -1.000000000000000000, 2.455023325076454960E-18 ) ) ;
#40640 = EDGE_LOOP ( 'NONE', ( #11461, #22912, #30484, #35295 ) ) ;
#40641 = ORIENTED_EDGE ( 'NONE', *, *, #20669, .T. ) ;
#40642 = SURFACE_STYLE_FILL_AREA ( #27379 ) ;
#40643 = CIRCLE ( 'NONE', #1639, 116.0000000000000000 ) ;
#40644 = CARTESIAN_POINT ( 'NONE',  ( 0.000000000000000000, 0.000000000000000000, -25.03750572909317285 ) ) ;
#40645 = AXIS2_PLACEMENT_3D ( 'NONE', #9802, #22723, #26186 ) ;
#40646 = DIRECTION ( 'NONE',  ( 0.000000000000000000, 0.000000000000000000, 1.000000000000000000 ) ) ;
#40647 = B_SPLINE_CURVE_WITH_KNOTS ( 'NONE', 3,
 ( #29196, #2739, #32232, #28978, #19179, #6042, #40682, #7546 ),
 .UNSPECIFIED., .F., .F.,
 ( 4, 2, 2, 4 ),
 ( 2.465131517390770070E-07, 0.001183067374689869946, 0.001774477805458935659, 0.002365888236228001588 ),
 .UNSPECIFIED. ) ;
#40648 = ADVANCED_FACE ( 'NONE', ( #26606 ), #7156, .F. ) ;
#40649 = ORIENTED_EDGE ( 'NONE', *, *, #6217, .F. ) ;
#40650 = CARTESIAN_POINT ( 'NONE',  ( 18.00000000000000355, 0.000000000000000000, 0.000000000000000000 ) ) ;
#40651 = VERTEX_POINT ( 'NONE', #40089 ) ;
#40652 = DIRECTION ( 'NONE',  ( -1.000000000000000000, 0.000000000000000000, 0.000000000000000000 ) ) ;
#40653 = EDGE_CURVE ( 'NONE', #28377, #23473, #10658, .T. ) ;
#40654 = CARTESIAN_POINT ( 'NONE',  ( 18.00000000000000355, -51.19683565102437228, -9.104066087303984034 ) ) ;
#40655 = LINE ( 'NONE', #4678, #40023 ) ;
#40656 = ORIENTED_EDGE ( 'NONE', *, *, #5408, .F. ) ;
#40657 = EDGE_LOOP ( 'NONE', ( #2173, #16566 ) ) ;
#40658 = CARTESIAN_POINT ( 'NONE',  ( 17.99999999999999645, 0.000000000000000000, 0.000000000000000000 ) ) ;
#40659 = AXIS2_PLACEMENT_3D ( 'NONE', #31005, #17734, #1094 ) ;
#40660 = CARTESIAN_POINT ( 'NONE',  ( 17.99999999999999645, -110.8621702203446659, -34.14058016547651420 ) ) ;
#40661 = CARTESIAN_POINT ( 'NONE',  ( 4.000000000000000888, 0.8228435280416209752, -3.430609588141487976 ) ) ;
#40662 = AXIS2_PLACEMENT_3D ( 'NONE', #2066, #15844, #25460 ) ;
#40663 = ORIENTED_EDGE ( 'NONE', *, *, #41789, .T. ) ;
#40665 = ORIENTED_EDGE ( 'NONE', *, *, #36948, .F. ) ;
#40664 = CARTESIAN_POINT ( 'NONE',  ( 18.00000000000000355, -0.2227391519119825691, 46.98410307550729215 ) ) ;
#40666 = CARTESIAN_POINT ( 'NONE',  ( 41.46880187713386334, 31.00000000000000355, 24.04226233541373858 ) ) ;
#40667 = CARTESIAN_POINT ( 'NONE',  ( 47.55521504368574881, -2.055254544495723756, -70.64469547305695585 ) ) ;
#40668 = VECTOR ( 'NONE', #8294, 1000.000000000000000 ) ;
#40670 = ORIENTED_EDGE ( 'NONE', *, *, #7350, .T. ) ;
#40669 = CARTESIAN_POINT ( 'NONE',  ( 0.000000000000000000, -35.78425302087536863, -3.935382540233168580 ) ) ;
#40671 = ORIENTED_EDGE ( 'NONE', *, *, #1361, .F. ) ;
#40672 = CARTESIAN_POINT ( 'NONE',  ( 0.000000000000000000, -30.93515269692088765, -36.04401931830283701 ) ) ;
#40673 = CARTESIAN_POINT ( 'NONE',  ( -41.78821403078462282, 40.00000000000000000, -47.79414628086202299 ) ) ;
#40674 = EDGE_CURVE ( 'NONE', #28703, #19537, #37696, .T. ) ;
#40675 = EDGE_CURVE ( 'NONE', #16446, #11466, #27253, .T. ) ;
#40676 = DIRECTION ( 'NONE',  ( 1.000000000000000000, 0.000000000000000000, 0.000000000000000000 ) ) ;
#40677 = EDGE_CURVE ( 'NONE', #11747, #17756, #40457, .T. ) ;
#40678 = ADVANCED_FACE ( 'NONE', ( #23146 ), #18950, .T. ) ;
#40679 = AXIS2_PLACEMENT_3D ( 'NONE', #4778, #27927, #31603 ) ;
#40680 = CARTESIAN_POINT ( 'NONE',  ( 0.000000000000000000, -46.87740477351715640, 16.82754413119429771 ) ) ;
#40681 = ORIENTED_EDGE ( 'NONE', *, *, #7567, .T. ) ;
#40682 = CARTESIAN_POINT ( 'NONE',  ( -1.828356344711647319, -3.563200125723192002, -1.076197711133951296E-14 ) ) ;
#40683 = ORIENTED_EDGE ( 'NONE', *, *, #23392, .T. ) ;
#40684 = CIRCLE ( 'NONE', #6557, 59.00000000000000711 ) ;
#40685 = DIRECTION ( 'NONE',  ( -1.000000000000000000, -0.000000000000000000, 0.000000000000000000 ) ) ;
#40686 = DIRECTION ( 'NONE',  ( 0.000000000000000000, 0.5076658003388352380, 0.8615540813938089570 ) ) ;
#40687 = CARTESIAN_POINT ( 'NONE',  ( -58.48566925783705983, 31.00000000000000711, -15.65830181327787862 ) ) ;
#40688 = CARTESIAN_POINT ( 'NONE',  ( 18.00000000000000355, -27.79676263918213763, 37.88001506494759241 ) ) ;
#40689 = ORIENTED_EDGE ( 'NONE', *, *, #40201, .T. ) ;
#40690 = CIRCLE ( 'NONE', #34863, 36.00000000000000000 ) ;
#40691 = DIRECTION ( 'NONE',  ( 1.000000000000000000, 0.000000000000000000, 0.000000000000000000 ) ) ;
#40692 = VERTEX_POINT ( 'NONE', #39875 ) ;
#40693 = CARTESIAN_POINT ( 'NONE',  ( -5.732510072307491988, 40.00000000000000000, -21.37570426403446078 ) ) ;
#40694 = CIRCLE ( 'NONE', #5184, 116.0000000000000000 ) ;
#40695 = EDGE_LOOP ( 'NONE', ( #23664, #9880, #29874, #11900 ) ) ;
#40696 = LINE ( 'NONE', #37222, #36073 ) ;
#40697 = DIRECTION ( 'NONE',  ( 0.000000000000000000, 0.9826841245925200807, 0.1852887240871181618 ) ) ;
#40698 = CARTESIAN_POINT ( 'NONE',  ( 69.81317433577432041, 31.00000000000000000, 34.54326205989952570 ) ) ;
#40699 = CARTESIAN_POINT ( 'NONE',  ( 76.69346925290108175, 39.99999999999999289, 10.21457306974340007 ) ) ;
#40700 = DIRECTION ( 'NONE',  ( 0.000000000000000000, 0.9048270524660205760, -0.4257792915650702170 ) ) ;
#40701 = AXIS2_PLACEMENT_3D ( 'NONE', #14601, #37042, #23988 ) ;
#40702 = AXIS2_PLACEMENT_3D ( 'NONE', #20093, #9353, #151 ) ;
#40703 = EDGE_CURVE ( 'NONE', #40190, #37810, #6506, .T. ) ;
#40704 = ORIENTED_EDGE ( 'NONE', *, *, #24960, .T. ) ;
#40705 = LINE ( 'NONE', #11505, #23511 ) ;
#40706 = ORIENTED_EDGE ( 'NONE', *, *, #19605, .T. ) ;
#40707 = CARTESIAN_POINT ( 'NONE',  ( 17.99999999999999645, 0.000000000000000000, 0.000000000000000000 ) ) ;
#40708 = CIRCLE ( 'NONE', #21968, 15.99999999999998934 ) ;
#40709 = DIRECTION ( 'NONE',  ( -1.000000000000000000, 0.000000000000000000, -0.000000000000000000 ) ) ;
#40710 = ADVANCED_FACE ( 'NONE', ( #19866 ), #33135, .T. ) ;
#40711 = MECHANICAL_DESIGN_GEOMETRIC_PRESENTATION_REPRESENTATION (  '', ( #33788 ), #21970 ) ;
#40713 = ORIENTED_EDGE ( 'NONE', *, *, #40740, .F. ) ;
#40712 = CARTESIAN_POINT ( 'NONE',  ( 18.00000000000000355, -46.11014828289837197, -9.022736828081200144 ) ) ;
#40714 = DIRECTION ( 'NONE',  ( 1.000000000000000000, 0.000000000000000000, 0.000000000000000000 ) ) ;
#40715 = ORIENTED_EDGE ( 'NONE', *, *, #8471, .F. ) ;
#40716 = CARTESIAN_POINT ( 'NONE',  ( 33.90854556226734218, -35.35525454449573601, -74.83297477053821467 ) ) ;
#40717 = AXIS2_PLACEMENT_3D ( 'NONE', #41146, #40714, #14586 ) ;
#40718 = CARTESIAN_POINT ( 'NONE',  ( -49.69442049507403425, 40.00000000000000000, -64.76435429890716478 ) ) ;
#40719 = DIRECTION ( 'NONE',  ( 0.000000000000000000, 0.000000000000000000, 1.000000000000000000 ) ) ;
#40720 = ORIENTED_EDGE ( 'NONE', *, *, #23698, .F. ) ;
#40721 = CYLINDRICAL_SURFACE ( 'NONE', #26238, 59.00000000000000000 ) ;
#40722 = DIRECTION ( 'NONE',  ( -1.000000000000000000, 0.000000000000000000, 0.000000000000000000 ) ) ;
#40723 = VERTEX_POINT ( 'NONE', #6732 ) ;
#40724 = AXIS2_PLACEMENT_3D ( 'NONE', #7712, #21076, #39985 ) ;
#40725 = VERTEX_POINT ( 'NONE', #16360 ) ;
#40726 = DIRECTION ( 'NONE',  ( -1.000000000000000000, -0.000000000000000000, 0.000000000000000000 ) ) ;
#40727 = EDGE_LOOP ( 'NONE', ( #26582, #2874, #30007, #38301 ) ) ;
#40728 = CARTESIAN_POINT ( 'NONE',  ( 12.70938237924789860, 40.00000000000000000, -21.97768283340562689 ) ) ;
#40729 = DIRECTION ( 'NONE',  ( 0.000000000000000000, 1.541976423090494844E-15, 1.000000000000000000 ) ) ;
#40730 = ADVANCED_FACE ( 'NONE', ( #29669 ), #20097, .T. ) ;
#40731 = DIRECTION ( 'NONE',  ( 1.000000000000000000, 0.000000000000000000, 0.000000000000000000 ) ) ;
#40732 = EDGE_CURVE ( 'NONE', #5010, #14947, #13099, .T. ) ;
#40733 = ADVANCED_FACE ( 'NONE', ( #20303 ), #39667, .F. ) ;
#40734 = COLOUR_RGB ( '', 0.09019608, 0.27058824, 0.51372549) ;
#40735 = CARTESIAN_POINT ( 'NONE',  ( 6.600000000000008527, 6.938893903907228378E-15, 0.000000000000000000 ) ) ;
#40737 = ORIENTED_EDGE ( 'NONE', *, *, #37568, .F. ) ;
#40736 = CIRCLE ( 'NONE', #332, 51.99999999999999289 ) ;
#40739 = FACE_OUTER_BOUND ( 'NONE', #24341, .T. ) ;
#40738 = CARTESIAN_POINT ( 'NONE',  ( -10.00000000000000000, 0.000000000000000000, 0.000000000000000000 ) ) ;
#40740 = EDGE_CURVE ( 'NONE', #27094, #9333, #30743, .T. ) ;
#40741 = VERTEX_POINT ( 'NONE', #30307 ) ;
#40742 = VECTOR ( 'NONE', #33538, 1000.000000000000000 ) ;
#40743 = CARTESIAN_POINT ( 'NONE',  ( 18.00000000000000355, -46.90537658765328644, -2.727856614654796452 ) ) ;
#40744 = CARTESIAN_POINT ( 'NONE',  ( -3.620280825866593055, 31.00000000000000355, 27.53105304817175636 ) ) ;
#40745 = VERTEX_POINT ( 'NONE', #27046 ) ;
#40746 = CARTESIAN_POINT ( 'NONE',  ( 22.90854556226710415, -14.05525454449572997, -74.83297477053821467 ) ) ;
#40747 = AXIS2_PLACEMENT_3D ( 'NONE', #18248, #28041, #21087 ) ;
#40748 = CARTESIAN_POINT ( 'NONE',  ( 17.99999999999999645, 0.000000000000000000, 0.000000000000000000 ) ) ;
#40749 = CONTEXT_DEPENDENT_SHAPE_REPRESENTATION ( #21221, #18986 ) ;
#40751 = VECTOR ( 'NONE', #35679, 1000.000000000000000 ) ;
#40750 = DIRECTION ( 'NONE',  ( 0.000000000000000000, 0.9618256431728179345, 0.2736629900720866648 ) ) ;
#40752 = CARTESIAN_POINT ( 'NONE',  ( -18.69663849766352826, 31.00000000000000355, -69.77653669617104981 ) ) ;
#40753 = EDGE_CURVE ( 'NONE', #31904, #25141, #38385, .T. ) ;
#40754 = ORIENTED_EDGE ( 'NONE', *, *, #8559, .T. ) ;
#40755 = CARTESIAN_POINT ( 'NONE',  ( 44.12914893500597202, 31.00000000000000355, -14.89880614700436112 ) ) ;
#40756 = CARTESIAN_POINT ( 'NONE',  ( 50.95389515256417923, 40.00000000000000000, -66.42840393140320998 ) ) ;
#40757 = DIRECTION ( 'NONE',  ( -0.000000000000000000, -0.000000000000000000, -1.000000000000000000 ) ) ;
#40758 = CARTESIAN_POINT ( 'NONE',  ( 0.000000000000000000, 53.40478689619876462, -108.0204598100360016 ) ) ;
#40759 = DIRECTION ( 'NONE',  ( 1.000000000000000000, -0.000000000000000000, 0.000000000000000000 ) ) ;
#40760 = AXIS2_PLACEMENT_3D ( 'NONE', #2058, #32178, #14986 ) ;
#40762 = VERTEX_POINT ( 'NONE', #34645 ) ;
#40761 = DIRECTION ( 'NONE',  ( -1.000000000000000000, 0.000000000000000000, 0.000000000000000000 ) ) ;
#40763 = DIRECTION ( 'NONE',  ( 0.000000000000000000, 0.000000000000000000, 1.000000000000000000 ) ) ;
#40764 = CIRCLE ( 'NONE', #27570, 47.49900000000000233 ) ;
#40765 = LINE ( 'NONE', #20984, #17499 ) ;
#40766 = AXIS2_PLACEMENT_3D ( 'NONE', #31892, #27779, #21247 ) ;
#40767 = VERTEX_POINT ( 'NONE', #41386 ) ;
#40768 = CARTESIAN_POINT ( 'NONE',  ( -31.39472673864601049, 40.00000000000000000, -40.91112553188754930 ) ) ;
#40769 = CYLINDRICAL_SURFACE ( 'NONE', #27800, 59.00000000000000000 ) ;
#40770 = DIRECTION ( 'NONE',  ( 0.000000000000000000, 0.000000000000000000, 1.000000000000000000 ) ) ;
#40771 = VECTOR ( 'NONE', #7057, 1000.000000000000000 ) ;
#40772 = VERTEX_POINT ( 'NONE', #35445 ) ;
#40773 = AXIS2_PLACEMENT_3D ( 'NONE', #13051, #9748, #25928 ) ;
#40774 = CARTESIAN_POINT ( 'NONE',  ( 17.99999999999999645, 87.74575819880270444, -75.87280091124384285 ) ) ;
#40775 = CARTESIAN_POINT ( 'NONE',  ( 0.000000000000000000, -52.88069566989523906, 103.2454939717367211 ) ) ;
#40776 = COLOUR_RGB ( '', 0.66274510, 0.83137255, 0.94901961) ;
#40777 = VERTEX_POINT ( 'NONE', #21170 ) ;
#40778 = CYLINDRICAL_SURFACE ( 'NONE', #31895, 15.00000000000000000 ) ;
#40779 = ORIENTED_EDGE ( 'NONE', *, *, #38877, .T. ) ;
#40780 = AXIS2_PLACEMENT_3D ( 'NONE', #30397, #10088, #23436 ) ;
#40781 = DIRECTION ( 'NONE',  ( 1.000000000000000000, 1.836909530733573776E-16, 0.000000000000000000 ) ) ;
#40782 = ORIENTED_EDGE ( 'NONE', *, *, #551, .F. ) ;
#40783 = CARTESIAN_POINT ( 'NONE',  ( 0.000000000000000000, -16.77566611177699940, -119.3275660838943963 ) ) ;
#40784 = CARTESIAN_POINT ( 'NONE',  ( -101.9959696149863930, 31.00000000000000355, -0.1269066430507536924 ) ) ;
#40785 = VERTEX_POINT ( 'NONE', #14822 ) ;
#40786 = LINE ( 'NONE', #10705, #27536 ) ;
#40787 = EDGE_CURVE ( 'NONE', #41769, #15814, #11949, .T. ) ;
#40788 = DIRECTION ( 'NONE',  ( 0.000000000000000000, -0.9996456111234522934, -0.02662052143778456323 ) ) ;
#40789 = ORIENTED_EDGE ( 'NONE', *, *, #14634, .T. ) ;
#40790 = FACE_OUTER_BOUND ( 'NONE', #532, .T. ) ;
#40791 = CARTESIAN_POINT ( 'NONE',  ( 17.99999999999999645, -28.57802095670076881, -14.28532136906702732 ) ) ;
#40792 = VECTOR ( 'NONE', #39564, 1000.000000000000000 ) ;
#40793 = DIRECTION ( 'NONE',  ( 0.000000000000000000, 0.000000000000000000, 1.000000000000000000 ) ) ;
#40794 = VECTOR ( 'NONE', #8450, 1000.000000000000000 ) ;
#40795 = DIRECTION ( 'NONE',  ( -1.000000000000000000, -0.000000000000000000, 0.000000000000000000 ) ) ;
#40796 = ORIENTED_EDGE ( 'NONE', *, *, #13301, .T. ) ;
#40797 = EDGE_CURVE ( 'NONE', #36072, #7950, #1472, .T. ) ;
#40798 = AXIS2_PLACEMENT_3D ( 'NONE', #20699, #39840, #40697 ) ;
#40799 = DIRECTION ( 'NONE',  ( -0.6083093092473085273, 1.336247061659937394E-16, 0.7937000593946447191 ) ) ;
#40800 = LINE ( 'NONE', #10956, #42029 ) ;
#40801 = CARTESIAN_POINT ( 'NONE',  ( 44.50160557815096496, 31.00000000000000355, -5.869829666507492050 ) ) ;
#40802 = EDGE_LOOP ( 'NONE', ( #43042, #6983, #7005, #29507 ) ) ;
#40803 = AXIS2_PLACEMENT_3D ( 'NONE', #9003, #8149, #41288 ) ;
#40805 = DIRECTION ( 'NONE',  ( 1.541976423090495042E-15, -1.000000000000000000, 4.818676322157797005E-17 ) ) ;
#40804 = CYLINDRICAL_SURFACE ( 'NONE', #222, 116.0000000000000000 ) ;
#40806 = EDGE_CURVE ( 'NONE', #29283, #21974, #10891, .T. ) ;
#40807 = VECTOR ( 'NONE', #24824, 1000.000000000000000 ) ;
#40808 = DIRECTION ( 'NONE',  ( 0.000000000000000000, 0.9048270524660175784, 0.4257792915650768784 ) ) ;
#40809 = ORIENTED_EDGE ( 'NONE', *, *, #41226, .F. ) ;
#40810 = VECTOR ( 'NONE', #41522, 1000.000000000000000 ) ;
#40811 = CIRCLE ( 'NONE', #2495, 19.11697999999999809 ) ;
#40812 = CARTESIAN_POINT ( 'NONE',  ( 0.000000000000000000, -28.35267316522767445, -22.18391138608739155 ) ) ;
#40813 = CARTESIAN_POINT ( 'NONE',  ( -50.10416666532988472, 40.00000000000000000, -3.272492339034341224 ) ) ;
#40814 = CARTESIAN_POINT ( 'NONE',  ( 25.95756378415974908, 40.00000000000000000, 52.86556711864420066 ) ) ;
#40815 = CIRCLE ( 'NONE', #36613, 100.0000000000000000 ) ;
#40816 = DIRECTION ( 'NONE',  ( -1.000000000000000000, -0.000000000000000000, 0.000000000000000000 ) ) ;
#40817 = CARTESIAN_POINT ( 'NONE',  ( 0.000000000000000000, 92.25992191227497585, -77.51514567967302582 ) ) ;
#40818 = LINE ( 'NONE', #43077, #26889 ) ;
#40819 = DIRECTION ( 'NONE',  ( -1.000000000000000000, 0.000000000000000000, 0.000000000000000000 ) ) ;
#40820 = EDGE_LOOP ( 'NONE', ( #13138, #2489 ) ) ;
#40821 = CARTESIAN_POINT ( 'NONE',  ( -7.088330391075835735, 40.00000000000000000, -20.85399598300688595 ) ) ;
#40822 = ORIENTED_EDGE ( 'NONE', *, *, #17821, .T. ) ;
#40823 = CARTESIAN_POINT ( 'NONE',  ( 2.500000000000000000, -1.178949249685214307, 2.042000000000001592 ) ) ;
#40824 = DIRECTION ( 'NONE',  ( 0.000000000000000000, -0.3681245526846654292, -0.9297764858882562322 ) ) ;
#40825 = ORIENTED_EDGE ( 'NONE', *, *, #23817, .T. ) ;
#40826 = CIRCLE ( 'NONE', #3190, 116.0000000000000000 ) ;
#40827 = DIRECTION ( 'NONE',  ( 0.000000000000000000, 1.000000000000000000, 0.000000000000000000 ) ) ;
#40828 = CARTESIAN_POINT ( 'NONE',  ( 0.2500000000000002220, 4.898587196589412829E-16, -4.000000000000000000 ) ) ;
#40829 = ORIENTED_EDGE ( 'NONE', *, *, #28934, .T. ) ;
#40830 = CARTESIAN_POINT ( 'NONE',  ( 17.99999999999999645, 16.77727049691149475, -27.19001440037526862 ) ) ;
#40831 = CIRCLE ( 'NONE', #10907, 59.00000000000000000 ) ;
#40832 = ORIENTED_EDGE ( 'NONE', *, *, #36206, .F. ) ;
#40833 = AXIS2_PLACEMENT_3D ( 'NONE', #2310, #28975, #18771 ) ;
#40834 = AXIS2_PLACEMENT_3D ( 'NONE', #30014, #278, #42843 ) ;
#40835 = ORIENTED_EDGE ( 'NONE', *, *, #20845, .T. ) ;
#40836 = COLOUR_RGB ( '', 0.72549020, 0.75294118, 0.79215686) ;
#40838 = ORIENTED_EDGE ( 'NONE', *, *, #33933, .T. ) ;
#40837 = FACE_OUTER_BOUND ( 'NONE', #33729, .T. ) ;
#40839 = CARTESIAN_POINT ( 'NONE',  ( -32.59403919554602425, 31.00000000000000355, -66.35267222981636337 ) ) ;
#40840 = AXIS2_PLACEMENT_3D ( 'NONE', #5921, #5714, #15568 ) ;
#40841 = ORIENTED_EDGE ( 'NONE', *, *, #24981, .F. ) ;
#40842 = DIRECTION ( 'NONE',  ( 1.000000000000000000, -1.373900992973641277E-15, -5.551115123125812284E-16 ) ) ;
#40843 = CIRCLE ( 'NONE', #29020, 36.00000000000000000 ) ;
#40844 = EDGE_CURVE ( 'NONE', #30103, #12063, #15447, .T. ) ;
#40845 = VERTEX_POINT ( 'NONE', #17900 ) ;
#40846 = CARTESIAN_POINT ( 'NONE',  ( 26.85238513915532721, -12.05525454449572464, 88.54322126041917329 ) ) ;
#40847 = CIRCLE ( 'NONE', #10179, 13.59999999999999964 ) ;
#40848 = ORIENTED_EDGE ( 'NONE', *, *, #30631, .T. ) ;
#40849 = CARTESIAN_POINT ( 'NONE',  ( 94.26586287999622016, 39.99999999999999289, 25.37251369638877563 ) ) ;
#40851 = DIRECTION ( 'NONE',  ( 3.996523416598930318E-16, -2.658563593772947863E-15, -1.000000000000000000 ) ) ;
#40850 = DIRECTION ( 'NONE',  ( 0.000000000000000000, 0.9213119778704113028, 0.3888241754733245403 ) ) ;
#40852 = AXIS2_PLACEMENT_3D ( 'NONE', #22841, #6208, #19554 ) ;
#40853 = FACE_OUTER_BOUND ( 'NONE', #20550, .T. ) ;
#40854 = LINE ( 'NONE', #34110, #21514 ) ;
#40855 = VERTEX_POINT ( 'NONE', #38133 ) ;
#40856 = EDGE_CURVE ( 'NONE', #32115, #30953, #14609, .T. ) ;
#40857 =( NAMED_UNIT ( * ) PLANE_ANGLE_UNIT ( ) SI_UNIT ( $, .RADIAN. ) );
#40858 = LINE ( 'NONE', #11014, #37253 ) ;
#40859 = EDGE_CURVE ( 'NONE', #32785, #9347, #27990, .T. ) ;
#40860 = CARTESIAN_POINT ( 'NONE',  ( -77.37786320076959612, 31.00000000000000711, 44.69160382239309115 ) ) ;
#40861 = DIRECTION ( 'NONE',  ( 0.1305261922200512681, -0.9914448613738104932, 0.000000000000000000 ) ) ;
#40862 = ORIENTED_EDGE ( 'NONE', *, *, #32934, .T. ) ;
#40863 = CIRCLE ( 'NONE', #22120, 2.649999999999973266 ) ;
#40864 = AXIS2_PLACEMENT_3D ( 'NONE', #1386, #38036, #4664 ) ;
#40865 = CARTESIAN_POINT ( 'NONE',  ( -21.70016380022027391, 40.00000000000000000, -5.809120511592388958 ) ) ;
#40866 = AXIS2_PLACEMENT_3D ( 'NONE', #35562, #5682, #15969 ) ;
#40867 = ORIENTED_EDGE ( 'NONE', *, *, #22672, .T. ) ;
#40868 = ORIENTED_EDGE ( 'NONE', *, *, #24741, .T. ) ;
#40869 = LINE ( 'NONE', #37605, #36687 ) ;
#40870 = CYLINDRICAL_SURFACE ( 'NONE', #35921, 2.649999999999999467 ) ;
#40871 = CIRCLE ( 'NONE', #30440, 20.00000000000000711 ) ;
#40872 = DIRECTION ( 'NONE',  ( 1.000000000000000000, 0.000000000000000000, 0.000000000000000000 ) ) ;
#40873 = CIRCLE ( 'NONE', #38797, 64.99999999999998579 ) ;
#40874 = ORIENTED_EDGE ( 'NONE', *, *, #6268, .T. ) ;
#40875 = CYLINDRICAL_SURFACE ( 'NONE', #1233, 116.0000000000000000 ) ;
#40876 = ORIENTED_EDGE ( 'NONE', *, *, #16727, .F. ) ;
#40877 = DIRECTION ( 'NONE',  ( 0.000000000000000000, -0.5076658003388293539, -0.8615540813938123987 ) ) ;
#40878 = EDGE_CURVE ( 'NONE', #2459, #42969, #26566, .T. ) ;
#40879 = CARTESIAN_POINT ( 'NONE',  ( 17.99999999999999645, -2.418575551220017328, -120.4767259403369053 ) ) ;
#40880 = CIRCLE ( 'NONE', #1868, 31.49900000000000588 ) ;
#40881 = EDGE_CURVE ( 'NONE', #27385, #36371, #14754, .T. ) ;
#40882 = FACE_OUTER_BOUND ( 'NONE', #29096, .T. ) ;
#40883 = DIRECTION ( 'NONE',  ( -1.000000000000000000, 0.000000000000000000, 0.000000000000000000 ) ) ;
#40884 = EDGE_LOOP ( 'NONE', ( #15681, #25769, #38786, #23130 ) ) ;
#40885 = VERTEX_POINT ( 'NONE', #1264 ) ;
#40886 = FACE_OUTER_BOUND ( 'NONE', #21465, .T. ) ;
#40887 = CARTESIAN_POINT ( 'NONE',  ( 17.99999999999999645, -120.2856157092987388, 7.201503623196430226 ) ) ;
#40888 = LINE ( 'NONE', #24369, #35481 ) ;
#40889 = ORIENTED_EDGE ( 'NONE', *, *, #35908, .F. ) ;
#40891 = EDGE_LOOP ( 'NONE', ( #18011, #9505, #10096, #33764 ) ) ;
#40890 = DIRECTION ( 'NONE',  ( 0.000000000000000000, 0.000000000000000000, -1.000000000000000000 ) ) ;
#40892 = CARTESIAN_POINT ( 'NONE',  ( 34.59698569360211451, 31.00000000000000355, -30.23997570423561498 ) ) ;
#40893 = CARTESIAN_POINT ( 'NONE',  ( -22.00000000000000711, 40.00000000000000000, 0.000000000000000000 ) ) ;
#40894 = AXIS2_PLACEMENT_3D ( 'NONE', #3777, #13232, #30449 ) ;
#40895 = CIRCLE ( 'NONE', #29098, 116.0000000000000000 ) ;
#40896 = CIRCLE ( 'NONE', #32564, 13.59999999999999964 ) ;
#40898 = DIRECTION ( 'NONE',  ( -1.058513553088275437E-16, -1.000000000000000000, 8.813324511995299047E-17 ) ) ;
#40897 = LINE ( 'NONE', #966, #33516 ) ;
#40899 = ORIENTED_EDGE ( 'NONE', *, *, #11919, .T. ) ;
#40900 = CARTESIAN_POINT ( 'NONE',  ( 21.04585062969761822, 40.00000000000000000, -61.66509230325024760 ) ) ;
#40901 = AXIS2_PLACEMENT_3D ( 'NONE', #16514, #25700, #9506 ) ;
#40902 = CARTESIAN_POINT ( 'NONE',  ( 0.000000000000000000, -107.1354928292872728, 44.47455650398029547 ) ) ;
#40903 = UNCERTAINTY_MEASURE_WITH_UNIT (LENGTH_MEASURE( 1.000000000000000082E-05 ), #23045, 'distance_accuracy_value', 'NONE');
#40904 = DIRECTION ( 'NONE',  ( -0.000000000000000000, -0.000000000000000000, -1.000000000000000000 ) ) ;
#40905 = ORIENTED_EDGE ( 'NONE', *, *, #27683, .F. ) ;
#40906 = DIRECTION ( 'NONE',  ( 0.000000000000000000, 0.000000000000000000, 1.000000000000000000 ) ) ;
#40907 = EDGE_LOOP ( 'NONE', ( #33650, #3908, #21966, #6107 ) ) ;
#40908 = EDGE_CURVE ( 'NONE', #26205, #40508, #20333, .T. ) ;
#40909 = SHAPE_REPRESENTATION_RELATIONSHIP ( 'NONE' , 'NONE' ,  #41895, #31788 ) ;
#40910 = APPLICATION_CONTEXT ( 'automotive_design' ) ;
#40911 = DIRECTION ( 'NONE',  ( -1.000000000000000000, 0.000000000000000000, 0.000000000000000000 ) ) ;
#40912 = LINE ( 'NONE', #17633, #31057 ) ;
#40913 = AXIS2_PLACEMENT_3D ( 'NONE', #33665, #3750, #17133 ) ;
#40914 = EDGE_CURVE ( 'NONE', #22117, #28016, #25900, .T. ) ;
#40915 = CARTESIAN_POINT ( 'NONE',  ( -57.43240763726046794, 31.00000000000000355, -19.49446143887317717 ) ) ;
#40916 = DIRECTION ( 'NONE',  ( -1.000000000000000000, -0.000000000000000000, -0.000000000000000000 ) ) ;
#40917 = ORIENTED_EDGE ( 'NONE', *, *, #27368, .T. ) ;
#40918 = CARTESIAN_POINT ( 'NONE',  ( 0.000000000000000000, -15.49408907645202937, 44.90087086784588166 ) ) ;
#40919 = ORIENTED_EDGE ( 'NONE', *, *, #28914, .T. ) ;
#40920 = CARTESIAN_POINT ( 'NONE',  ( -17.40445659762299968, 40.00000000000000000, 22.69748452323785060 ) ) ;
#40921 = ORIENTED_EDGE ( 'NONE', *, *, #17362, .F. ) ;
#40922 = CARTESIAN_POINT ( 'NONE',  ( 42.80287614962790599, -40.05525454449572464, 69.29271901957253021 ) ) ;
#40923 = CARTESIAN_POINT ( 'NONE',  ( 0.000000000000000000, 0.000000000000000000, 0.000000000000000000 ) ) ;
#40924 = CIRCLE ( 'NONE', #15206, 31.49899999999999523 ) ;
#40925 = CARTESIAN_POINT ( 'NONE',  ( -71.90006454728114704, 31.00000000000000711, 4.599370544632132685 ) ) ;
#40926 = CARTESIAN_POINT ( 'NONE',  ( 68.60033760563641181, 39.99999999999999289, -33.70054013428169526 ) ) ;
#40927 = DIRECTION ( 'NONE',  ( 0.000000000000000000, 0.000000000000000000, 1.000000000000000000 ) ) ;
#40928 = EDGE_LOOP ( 'NONE', ( #37146, #11883, #41566, #15821 ) ) ;
#40929 = CARTESIAN_POINT ( 'NONE',  ( 18.00000000000000355, -44.75336757549769118, -14.30704879393654316 ) ) ;
#40930 = VECTOR ( 'NONE', #654, 1000.000000000000000 ) ;
#40931 = VERTEX_POINT ( 'NONE', #1030 ) ;
#40932 = CIRCLE ( 'NONE', #15909, 31.49900000000000233 ) ;
#40933 = DIRECTION ( 'NONE',  ( -1.000000000000000000, 0.000000000000000000, 0.000000000000000000 ) ) ;
#40934 = EDGE_CURVE ( 'NONE', #16359, #848, #34244, .T. ) ;
#40935 = DIRECTION ( 'NONE',  ( 0.000000000000000000, 0.000000000000000000, 1.000000000000000000 ) ) ;
#40936 = EDGE_CURVE ( 'NONE', #36435, #38324, #18979, .T. ) ;
#40937 = CIRCLE ( 'NONE', #33295, 59.00000000000000000 ) ;
#40938 = EDGE_CURVE ( 'NONE', #4481, #6529, #17678, .T. ) ;
#40939 = EDGE_CURVE ( 'NONE', #28172, #11528, #23139, .T. ) ;
#40941 = ORIENTED_EDGE ( 'NONE', *, *, #36548, .T. ) ;
#40940 = DIRECTION ( 'NONE',  ( 0.000000000000000000, 0.000000000000000000, 1.000000000000000000 ) ) ;
#40942 = DIRECTION ( 'NONE',  ( 0.000000000000000000, -0.9826841245925190815, -0.1852887240871243235 ) ) ;
#40943 = ORIENTED_EDGE ( 'NONE', *, *, #5517, .F. ) ;
#40944 = LINE ( 'NONE', #37672, #20996 ) ;
#40945 = CARTESIAN_POINT ( 'NONE',  ( 31.25450476884064699, 40.00000000000000000, 92.02345382966369414 ) ) ;
#40946 = FACE_OUTER_BOUND ( 'NONE', #14488, .T. ) ;
#40947 = VERTEX_POINT ( 'NONE', #28122 ) ;
#40948 = CARTESIAN_POINT ( 'NONE',  ( 17.99999999999999645, -31.81777574834303124, -2.898764365605651427 ) ) ;
#40949 = DIRECTION ( 'NONE',  ( -1.000000000000000000, 0.000000000000000000, -0.000000000000000000 ) ) ;
#40950 = DIRECTION ( 'NONE',  ( 1.000000000000000000, 0.000000000000000000, 0.000000000000000000 ) ) ;
#40951 = ORIENTED_EDGE ( 'NONE', *, *, #11128, .T. ) ;
#40952 = CARTESIAN_POINT ( 'NONE',  ( 17.99999999999999645, 78.75547124681493472, -91.20343606296920314 ) ) ;
#40953 = EDGE_LOOP ( 'NONE', ( #186, #10166, #29784, #4026 ) ) ;
#40954 = CARTESIAN_POINT ( 'NONE',  ( -30.58448433907587827, 40.00000000000000000, 8.146263651249089577 ) ) ;
#40955 = FACE_OUTER_BOUND ( 'NONE', #7109, .T. ) ;
#40956 = CIRCLE ( 'NONE', #3325, 58.99999999999998579 ) ;
#40957 = FACE_OUTER_BOUND ( 'NONE', #7036, .T. ) ;
#40958 = DIRECTION ( 'NONE',  ( -1.000000000000000000, 0.000000000000000000, 0.000000000000000000 ) ) ;
#40959 = VERTEX_POINT ( 'NONE', #37263 ) ;
#40960 = CIRCLE ( 'NONE', #5447, 116.0000000000000000 ) ;
#40962 = CARTESIAN_POINT ( 'NONE',  ( 0.000000000000000000, 115.9387338813861419, 3.769613505536437259 ) ) ;
#40961 = CARTESIAN_POINT ( 'NONE',  ( 0.000000000000000000, -75.03166794516862126, 94.29071961951481740 ) ) ;
#40963 = AXIS2_PLACEMENT_3D ( 'NONE', #8855, #35663, #15438 ) ;
#40964 = ORIENTED_EDGE ( 'NONE', *, *, #23420, .T. ) ;
#40965 = EDGE_CURVE ( 'NONE', #9979, #34324, #4269, .T. ) ;
#40966 = CIRCLE ( 'NONE', #23605, 120.5010000000000332 ) ;
#40967 = CARTESIAN_POINT ( 'NONE',  ( 8.999999999999998224, 83.58328028049768932, -80.43528614701241963 ) ) ;
#40968 = ADVANCED_FACE ( 'NONE', ( #17460 ), #27463, .T. ) ;
#40969 = CARTESIAN_POINT ( 'NONE',  ( 5.935205493550105516, 31.00000000000000355, -22.18504493031268865 ) ) ;
#40970 = VERTEX_POINT ( 'NONE', #40961 ) ;
#40971 = CYLINDRICAL_SURFACE ( 'NONE', #23224, 59.00000000000000000 ) ;
#40972 = AXIS2_PLACEMENT_3D ( 'NONE', #7415, #37081, #40554 ) ;
#40973 = CARTESIAN_POINT ( 'NONE',  ( 0.000000000000000000, 107.5680526044919674, -31.89649718262133149 ) ) ;
#40974 = CONTEXT_DEPENDENT_SHAPE_REPRESENTATION ( #2477, #12341 ) ;
#40975 = CARTESIAN_POINT ( 'NONE',  ( 0.000000000000000000, 105.7179949885867956, -37.57629584241721687 ) ) ;
#40976 = CARTESIAN_POINT ( 'NONE',  ( 5.072363130230502115, 31.00000000000000355, 77.39583333421907696 ) ) ;
#40977 = ORIENTED_EDGE ( 'NONE', *, *, #39760, .T. ) ;
#40978 = CARTESIAN_POINT ( 'NONE',  ( -32.45554871466278968, 31.00000000000000355, -28.56710966684966380 ) ) ;
#40979 = CARTESIAN_POINT ( 'NONE',  ( -77.84600223180727596, 40.00000000000000711, -20.84395318355897686 ) ) ;
#40980 = CARTESIAN_POINT ( 'NONE',  ( 0.000000000000000000, 0.000000000000000000, 0.000000000000000000 ) ) ;
#40981 = EDGE_CURVE ( 'NONE', #32785, #29037, #37693, .T. ) ;
#40982 = DIRECTION ( 'NONE',  ( -0.000000000000000000, -0.000000000000000000, 1.000000000000000000 ) ) ;
#40983 = CARTESIAN_POINT ( 'NONE',  ( 0.000000000000000000, -6.007673836298252468, 35.49518073029994980 ) ) ;
#40985 = ADVANCED_FACE ( 'NONE', ( #36287 ), #9254, .T. ) ;
#40984 = AXIS2_PLACEMENT_3D ( 'NONE', #32644, #28595, #11805 ) ;
#40986 = EDGE_CURVE ( 'NONE', #42969, #38699, #28702, .T. ) ;
#40987 = ADVANCED_FACE ( 'NONE', ( #3105 ), #6197, .F. ) ;
#40989 = VERTEX_POINT ( 'NONE', #16048 ) ;
#40988 = DIRECTION ( 'NONE',  ( 0.000000000000000000, -0.9911528310040057521, -0.1327255272837325473 ) ) ;
#40990 = CARTESIAN_POINT ( 'NONE',  ( -103.7695705685748635, -106.4195705685759776, 9.999999999999998224 ) ) ;
#40991 = CARTESIAN_POINT ( 'NONE',  ( 2.000000000000005329, -3.464101615137751722, 0.000000000000000000 ) ) ;
#40992 = CIRCLE ( 'NONE', #28525, 58.99999999999999289 ) ;
#40993 = ADVANCED_FACE ( 'NONE', ( #19543 ), #32811, .F. ) ;
#40994 = VERTEX_POINT ( 'NONE', #2889 ) ;
#40995 = CARTESIAN_POINT ( 'NONE',  ( -16.75480014238754478, 40.00000000000000000, -49.32177912249007790 ) ) ;
#40996 = FACE_OUTER_BOUND ( 'NONE', #41653, .T. ) ;
#40997 = CARTESIAN_POINT ( 'NONE',  ( 0.000000000000000000, -46.11014828289837197, -9.022736828081200144 ) ) ;
#40998 = ORIENTED_EDGE ( 'NONE', *, *, #34542, .T. ) ;
#40999 = DIRECTION ( 'NONE',  ( 1.000000000000000000, 0.000000000000000000, 0.000000000000000000 ) ) ;
#41000 = CARTESIAN_POINT ( 'NONE',  ( 17.99999999999999645, 0.000000000000000000, 0.000000000000000000 ) ) ;
#41001 = ORIENTED_EDGE ( 'NONE', *, *, #33267, .T. ) ;
#41002 = CYLINDRICAL_SURFACE ( 'NONE', #20783, 13.59999999999999964 ) ;
#41003 = ORIENTED_EDGE ( 'NONE', *, *, #19953, .F. ) ;
#41004 = CARTESIAN_POINT ( 'NONE',  ( 17.99999999999999645, 28.57802095670106723, -14.28532136906642691 ) ) ;
#41005 = ORIENTED_EDGE ( 'NONE', *, *, #25557, .F. ) ;
#41006 = DIRECTION ( 'NONE',  ( -1.000000000000000000, 0.000000000000000000, -0.000000000000000000 ) ) ;
#41007 = CARTESIAN_POINT ( 'NONE',  ( 17.99999999999999645, -0.6168405712484049674, -35.99471499692227638 ) ) ;
#41008 = EDGE_LOOP ( 'NONE', ( #562, #34626, #42984, #20023 ) ) ;
#41009 = CARTESIAN_POINT ( 'NONE',  ( 17.99999999999999645, 91.51415974874679193, -64.91094698989203948 ) ) ;
#41010 = DIRECTION ( 'NONE',  ( -1.000000000000000000, 0.000000000000000000, 0.000000000000000000 ) ) ;
#41011 = ORIENTED_EDGE ( 'NONE', *, *, #40878, .T. ) ;
#41012 = DIRECTION ( 'NONE',  ( -1.000000000000000000, 0.000000000000000000, 0.000000000000000000 ) ) ;
#41013 = DIRECTION ( 'NONE',  ( -1.000000000000000000, 0.000000000000000000, 0.000000000000000000 ) ) ;
#41014 = AXIS2_PLACEMENT_3D ( 'NONE', #11907, #31969, #40890 ) ;
#41015 = DIRECTION ( 'NONE',  ( -1.000000000000000000, -0.000000000000000000, -0.000000000000000000 ) ) ;
#41016 = CARTESIAN_POINT ( 'NONE',  ( 17.99999999999999645, 34.74871106919766106, -106.6808302961368327 ) ) ;
#41017 = AXIS2_PLACEMENT_3D ( 'NONE', #38419, #31900, #29269 ) ;
#41018 = ORIENTED_EDGE ( 'NONE', *, *, #12405, .T. ) ;
#41019 = CARTESIAN_POINT ( 'NONE',  ( 36.42574649280187771, 8.999999999999994671, -75.69124779287312776 ) ) ;
#41020 = DIRECTION ( 'NONE',  ( 1.000000000000000000, 0.000000000000000000, -0.000000000000000000 ) ) ;
#41021 = CARTESIAN_POINT ( 'NONE',  ( 18.38119342899891961, 31.00000000000000355, 31.81670425098764099 ) ) ;
#41022 = ORIENTED_EDGE ( 'NONE', *, *, #34517, .F. ) ;
#41024 = DIRECTION ( 'NONE',  ( 1.000000000000000000, 0.000000000000000000, 0.000000000000000000 ) ) ;
#41023 = CARTESIAN_POINT ( 'NONE',  ( 9.000000000000001776, 18.53613841426857434, -48.58406706613883586 ) ) ;
#41025 = DIRECTION ( 'NONE',  ( 0.000000000000000000, -0.1837495178165775567, 0.9829730996839004531 ) ) ;
#41026 = ORIENTED_EDGE ( 'NONE', *, *, #22735, .T. ) ;
#41027 = DIRECTION ( 'NONE',  ( -1.000000000000000000, -0.000000000000000000, -0.000000000000000000 ) ) ;
#41028 = CARTESIAN_POINT ( 'NONE',  ( 23.39270017067629936, 40.00000000000000000, 40.49502024156475244 ) ) ;
#41029 = CARTESIAN_POINT ( 'NONE',  ( 56.82522199879618086, 40.00000000000000000, 7.581518937762242949 ) ) ;
#41030 = DIRECTION ( 'NONE',  ( -1.000000000000000000, -0.000000000000000000, -0.000000000000000000 ) ) ;
#41031 = DIRECTION ( 'NONE',  ( 1.000000000000000000, 0.000000000000000000, 0.000000000000000000 ) ) ;
#41032 = EDGE_CURVE ( 'NONE', #18808, #11152, #39797, .T. ) ;
#41033 = EDGE_CURVE ( 'NONE', #16426, #41981, #28018, .T. ) ;
#41034 = CARTESIAN_POINT ( 'NONE',  ( 0.000000000000000000, 19.44205635905601426, -43.33776004284588623 ) ) ;
#41035 = DIRECTION ( 'NONE',  ( -1.000000000000000000, 0.000000000000000000, 0.000000000000000000 ) ) ;
#41036 = EDGE_CURVE ( 'NONE', #40221, #13380, #42824, .T. ) ;
#41037 = EDGE_LOOP ( 'NONE', ( #1196, #28585, #5164, #2938 ) ) ;
#41038 = CARTESIAN_POINT ( 'NONE',  ( -18.92511213055653130, 40.00000000000000000, 21.58621387822740090 ) ) ;
#41039 = VERTEX_POINT ( 'NONE', #15833 ) ;
#41040 = CARTESIAN_POINT ( 'NONE',  ( 17.99999999999999645, 0.000000000000000000, 0.000000000000000000 ) ) ;
#41041 = CARTESIAN_POINT ( 'NONE',  ( -2.807080416178626692, 3.225969019225154444, -3.502507215260441065 ) ) ;
#41042 = ORIENTED_EDGE ( 'NONE', *, *, #15339, .T. ) ;
#41043 = AXIS2_PLACEMENT_3D ( 'NONE', #20664, #16951, #34140 ) ;
#41044 = CARTESIAN_POINT ( 'NONE',  ( 22.90854556226722138, -2.055254544495723756, -74.83297477053847047 ) ) ;
#41045 = DIRECTION ( 'NONE',  ( -1.000000000000000000, 0.000000000000000000, -0.000000000000000000 ) ) ;
#41046 = ORIENTED_EDGE ( 'NONE', *, *, #18863, .T. ) ;
#41047 = CARTESIAN_POINT ( 'NONE',  ( -8.749793197483592522, 117.9447454555042754, 2.972870684497274762 ) ) ;
#41048 = ORIENTED_EDGE ( 'NONE', *, *, #31173, .T. ) ;
#41049 = EDGE_CURVE ( 'NONE', #38810, #12162, #2177, .T. ) ;
#41050 = ORIENTED_EDGE ( 'NONE', *, *, #17048, .T. ) ;
#41051 = DIRECTION ( 'NONE',  ( -1.000000000000000000, 0.000000000000000000, 0.000000000000000000 ) ) ;
#41052 = ADVANCED_FACE ( 'NONE', ( #13202 ), #73, .T. ) ;
#41053 = CARTESIAN_POINT ( 'NONE',  ( 72.60479858918232310, 31.00000000000000000, -24.53750584076950503 ) ) ;
#41054 = ORIENTED_EDGE ( 'NONE', *, *, #33861, .T. ) ;
#41055 = DIRECTION ( 'NONE',  ( 0.000000000000000000, 0.4999999999999990008, -0.8660254037844391517 ) ) ;
#41056 = CARTESIAN_POINT ( 'NONE',  ( 17.99999999999999645, 14.84191762912354839, -27.78316904333109960 ) ) ;
#41057 = ORIENTED_EDGE ( 'NONE', *, *, #24547, .T. ) ;
#41058 = CARTESIAN_POINT ( 'NONE',  ( 17.99999999999999645, -103.1672962317654338, 44.09967643725834563 ) ) ;
#41059 = ORIENTED_EDGE ( 'NONE', *, *, #29415, .F. ) ;
#41060 = CARTESIAN_POINT ( 'NONE',  ( -24.28006566513952791, 40.00000000000000000, -91.10131089348455191 ) ) ;
#41062 = CYLINDRICAL_SURFACE ( 'NONE', #10247, 120.5010000000000190 ) ;
#41061 = FACE_OUTER_BOUND ( 'NONE', #32314, .T. ) ;
#41063 = DIRECTION ( 'NONE',  ( 0.000000000000000000, 0.000000000000000000, -1.000000000000000000 ) ) ;
#41064 = EDGE_CURVE ( 'NONE', #31468, #38864, #14783, .T. ) ;
#41065 = DIRECTION ( 'NONE',  ( -1.000000000000000000, 0.000000000000000000, 0.000000000000000000 ) ) ;
#41066 = ORIENTED_EDGE ( 'NONE', *, *, #7399, .T. ) ;
#41067 =( LENGTH_UNIT ( ) NAMED_UNIT ( * ) SI_UNIT ( .MILLI., .METRE. ) );
#41068 = FILL_AREA_STYLE ('',( #21075 ) ) ;
#41069 = CIRCLE ( 'NONE', #26493, 59.00000000000000000 ) ;
#41070 = VERTEX_POINT ( 'NONE', #35850 ) ;
#41071 = CARTESIAN_POINT ( 'NONE',  ( 17.99999999999999645, -30.78424799127063238, -6.672111855473501940 ) ) ;
#41072 = CIRCLE ( 'NONE', #14653, 47.49900000000000233 ) ;
#41073 = CARTESIAN_POINT ( 'NONE',  ( 22.58587702529213104, 31.00000000000000355, 84.29678642628191199 ) ) ;
#41074 = DIRECTION ( 'NONE',  ( 1.000000000000000000, 0.000000000000000000, 0.000000000000000000 ) ) ;
#41075 = VERTEX_POINT ( 'NONE', #39769 ) ;
#41076 = CARTESIAN_POINT ( 'NONE',  ( -10.52919346384764054, 40.00000000000000000, -21.36894910329525743 ) ) ;
#41077 = ORIENTED_EDGE ( 'NONE', *, *, #34010, .F. ) ;
#41078 = EDGE_LOOP ( 'NONE', ( #35911, #7301 ) ) ;
#41079 = CARTESIAN_POINT ( 'NONE',  ( 2.449848172108560096, 3.432307619358740514, -3.503702292528905637 ) ) ;
#41080 = CARTESIAN_POINT ( 'NONE',  ( 0.000000000000000000, 69.72480978690171582, -92.70626138605946664 ) ) ;
#41081 = FACE_OUTER_BOUND ( 'NONE', #753, .T. ) ;
#41082 = EDGE_CURVE ( 'NONE', #17739, #3818, #26599, .T. ) ;
#41083 = DIRECTION ( 'NONE',  ( 3.996523416598993920E-16, 2.658563593772947074E-15, 1.000000000000000000 ) ) ;
#41084 = ORIENTED_EDGE ( 'NONE', *, *, #2444, .T. ) ;
#41085 = CARTESIAN_POINT ( 'NONE',  ( -10.00000000000000178, 1.641026710857453312E-15, 13.40000000000000036 ) ) ;
#41086 = ORIENTED_EDGE ( 'NONE', *, *, #39657, .T. ) ;
#41087 = DIRECTION ( 'NONE',  ( 1.000000000000000000, 0.000000000000000000, 0.000000000000000000 ) ) ;
#41088 = DIRECTION ( 'NONE',  ( -1.000000000000000000, 0.000000000000000000, 0.000000000000000000 ) ) ;
#41089 = EDGE_CURVE ( 'NONE', #2260, #12961, #25669, .T. ) ;
#41090 = CARTESIAN_POINT ( 'NONE',  ( 17.99999999999999645, 0.000000000000000000, 0.000000000000000000 ) ) ;
#41091 = FACE_OUTER_BOUND ( 'NONE', #26775, .T. ) ;
#41092 = ORIENTED_EDGE ( 'NONE', *, *, #14612, .T. ) ;
#41093 = ORIENTED_EDGE ( 'NONE', *, *, #7104, .T. ) ;
#41094 = DIRECTION ( 'NONE',  ( 1.000000000000000000, 0.000000000000000000, -6.546126324440850663E-16 ) ) ;
#41095 = CARTESIAN_POINT ( 'NONE',  ( 9.999999999999998224, 0.000000000000000000, -13.40000000000000213 ) ) ;
#41096 = ADVANCED_FACE ( 'NONE', ( #39562 ), #2684, .T. ) ;
#41097 = AXIS2_PLACEMENT_3D ( 'NONE', #27941, #11793, #28376 ) ;
#41098 = VERTEX_POINT ( 'NONE', #33250 ) ;
#41100 = VERTEX_POINT ( 'NONE', #9046 ) ;
#41099 = FACE_OUTER_BOUND ( 'NONE', #11680, .T. ) ;
#41101 = AXIS2_PLACEMENT_3D ( 'NONE', #18963, #22649, #32429 ) ;
#41102 = ADVANCED_FACE ( 'NONE', ( #5763 ), #19120, .F. ) ;
#41103 = CARTESIAN_POINT ( 'NONE',  ( -41.92568936860566708, 31.00000000000000355, -5.596851440150872214 ) ) ;
#41104 = AXIS2_PLACEMENT_3D ( 'NONE', #15091, #1307, #8074 ) ;
#41105 = FACE_OUTER_BOUND ( 'NONE', #15794, .T. ) ;
#41107 = CARTESIAN_POINT ( 'NONE',  ( 0.000000000000000000, 11.49545354908936545, 29.80986809967263085 ) ) ;
#41106 = DIRECTION ( 'NONE',  ( -1.000000000000000000, 0.000000000000000000, 0.000000000000000000 ) ) ;
#41108 = VERTEX_POINT ( 'NONE', #25873 ) ;
#41109 = DIRECTION ( 'NONE',  ( -1.000000000000000000, -0.000000000000000000, -0.000000000000000000 ) ) ;
#41110 = CARTESIAN_POINT ( 'NONE',  ( -55.11358496761538106, 40.00000000000000711, 27.06326608206703099 ) ) ;
#41111 = CARTESIAN_POINT ( 'NONE',  ( 17.99999999999999645, 23.87611429743691360, -20.54551452399595135 ) ) ;
#41112 = CARTESIAN_POINT ( 'NONE',  ( -31.74999999999995737, 0.000000000000000000, 4.250000000000000000 ) ) ;
#41113 = ORIENTED_EDGE ( 'NONE', *, *, #35416, .T. ) ;
#41114 = LINE ( 'NONE', #34587, #16833 ) ;
#41115 = EDGE_CURVE ( 'NONE', #33767, #7030, #39122, .T. ) ;
#41116 = ORIENTED_EDGE ( 'NONE', *, *, #16008, .T. ) ;
#41117 =( NAMED_UNIT ( * ) SI_UNIT ( $, .STERADIAN. ) SOLID_ANGLE_UNIT ( ) );
#41118 = EDGE_CURVE ( 'NONE', #3101, #10939, #3570, .T. ) ;
#41119 = DIRECTION ( 'NONE',  ( 1.000000000000000000, 0.000000000000000000, 0.000000000000000000 ) ) ;
#41120 = DIRECTION ( 'NONE',  ( -1.000000000000000000, -0.000000000000000000, -0.000000000000000000 ) ) ;
#41121 = AXIS2_PLACEMENT_3D ( 'NONE', #17732, #14664, #27524 ) ;
#41123 = ADVANCED_FACE ( 'NONE', ( #17570 ), #24105, .F. ) ;
#41122 = CARTESIAN_POINT ( 'NONE',  ( -35.70415035507907930, 31.00000000000000355, 46.55071329160319493 ) ) ;
#41124 = PLANE ( 'NONE',  #29552 ) ;
#41125 = VERTEX_POINT ( 'NONE', #17783 ) ;
#41126 = CIRCLE ( 'NONE', #12605, 58.99999999999999289 ) ;
#41127 = VERTEX_POINT ( 'NONE', #4201 ) ;
#41128 = CARTESIAN_POINT ( 'NONE',  ( -20.72449291656876369, 40.00000000000000000, -23.61699481730619610 ) ) ;
#41129 = AXIS2_PLACEMENT_3D ( 'NONE', #28109, #35056, #41374 ) ;
#41130 = AXIS2_PLACEMENT_3D ( 'NONE', #7692, #21271, #40842 ) ;
#41131 = ORIENTED_EDGE ( 'NONE', *, *, #1278, .T. ) ;
#41132 = DIRECTION ( 'NONE',  ( -1.000000000000000000, 0.000000000000000000, 0.000000000000000000 ) ) ;
#41133 = CYLINDRICAL_SURFACE ( 'NONE', #5287, 20.00000000000000711 ) ;
#41134 = CARTESIAN_POINT ( 'NONE',  ( -54.99468034530342919, 31.00000000000000355, -62.86974495748531666 ) ) ;
#41135 = CARTESIAN_POINT ( 'NONE',  ( -23.42519174997118014, 40.00000000000000000, 87.00664592748896098 ) ) ;
#41136 = VECTOR ( 'NONE', #35942, 1000.000000000000000 ) ;
#41137 = CARTESIAN_POINT ( 'NONE',  ( 17.99999999999999645, 31.11570115861495367, 4.898994019976747438 ) ) ;
#41138 = EDGE_CURVE ( 'NONE', #14755, #7826, #41204, .T. ) ;
#41139 = VERTEX_POINT ( 'NONE', #6844 ) ;
#41140 = CARTESIAN_POINT ( 'NONE',  ( 17.99999999999999645, -61.59243992711522964, 93.77976230226020959 ) ) ;
#41141 = VERTEX_POINT ( 'NONE', #23888 ) ;
#41142 = CARTESIAN_POINT ( 'NONE',  ( 4.121423858225410797, -12.61643262889541006, -1.199999999999999956 ) ) ;
#41143 = CARTESIAN_POINT ( 'NONE',  ( -10.00000000000000000, 0.000000000000000000, 0.000000000000000000 ) ) ;
#41145 = ORIENTED_EDGE ( 'NONE', *, *, #29593, .T. ) ;
#41144 = CARTESIAN_POINT ( 'NONE',  ( 17.99999999999999645, 31.48608500567870294, -0.9019157472705674472 ) ) ;
#41146 = CARTESIAN_POINT ( 'NONE',  ( 0.000000000000000000, 0.000000000000000000, 0.000000000000000000 ) ) ;
#41147 = VERTEX_POINT ( 'NONE', #7701 ) ;
#41148 = DIRECTION ( 'NONE',  ( -1.000000000000000000, 0.000000000000000000, 0.000000000000000000 ) ) ;
#41149 = EDGE_CURVE ( 'NONE', #12162, #27630, #37044, .T. ) ;
#41150 = CARTESIAN_POINT ( 'NONE',  ( 84.73112319332513209, 39.99999999999999289, -41.78253223598262167 ) ) ;
#41151 = DIRECTION ( 'NONE',  ( 0.000000000000000000, 0.000000000000000000, 1.000000000000000000 ) ) ;
#41152 = ORIENTED_EDGE ( 'NONE', *, *, #23317, .F. ) ;
#41153 = CARTESIAN_POINT ( 'NONE',  ( -158.5000000000000284, 2.597717496998779451E-13, 9.999999999999937828 ) ) ;
#41154 = DIRECTION ( 'NONE',  ( 0.000000000000000000, -0.9048270524660235736, 0.4257792915650639998 ) ) ;
#41155 = CIRCLE ( 'NONE', #762, 47.49900000000000233 ) ;
#41157 = DIRECTION ( 'NONE',  ( 0.000000000000000000, -0.9822872507286865007, -0.1873813145857355367 ) ) ;
#41156 = CARTESIAN_POINT ( 'NONE',  ( 17.99999999999999645, -52.88069566989523906, 103.2454939717367211 ) ) ;
#41158 = ORIENTED_EDGE ( 'NONE', *, *, #2691, .T. ) ;
#41159 = CARTESIAN_POINT ( 'NONE',  ( -142.4999999999992326, 9.359674666681006779E-14, -44.99999999999993605 ) ) ;
#41161 = ORIENTED_EDGE ( 'NONE', *, *, #16310, .F. ) ;
#41160 = CIRCLE ( 'NONE', #2143, 59.00000000000000000 ) ;
#41162 = CARTESIAN_POINT ( 'NONE',  ( -2.345747346278108214, 3.264484291692489215, -0.01223254789873409049 ) ) ;
#41163 = CARTESIAN_POINT ( 'NONE',  ( -20.36888183406675168, 40.00000000000000000, -26.63352584488937325 ) ) ;
#41164 = CARTESIAN_POINT ( 'NONE',  ( 17.99999999999999645, -27.83061035787034498, 117.2431154827796576 ) ) ;
#41165 = AXIS2_PLACEMENT_3D ( 'NONE', #1787, #37790, #34310 ) ;
#41166 = CARTESIAN_POINT ( 'NONE',  ( 18.00000000000000355, -45.78515115856051665, 12.64416602183649374 ) ) ;
#41167 = CIRCLE ( 'NONE', #36309, 126.0000000000000284 ) ;
#41168 = DIRECTION ( 'NONE',  ( -1.000000000000000000, 0.000000000000000000, 0.000000000000000000 ) ) ;
#41169 = VERTEX_POINT ( 'NONE', #13630 ) ;
#41171 = DIRECTION ( 'NONE',  ( 0.000000000000000000, 0.000000000000000000, -1.000000000000000000 ) ) ;
#41170 = DIRECTION ( 'NONE',  ( 0.000000000000000000, 0.000000000000000000, 1.000000000000000000 ) ) ;
#41172 = ORIENTED_EDGE ( 'NONE', *, *, #854, .F. ) ;
#41173 = ADVANCED_FACE ( 'NONE', ( #30639 ), #3749, .T. ) ;
#41174 = AXIS2_PLACEMENT_3D ( 'NONE', #3651, #17020, #16601 ) ;
#41175 = CARTESIAN_POINT ( 'NONE',  ( 17.99999999999999645, -80.74349901498459303, 77.90224541347254217 ) ) ;
#41176 = CARTESIAN_POINT ( 'NONE',  ( -2.649999999999784528, -150.5000000000013642, 9.999999999999586109 ) ) ;
#41178 = EDGE_CURVE ( 'NONE', #28718, #36227, #10580, .T. ) ;
#41177 = CARTESIAN_POINT ( 'NONE',  ( 24.89583333603155069, 31.00000000000000355, -1.636246165087041016 ) ) ;
#41179 = VERTEX_POINT ( 'NONE', #7259 ) ;
#41180 = DIRECTION ( 'NONE',  ( 0.000000000000000000, 0.000000000000000000, -1.000000000000000000 ) ) ;
#41181 = CARTESIAN_POINT ( 'NONE',  ( 0.000000000000000000, 59.47573314508733944, 99.59235496188628645 ) ) ;
#41182 = ITEM_DEFINED_TRANSFORMATION ( 'NONE', 'NONE', #28191,  #13552 ) ;
#41183 = FACE_OUTER_BOUND ( 'NONE', #775, .T. ) ;
#41184 = CARTESIAN_POINT ( 'NONE',  ( -10.77850749866037816, 31.00000000000000355, -81.75987728344749428 ) ) ;
#41185 = ORIENTED_EDGE ( 'NONE', *, *, #36159, .T. ) ;
#41186 = EDGE_CURVE ( 'NONE', #31219, #21374, #40419, .T. ) ;
#41187 = CARTESIAN_POINT ( 'NONE',  ( -3.998040010416403334, 31.00000000000000355, 59.59469406578620720 ) ) ;
#41188 = CARTESIAN_POINT ( 'NONE',  ( -45.94448050778635917, 40.00000000000000000, -79.54744219826071117 ) ) ;
#41189 = EDGE_CURVE ( 'NONE', #37133, #18706, #27285, .T. ) ;
#41190 = EDGE_CURVE ( 'NONE', #16540, #36319, #14065, .T. ) ;
#41191 = CARTESIAN_POINT ( 'NONE',  ( 17.99999999999999645, -11.58753559615464290, -29.77419532459275331 ) ) ;
#41192 = CIRCLE ( 'NONE', #38407, 52.00000000000000000 ) ;
#41193 = FACE_OUTER_BOUND ( 'NONE', #39487, .T. ) ;
#41194 = DIRECTION ( 'NONE',  ( 0.000000000000000000, 0.5076658003388410112, -0.8615540813938056264 ) ) ;
#41195 = AXIS2_PLACEMENT_3D ( 'NONE', #1836, #10807, #38058 ) ;
#41197 = ORIENTED_EDGE ( 'NONE', *, *, #27127, .T. ) ;
#41196 = DIRECTION ( 'NONE',  ( 0.000000000000000000, 0.000000000000000000, 1.000000000000000000 ) ) ;
#41198 = CARTESIAN_POINT ( 'NONE',  ( 18.00000000000000355, 18.53613841426857434, -48.58406706613882875 ) ) ;
#41199 = CARTESIAN_POINT ( 'NONE',  ( 0.000000000000000000, 26.29521155129848964, 17.34211205339357065 ) ) ;
#41200 = EDGE_CURVE ( 'NONE', #16458, #12461, #26925, .T. ) ;
#41201 = EDGE_LOOP ( 'NONE', ( #16081, #27786, #3833, #3213 ) ) ;
#41202 = CARTESIAN_POINT ( 'NONE',  ( 57.76613438074698337, 39.99999999999999289, -28.48799604501563110 ) ) ;
#41203 = CYLINDRICAL_SURFACE ( 'NONE', #34715, 59.00000000000000000 ) ;
#41204 = CIRCLE ( 'NONE', #22456, 23.00000000000000000 ) ;
#41205 = ORIENTED_EDGE ( 'NONE', *, *, #39115, .T. ) ;
#41206 = EDGE_CURVE ( 'NONE', #1540, #42489, #30844, .T. ) ;
#41207 = DIRECTION ( 'NONE',  ( -1.000000000000000000, -0.000000000000000000, 0.000000000000000000 ) ) ;
#41208 = PLANE ( 'NONE',  #30588 ) ;
#41209 = ORIENTED_EDGE ( 'NONE', *, *, #1684, .F. ) ;
#41210 = CARTESIAN_POINT ( 'NONE',  ( 18.00000000000000355, 51.93417535146740960, -2.615612846549368431 ) ) ;
#41211 = ORIENTED_EDGE ( 'NONE', *, *, #19770, .T. ) ;
#41212 = CARTESIAN_POINT ( 'NONE',  ( 17.99999999999999645, 0.000000000000000000, 0.000000000000000000 ) ) ;
#41213 = ORIENTED_EDGE ( 'NONE', *, *, #11394, .T. ) ;
#41214 = FACE_OUTER_BOUND ( 'NONE', #2093, .T. ) ;
#41215 = B_SPLINE_CURVE_WITH_KNOTS ( 'NONE', 3,
 ( #11863, #5070, #31920, #11644, #18661, #4406 ),
 .UNSPECIFIED., .F., .F.,
 ( 4, 2, 4 ),
 ( 0.002452478801916361129, 0.003676905084148001344, 0.004901331366379641126 ),
 .UNSPECIFIED. ) ;
#41216 = CARTESIAN_POINT ( 'NONE',  ( -80.34276469477588023, 31.00000000000000711, 61.48650092630385444 ) ) ;
#41217 = EDGE_LOOP ( 'NONE', ( #1850, #27747, #18985, #8896 ) ) ;
#41218 = DIRECTION ( 'NONE',  ( 0.000000000000000000, 0.000000000000000000, 1.000000000000000000 ) ) ;
#41219 = CARTESIAN_POINT ( 'NONE',  ( 17.99999999999999645, 94.83915810436481308, -59.94836581341496640 ) ) ;
#41220 = ORIENTED_EDGE ( 'NONE', *, *, #41715, .F. ) ;
#41221 = DIRECTION ( 'NONE',  ( -1.000000000000000000, 0.000000000000000000, 0.000000000000000000 ) ) ;
#41222 = AXIS2_PLACEMENT_3D ( 'NONE', #28173, #21012, #41441 ) ;
#41223 =( REPRESENTATION_RELATIONSHIP ('NONE','NONE', #330, #18009 ) REPRESENTATION_RELATIONSHIP_WITH_TRANSFORMATION ( #20523 )SHAPE_REPRESENTATION_RELATIONSHIP( ) );
#41224 = CIRCLE ( 'NONE', #27305, 59.00000000000000000 ) ;
#41225 = FACE_OUTER_BOUND ( 'NONE', #25181, .T. ) ;
#41226 = EDGE_CURVE ( 'NONE', #27149, #1451, #20197, .T. ) ;
#41227 = EDGE_CURVE ( 'NONE', #4417, #15422, #11985, .T. ) ;
#41228 = ORIENTED_EDGE ( 'NONE', *, *, #5649, .T. ) ;
#41229 = DIRECTION ( 'NONE',  ( -1.000000000000000000, -0.000000000000000000, -0.000000000000000000 ) ) ;
#41230 = ADVANCED_FACE ( 'NONE', ( #36722 ), #14067, .F. ) ;
#41231 = EDGE_CURVE ( 'NONE', #28909, #30619, #23875, .T. ) ;
#41232 = CIRCLE ( 'NONE', #23188, 20.00000000000000711 ) ;
#41233 = DIRECTION ( 'NONE',  ( 0.000000000000000000, 1.000000000000000000, 0.000000000000000000 ) ) ;
#41234 = ORIENTED_EDGE ( 'NONE', *, *, #11413, .T. ) ;
#41235 = DIRECTION ( 'NONE',  ( -1.276222519706440154E-16, 0.9999999999999998890, -5.451477089573758773E-17 ) ) ;
#41236 = DIRECTION ( 'NONE',  ( 1.000000000000000000, -0.000000000000000000, 0.000000000000000000 ) ) ;
#41237 = CARTESIAN_POINT ( 'NONE',  ( 47.00375723443311671, 31.00000000000000355, -27.15133022689256137 ) ) ;
#41238 = AXIS2_PLACEMENT_3D ( 'NONE', #1580, #8352, #34758 ) ;
#41239 = VERTEX_POINT ( 'NONE', #7051 ) ;
#41241 = CARTESIAN_POINT ( 'NONE',  ( 17.99999999999999645, 10.40101730206366959, 120.0512800434971581 ) ) ;
#41240 = DIRECTION ( 'NONE',  ( 1.000000000000000000, 0.000000000000000000, 0.000000000000000000 ) ) ;
#41242 = CYLINDRICAL_SURFACE ( 'NONE', #10559, 59.00000000000000000 ) ;
#41243 = ORIENTED_EDGE ( 'NONE', *, *, #21246, .T. ) ;
#41244 = CARTESIAN_POINT ( 'NONE',  ( 12.55910585664918422, 0.7408941433508176022, 0.000000000000000000 ) ) ;
#41245 = CARTESIAN_POINT ( 'NONE',  ( 50.84997085138504502, 39.99999999999999289, -39.01959913716785167 ) ) ;
#41246 = CARTESIAN_POINT ( 'NONE',  ( 48.78760054484346398, 40.00000000000000000, -28.06521077754944926 ) ) ;
#41247 = CARTESIAN_POINT ( 'NONE',  ( 18.00000000000000355, 46.21320724403663860, -10.97699764141904843 ) ) ;
#41248 = DIRECTION ( 'NONE',  ( 0.000000000000000000, 0.2486898871648482723, 0.9685831611286327414 ) ) ;
#41249 = CARTESIAN_POINT ( 'NONE',  ( 18.00000000000000355, 38.92705108641770551, -27.21837053747755419 ) ) ;
#41250 = DIRECTION ( 'NONE',  ( -1.000000000000000000, 0.000000000000000000, 0.000000000000000000 ) ) ;
#41251 = ADVANCED_FACE ( 'NONE', ( #40624 ), #917, .F. ) ;
#41252 = AXIS2_PLACEMENT_3D ( 'NONE', #26403, #29034, #23148 ) ;
#41253 = VERTEX_POINT ( 'NONE', #24762 ) ;
#41254 = CARTESIAN_POINT ( 'NONE',  ( 27.23661496637203427, 40.00000000000000000, 23.88131275951389654 ) ) ;
#41255 = ORIENTED_EDGE ( 'NONE', *, *, #10436, .F. ) ;
#41256 = LINE ( 'NONE', #7891, #22984 ) ;
#41257 = CARTESIAN_POINT ( 'NONE',  ( 17.99999999999999645, 100.6739960869717834, 49.52796165323294986 ) ) ;
#41258 = AXIS2_PLACEMENT_3D ( 'NONE', #19725, #16021, #29522 ) ;
#41259 = ORIENTED_EDGE ( 'NONE', *, *, #9707, .T. ) ;
#41260 = ADVANCED_FACE ( 'NONE', ( #21280 ), #18229, .T. ) ;
#41261 = CARTESIAN_POINT ( 'NONE',  ( -12.69999999999999929, 0.000000000000000000, -13.40000000000000213 ) ) ;
#41262 = CIRCLE ( 'NONE', #41979, 2.500000000000000888 ) ;
#41263 = DIRECTION ( 'NONE',  ( 0.000000000000000000, -0.2113826236296113270, -0.9774033898178695612 ) ) ;
#41264 = EDGE_LOOP ( 'NONE', ( #6623, #40423, #36256, #20576 ) ) ;
#41265 = DIRECTION ( 'NONE',  ( 1.000000000000000000, 0.000000000000000000, 0.000000000000000000 ) ) ;
#41266 = ORIENTED_EDGE ( 'NONE', *, *, #980, .F. ) ;
#41267 = VECTOR ( 'NONE', #3277, 1000.000000000000000 ) ;
#41268 = ORIENTED_EDGE ( 'NONE', *, *, #39551, .T. ) ;
#41269 = CARTESIAN_POINT ( 'NONE',  ( 0.000000000000000000, 0.000000000000000000, 0.000000000000000000 ) ) ;
#41270 = CARTESIAN_POINT ( 'NONE',  ( -67.85934734803990409, 31.00000000000000711, 22.92939687791763248 ) ) ;
#41271 = ORIENTED_EDGE ( 'NONE', *, *, #16347, .T. ) ;
#41272 = DIRECTION ( 'NONE',  ( 1.000000000000000000, -0.000000000000000000, -0.000000000000000000 ) ) ;
#41273 = DIRECTION ( 'NONE',  ( -1.000000000000000000, 3.336006684570784581E-17, 0.000000000000000000 ) ) ;
#41274 = ORIENTED_EDGE ( 'NONE', *, *, #37688, .T. ) ;
#41275 = DIRECTION ( 'NONE',  ( -1.000000000000000000, -0.000000000000000000, -0.000000000000000000 ) ) ;
#41276 = VERTEX_POINT ( 'NONE', #38238 ) ;
#41277 = CARTESIAN_POINT ( 'NONE',  ( 30.72743980831338462, 40.00000000000000000, -90.12673907452091271 ) ) ;
#41278 = CARTESIAN_POINT ( 'NONE',  ( 9.304442065603227618, 31.00000000000000355, 27.50946418541002458 ) ) ;
#41280 = FACE_OUTER_BOUND ( 'NONE', #10701, .T. ) ;
#41279 = DIRECTION ( 'NONE',  ( -1.000000000000000000, 0.000000000000000000, 0.000000000000000000 ) ) ;
#41281 = EDGE_CURVE ( 'NONE', #10089, #10944, #40542, .T. ) ;
#41282 = EDGE_CURVE ( 'NONE', #13944, #38187, #5711, .T. ) ;
#41283 = CARTESIAN_POINT ( 'NONE',  ( 9.000000000000001776, 24.47917365150009061, -45.87777302070909258 ) ) ;
#41284 = CARTESIAN_POINT ( 'NONE',  ( -36.94957890273524725, -2.055254544495720648, 165.5452302238048503 ) ) ;
#41285 = ORIENTED_EDGE ( 'NONE', *, *, #30147, .T. ) ;
#41286 = EDGE_CURVE ( 'NONE', #26752, #14373, #1534, .T. ) ;
#41287 = AXIS2_PLACEMENT_3D ( 'NONE', #2949, #2742, #16106 ) ;
#41288 = DIRECTION ( 'NONE',  ( 0.000000000000000000, 0.000000000000000000, 1.000000000000000000 ) ) ;
#41289 = VERTEX_POINT ( 'NONE', #14929 ) ;
#41290 = FACE_OUTER_BOUND ( 'NONE', #29449, .T. ) ;
#41291 = CARTESIAN_POINT ( 'NONE',  ( -49.27414759474276451, 31.00000000000000711, 85.34056160678568403 ) ) ;
#41292 = CARTESIAN_POINT ( 'NONE',  ( 18.00000000000000355, 5.871425383722275626, -51.66745943012274722 ) ) ;
#41293 = VERTEX_POINT ( 'NONE', #41500 ) ;
#41294 = CIRCLE ( 'NONE', #14868, 59.00000000000000000 ) ;
#41295 = CARTESIAN_POINT ( 'NONE',  ( 14.33709021557830887, 40.00000000000000000, 24.89380824183666618 ) ) ;
#41296 = AXIS2_PLACEMENT_3D ( 'NONE', #19872, #20309, #13320 ) ;
#41297 = ORIENTED_EDGE ( 'NONE', *, *, #20424, .T. ) ;
#41298 = EDGE_CURVE ( 'NONE', #26596, #36818, #38016, .T. ) ;
#41299 = ORIENTED_EDGE ( 'NONE', *, *, #11311, .F. ) ;
#41300 = DIRECTION ( 'NONE',  ( -1.000000000000000000, -0.000000000000000000, -0.000000000000000000 ) ) ;
#41301 = DIRECTION ( 'NONE',  ( 1.000000000000000000, 0.000000000000000000, 0.000000000000000000 ) ) ;
#41302 = DIRECTION ( 'NONE',  ( -0.000000000000000000, -0.000000000000000000, 1.000000000000000000 ) ) ;
#41303 = DIRECTION ( 'NONE',  ( -1.000000000000000000, -0.000000000000000000, 0.000000000000000000 ) ) ;
#41304 = ORIENTED_EDGE ( 'NONE', *, *, #11419, .T. ) ;
#41305 = CARTESIAN_POINT ( 'NONE',  ( 0.000000000000000000, 0.000000000000000000, -0.2800830152838844622 ) ) ;
#41306 = VERTEX_POINT ( 'NONE', #14716 ) ;
#41307 = DIRECTION ( 'NONE',  ( 0.000000000000000000, 0.000000000000000000, -1.000000000000000000 ) ) ;
#41308 = CARTESIAN_POINT ( 'NONE',  ( -12.69999999999999929, 0.000000000000000000, 0.000000000000000000 ) ) ;
#41309 = DIRECTION ( 'NONE',  ( 0.000000000000000000, 0.000000000000000000, 1.000000000000000000 ) ) ;
#41310 = DIRECTION ( 'NONE',  ( 0.000000000000000000, 0.1590634960190723812, -0.9872683547213445543 ) ) ;
#41311 = ORIENTED_EDGE ( 'NONE', *, *, #38389, .T. ) ;
#41312 = EDGE_CURVE ( 'NONE', #18784, #18043, #29436, .T. ) ;
#41313 = ORIENTED_EDGE ( 'NONE', *, *, #16943, .F. ) ;
#41314 = CARTESIAN_POINT ( 'NONE',  ( 0.000000000000000000, -23.85344185397275041, 113.5209818126990200 ) ) ;
#41315 = DIRECTION ( 'NONE',  ( -1.000000000000000000, -0.000000000000000000, 0.000000000000000000 ) ) ;
#41316 = AXIS2_PLACEMENT_3D ( 'NONE', #27204, #40035, #10169 ) ;
#41317 = EDGE_LOOP ( 'NONE', ( #27267, #19849, #29640, #22677 ) ) ;
#41319 = ORIENTED_EDGE ( 'NONE', *, *, #36621, .T. ) ;
#41318 = DIRECTION ( 'NONE',  ( 0.000000000000000000, 0.000000000000000000, -1.000000000000000000 ) ) ;
#41320 = CARTESIAN_POINT ( 'NONE',  ( -40.32452739092001792, 31.00000000000000355, -13.76986825753265897 ) ) ;
#41321 = CARTESIAN_POINT ( 'NONE',  ( 9.000000000000001776, -98.69720329640912837, -60.94966826380012037 ) ) ;
#41322 =( GEOMETRIC_REPRESENTATION_CONTEXT ( 3 ) GLOBAL_UNCERTAINTY_ASSIGNED_CONTEXT ( ( #16966 ) ) GLOBAL_UNIT_ASSIGNED_CONTEXT ( ( #5131, #30205, #26077 ) ) REPRESENTATION_CONTEXT ( 'NONE', 'WORKASPACE' ) );
#41324 = CARTESIAN_POINT ( 'NONE',  ( 17.99999999999999645, 117.9424311864589185, 24.69967462999075281 ) ) ;
#41323 = CARTESIAN_POINT ( 'NONE',  ( 18.00000000000000355, -27.43636312076294814, -38.14186064215179073 ) ) ;
#41325 = ORIENTED_EDGE ( 'NONE', *, *, #17492, .T. ) ;
#41326 = FACE_OUTER_BOUND ( 'NONE', #30726, .T. ) ;
#41328 = CARTESIAN_POINT ( 'NONE',  ( 40.05902963217418744, 40.00000000000000000, -52.04757428485088866 ) ) ;
#41327 = AXIS2_PLACEMENT_3D ( 'NONE', #26560, #10402, #37214 ) ;
#41329 = CARTESIAN_POINT ( 'NONE',  ( 104.9999999999993321, -2.293336392629658115E-13, -32.00000000000000000 ) ) ;
#41330 = ADVANCED_FACE ( 'NONE', ( #34530 ), #18018, .F. ) ;
#41331 = CYLINDRICAL_SURFACE ( 'NONE', #18646, 4.500000000000000888 ) ;
#41332 = ORIENTED_EDGE ( 'NONE', *, *, #32426, .F. ) ;
#41333 = FACE_OUTER_BOUND ( 'NONE', #12752, .T. ) ;
#41334 = AXIS2_PLACEMENT_3D ( 'NONE', #20553, #37732, #33822 ) ;
#41335 = VERTEX_POINT ( 'NONE', #31924 ) ;
#41336 = DIRECTION ( 'NONE',  ( -3.996523416598930318E-16, 2.658563593772947863E-15, 1.000000000000000000 ) ) ;
#41337 = FACE_OUTER_BOUND ( 'NONE', #23042, .T. ) ;
#41338 = AXIS2_PLACEMENT_3D ( 'NONE', #8790, #32139, #35802 ) ;
#41339 = CARTESIAN_POINT ( 'NONE',  ( 55.68207322489292466, 31.00000000000000000, -32.16283696845439266 ) ) ;
#41340 = CARTESIAN_POINT ( 'NONE',  ( 0.000000000000000000, -111.2559044912522950, -32.83479428644788811 ) ) ;
#41341 = VERTEX_POINT ( 'NONE', #8560 ) ;
#41342 = CIRCLE ( 'NONE', #3700, 116.0000000000000000 ) ;
#41343 = EDGE_CURVE ( 'NONE', #35191, #39524, #10608, .T. ) ;
#41344 =( LENGTH_UNIT ( ) NAMED_UNIT ( * ) SI_UNIT ( .MILLI., .METRE. ) );
#41345 = AXIS2_PLACEMENT_3D ( 'NONE', #41697, #1980, #8750 ) ;
#41346 = ADVANCED_FACE ( 'NONE', ( #5074 ), #21094, .T. ) ;
#41347 = ORIENTED_EDGE ( 'NONE', *, *, #42719, .F. ) ;
#41348 = CARTESIAN_POINT ( 'NONE',  ( 17.99999999999999645, 0.000000000000000000, 0.000000000000000000 ) ) ;
#41349 = DIRECTION ( 'NONE',  ( -1.000000000000000000, -0.000000000000000000, -0.000000000000000000 ) ) ;
#41350 = CARTESIAN_POINT ( 'NONE',  ( 82.09539989324809994, 31.00000000000000000, -27.75477508811727390 ) ) ;
#41351 = CARTESIAN_POINT ( 'NONE',  ( 68.41293481152064260, 39.99999999999999289, -52.34142988144959219 ) ) ;
#41352 = EDGE_CURVE ( 'NONE', #33690, #27845, #809, .T. ) ;
#41353 = DIRECTION ( 'NONE',  ( 0.000000000000000000, 1.000000000000000000, -1.287488025362403787E-15 ) ) ;
#41354 =( GEOMETRIC_REPRESENTATION_CONTEXT ( 3 ) GLOBAL_UNCERTAINTY_ASSIGNED_CONTEXT ( ( #26984 ) ) GLOBAL_UNIT_ASSIGNED_CONTEXT ( ( #211, #29726, #19497 ) ) REPRESENTATION_CONTEXT ( 'NONE', 'WORKASPACE' ) );
#41355 = EDGE_LOOP ( 'NONE', ( #23752, #25431, #38799, #11266 ) ) ;
#41356 = FACE_OUTER_BOUND ( 'NONE', #4729, .T. ) ;
#41357 = ORIENTED_EDGE ( 'NONE', *, *, #39657, .F. ) ;
#41358 = AXIS2_PLACEMENT_3D ( 'NONE', #25254, #5989, #28728 ) ;
#41359 = FACE_OUTER_BOUND ( 'NONE', #36242, .T. ) ;
#41361 = EDGE_LOOP ( 'NONE', ( #4267, #41092, #36247, #35708 ) ) ;
#41360 = DIRECTION ( 'NONE',  ( -1.000000000000000000, -0.000000000000000000, 0.000000000000000000 ) ) ;
#41362 = DIRECTION ( 'NONE',  ( -1.000000000000000000, 0.000000000000000000, 0.000000000000000000 ) ) ;
#41363 = ORIENTED_EDGE ( 'NONE', *, *, #36071, .F. ) ;
#41364 = CARTESIAN_POINT ( 'NONE',  ( 17.99999999999999645, -23.10276247328019039, -118.2656051737072431 ) ) ;
#41365 = AXIS2_PLACEMENT_3D ( 'NONE', #10752, #4180, #34094 ) ;
#41366 = CARTESIAN_POINT ( 'NONE',  ( 74.70319961851696178, 39.99999999999999289, -57.31929289364909152 ) ) ;
#41367 = CARTESIAN_POINT ( 'NONE',  ( 17.99999999999999645, -112.5120133921110295, 43.14554256760978745 ) ) ;
#41368 = EDGE_CURVE ( 'NONE', #24289, #42039, #30799, .T. ) ;
#41369 = AXIS2_PLACEMENT_3D ( 'NONE', #39792, #24783, #34554 ) ;
#41370 = ORIENTED_EDGE ( 'NONE', *, *, #21188, .F. ) ;
#41371 = CARTESIAN_POINT ( 'NONE',  ( 18.00000000000000355, 0.000000000000000000, 0.000000000000000000 ) ) ;
#41372 = CARTESIAN_POINT ( 'NONE',  ( 0.000000000000000000, 5.456439917446431309, -112.0647122740741253 ) ) ;
#41373 = AXIS2_PLACEMENT_3D ( 'NONE', #8956, #5670, #22305 ) ;
#41375 = CARTESIAN_POINT ( 'NONE',  ( 8.999999999999998224, 24.70533337038223110, 26.18485254986702060 ) ) ;
#41374 = DIRECTION ( 'NONE',  ( 1.000000000000000000, 0.000000000000000000, -3.273063162220425331E-16 ) ) ;
#41376 = AXIS2_PLACEMENT_3D ( 'NONE', #15703, #29430, #19204 ) ;
#41377 = VERTEX_POINT ( 'NONE', #41726 ) ;
#41378 = DIRECTION ( 'NONE',  ( 0.000000000000000000, 1.000000000000000000, -1.060184893785364939E-15 ) ) ;
#41379 = VERTEX_POINT ( 'NONE', #11868 ) ;
#41380 = CARTESIAN_POINT ( 'NONE',  ( -91.96080130434580724, -12.05525454449572109, 14.45886780445738218 ) ) ;
#41381 = CARTESIAN_POINT ( 'NONE',  ( 21.72498709343026846, 40.00000000000000000, -28.22316639787646864 ) ) ;
#41382 = DIRECTION ( 'NONE',  ( -1.000000000000000000, 0.000000000000000000, 0.000000000000000000 ) ) ;
#41383 = CARTESIAN_POINT ( 'NONE',  ( 67.80287614962797704, -12.05525454449572464, 69.29271901957280022 ) ) ;
#41384 = CARTESIAN_POINT ( 'NONE',  ( 17.99999999999999645, 78.75547124681493472, -91.20343606296920314 ) ) ;
#41385 = ORIENTED_EDGE ( 'NONE', *, *, #36929, .T. ) ;
#41387 = CARTESIAN_POINT ( 'NONE',  ( 2.712762565639649015, -3.052587955997662306, -3.430618716626630871 ) ) ;
#41386 = CARTESIAN_POINT ( 'NONE',  ( 18.00000000000000355, 13.56094713063641244, -50.20060470671726449 ) ) ;
#41388 = EDGE_CURVE ( 'NONE', #7662, #35337, #7918, .T. ) ;
#41389 = AXIS2_PLACEMENT_3D ( 'NONE', #26666, #16664, #24060 ) ;
#41390 = ORIENTED_EDGE ( 'NONE', *, *, #39601, .F. ) ;
#41391 = CIRCLE ( 'NONE', #29583, 36.00000000000000000 ) ;
#41392 = DIRECTION ( 'NONE',  ( 1.000000000000000000, -0.000000000000000000, -0.000000000000000000 ) ) ;
#41393 = FACE_OUTER_BOUND ( 'NONE', #10531, .T. ) ;
#41394 = CARTESIAN_POINT ( 'NONE',  ( -29.59829689555773058, 31.00000000000000355, 3.906358533625565954 ) ) ;
#41395 = ORIENTED_EDGE ( 'NONE', *, *, #1278, .F. ) ;
#41396 = CARTESIAN_POINT ( 'NONE',  ( 0.000000000000000000, 0.000000000000000000, -6.000000000000000000 ) ) ;
#41397 = DIRECTION ( 'NONE',  ( 0.000000000000000000, -0.8477344278896651319, -0.5304209081197519549 ) ) ;
#41398 = ADVANCED_FACE ( 'NONE', ( #22137, #38441 ), #25397, .F. ) ;
#41399 = AXIS2_PLACEMENT_3D ( 'NONE', #41876, #35116, #8298 ) ;
#41400 = CARTESIAN_POINT ( 'NONE',  ( 17.99999999999999645, 118.8387007424470738, 19.94628303336527608 ) ) ;
#41401 = CARTESIAN_POINT ( 'NONE',  ( -64.44063486737354651, 31.00000000000000711, -49.42892067282641477 ) ) ;
#41402 = AXIS2_PLACEMENT_3D ( 'NONE', #35816, #15588, #5735 ) ;
#41403 = EDGE_CURVE ( 'NONE', #28259, #9950, #31059, .T. ) ;
#41404 = VERTEX_POINT ( 'NONE', #27810 ) ;
#41405 = CARTESIAN_POINT ( 'NONE',  ( 15.22596115864829791, 31.00000000000000355, 57.21640888978779316 ) ) ;
#41406 = VECTOR ( 'NONE', #38778, 1000.000000000000000 ) ;
#41407 = ADVANCED_FACE ( 'NONE', ( #41061 ), #14816, .T. ) ;
#41408 = CARTESIAN_POINT ( 'NONE',  ( -28.35539204363714205, 40.00000000000000000, 83.52787551312086123 ) ) ;
#41409 = CIRCLE ( 'NONE', #11488, 116.0000000000000000 ) ;
#41410 = ORIENTED_EDGE ( 'NONE', *, *, #38340, .F. ) ;
#41411 = CARTESIAN_POINT ( 'NONE',  ( -97.01392236320388918, -2.055254544495720648, 76.75426063221412676 ) ) ;
#41412 = DIRECTION ( 'NONE',  ( 0.000000000000000000, 0.1837495178165638177, 0.9829730996839030066 ) ) ;
#41413 = CARTESIAN_POINT ( 'NONE',  ( 17.99999999999999645, -21.48775762007876367, 23.64423737150130478 ) ) ;
#41415 = ORIENTED_EDGE ( 'NONE', *, *, #75, .F. ) ;
#41414 = CARTESIAN_POINT ( 'NONE',  ( 0.000000000000000000, 0.000000000000000000, 0.000000000000000000 ) ) ;
#41416 = DIRECTION ( 'NONE',  ( 0.000000000000000000, -0.8747630845319658288, 0.4845508703326422140 ) ) ;
#41417 = CARTESIAN_POINT ( 'NONE',  ( -3.996523416598931009E-15, 2.658563593772952281E-14, 10.00000000000000178 ) ) ;
#41418 = CIRCLE ( 'NONE', #11495, 12.59999999999999964 ) ;
#41419 = ORIENTED_EDGE ( 'NONE', *, *, #319, .F. ) ;
#41420 = CARTESIAN_POINT ( 'NONE',  ( -60.10416666555506993, 40.00000000000000711, -3.926990808566252156 ) ) ;
#41421 = CARTESIAN_POINT ( 'NONE',  ( 17.99999999999999645, 0.000000000000000000, 0.000000000000000000 ) ) ;
#41422 = EDGE_CURVE ( 'NONE', #21320, #39191, #34995, .T. ) ;
#41423 = ORIENTED_EDGE ( 'NONE', *, *, #11186, .F. ) ;
#41424 = EDGE_CURVE ( 'NONE', #33606, #33175, #25614, .T. ) ;
#41425 = DIRECTION ( 'NONE',  ( -1.000000000000000000, -0.000000000000000000, -0.000000000000000000 ) ) ;
#41426 = CARTESIAN_POINT ( 'NONE',  ( 0.000000000000000000, 30.71634675606053833, 8.790889055186667633 ) ) ;
#41427 = ORIENTED_EDGE ( 'NONE', *, *, #19704, .F. ) ;
#41428 = CYLINDRICAL_SURFACE ( 'NONE', #3292, 12.55910585664918422 ) ;
#41429 = ORIENTED_EDGE ( 'NONE', *, *, #39159, .F. ) ;
#41430 = CIRCLE ( 'NONE', #9355, 100.0000000000000000 ) ;
#41431 = DIRECTION ( 'NONE',  ( -1.000000000000000000, -0.000000000000000000, 0.000000000000000000 ) ) ;
#41432 = ORIENTED_EDGE ( 'NONE', *, *, #13797, .T. ) ;
#41433 = CIRCLE ( 'NONE', #41464, 116.0000000000000000 ) ;
#41434 = DIRECTION ( 'NONE',  ( 0.000000000000000000, 0.000000000000000000, 1.000000000000000000 ) ) ;
#41435 = DIRECTION ( 'NONE',  ( 1.000000000000000000, 0.000000000000000000, 0.000000000000000000 ) ) ;
#41436 = VERTEX_POINT ( 'NONE', #22766 ) ;
#41437 = CIRCLE ( 'NONE', #30994, 100.0000000000000000 ) ;
#41438 = DIRECTION ( 'NONE',  ( -1.000000000000000000, -0.000000000000000000, -0.000000000000000000 ) ) ;
#41439 = FACE_OUTER_BOUND ( 'NONE', #30390, .T. ) ;
#41440 = EDGE_LOOP ( 'NONE', ( #20203, #523, #36868, #17274 ) ) ;
#41441 = DIRECTION ( 'NONE',  ( 0.000000000000000000, 0.000000000000000000, 1.000000000000000000 ) ) ;
#41442 = EDGE_CURVE ( 'NONE', #30953, #37795, #37755, .T. ) ;
#41443 = AXIS2_PLACEMENT_3D ( 'NONE', #3141, #3573, #16516 ) ;
#41444 = DIRECTION ( 'NONE',  ( -1.000000000000000000, -0.000000000000000000, -0.000000000000000000 ) ) ;
#41445 = ORIENTED_EDGE ( 'NONE', *, *, #19734, .F. ) ;
#41446 = DIRECTION ( 'NONE',  ( 0.000000000000000000, 0.000000000000000000, 1.000000000000000000 ) ) ;
#41447 = CARTESIAN_POINT ( 'NONE',  ( 17.99999999999999645, 0.000000000000000000, 0.000000000000000000 ) ) ;
#41448 = DIRECTION ( 'NONE',  ( -1.000000000000000000, 0.000000000000000000, 1.047444401652940007E-14 ) ) ;
#41449 = EDGE_CURVE ( 'NONE', #37862, #26858, #6354, .T. ) ;
#41450 = CARTESIAN_POINT ( 'NONE',  ( 18.00000000000000355, -17.50309955389642269, 43.60271849949357659 ) ) ;
#41451 = CARTESIAN_POINT ( 'NONE',  ( 3.108867721649529958, 31.00000000000000355, 47.39583333474234905 ) ) ;
#41452 = ORIENTED_EDGE ( 'NONE', *, *, #8317, .F. ) ;
#41454 = DIRECTION ( 'NONE',  ( 0.000000000000000000, 0.000000000000000000, 1.000000000000000000 ) ) ;
#41453 = CARTESIAN_POINT ( 'NONE',  ( -2.600000000000000533, -12.75000000000000000, -1.199999999999999956 ) ) ;
#41455 = EDGE_CURVE ( 'NONE', #15184, #16399, #5035, .T. ) ;
#41456 = VERTEX_POINT ( 'NONE', #18867 ) ;
#41457 = EDGE_CURVE ( 'NONE', #28923, #13830, #3601, .T. ) ;
#41458 = ADVANCED_FACE ( 'NONE', ( #19492 ), #23195, .F. ) ;
#41459 = DIRECTION ( 'NONE',  ( 1.000000000000000000, 0.000000000000000000, 0.000000000000000000 ) ) ;
#41460 = CARTESIAN_POINT ( 'NONE',  ( -56.43872490705654599, 40.00000000000000711, 19.17141758012168751 ) ) ;
#41461 = AXIS2_PLACEMENT_3D ( 'NONE', #26122, #35690, #19167 ) ;
#41462 = CARTESIAN_POINT ( 'NONE',  ( 29.31577600748121881, 40.00000000000000000, 50.95836110724019363 ) ) ;
#41463 = VECTOR ( 'NONE', #13816, 1000.000000000000000 ) ;
#41464 = AXIS2_PLACEMENT_3D ( 'NONE', #13076, #39849, #20068 ) ;
#41465 = DIRECTION ( 'NONE',  ( 1.000000000000000000, 0.000000000000000000, 0.000000000000000000 ) ) ;
#41466 = CIRCLE ( 'NONE', #17096, 59.00000000000000711 ) ;
#41467 = CARTESIAN_POINT ( 'NONE',  ( 0.000000000000000000, 0.000000000000000000, 0.000000000000000000 ) ) ;
#41468 = AXIS2_PLACEMENT_3D ( 'NONE', #27376, #33472, #3556 ) ;
#41469 = LINE ( 'NONE', #11187, #21884 ) ;
#41470 = CARTESIAN_POINT ( 'NONE',  ( 10.28773449565296083, 31.00000000000000355, -20.88174966193524895 ) ) ;
#41471 = ORIENTED_EDGE ( 'NONE', *, *, #6837, .T. ) ;
#41472 = CARTESIAN_POINT ( 'NONE',  ( 9.621748599878955588, 40.00000000000000000, 35.89595399306684698 ) ) ;
#41473 = VERTEX_POINT ( 'NONE', #26016 ) ;
#41474 = LINE ( 'NONE', #40823, #11099 ) ;
#41475 = ADVANCED_FACE ( 'NONE', ( #36231 ), #36021, .T. ) ;
#41476 = ORIENTED_EDGE ( 'NONE', *, *, #1490, .F. ) ;
#41477 = EDGE_CURVE ( 'NONE', #28172, #20222, #2841, .T. ) ;
#41478 = DIRECTION ( 'NONE',  ( 0.9997917317482359900, -0.02040816326530612776, 0.000000000000000000 ) ) ;
#41479 = ADVANCED_FACE ( 'NONE', ( #5920, #8998 ), #35594, .F. ) ;
#41480 = ADVANCED_FACE ( 'NONE', ( #32127 ), #2636, .T. ) ;
#41481 = DIRECTION ( 'NONE',  ( -1.000000000000000000, -0.000000000000000000, -0.000000000000000000 ) ) ;
#41482 = ORIENTED_EDGE ( 'NONE', *, *, #27229, .T. ) ;
#41483 = CARTESIAN_POINT ( 'NONE',  ( 3.511755186886750923, -2.826662030176382956, -3.597382984111582083 ) ) ;
#41484 = VERTEX_POINT ( 'NONE', #42766 ) ;
#41485 = VERTEX_POINT ( 'NONE', #15998 ) ;
#41486 = CARTESIAN_POINT ( 'NONE',  ( 8.999999999999998224, 12.42760411676086996, -33.78690065568411427 ) ) ;
#41487 = CARTESIAN_POINT ( 'NONE',  ( -43.11175393642376008, 31.00000000000000355, 56.02072642018850246 ) ) ;
#41488 = ORIENTED_EDGE ( 'NONE', *, *, #41368, .T. ) ;
#41489 = FACE_OUTER_BOUND ( 'NONE', #32059, .T. ) ;
#41490 = AXIS2_PLACEMENT_3D ( 'NONE', #11006, #14069, #7490 ) ;
#41492 = DIRECTION ( 'NONE',  ( 0.000000000000000000, -0.8951632913550570114, -0.4457383557765488558 ) ) ;
#41491 = AXIS2_PLACEMENT_3D ( 'NONE', #24930, #7430, #646 ) ;
#41493 = ORIENTED_EDGE ( 'NONE', *, *, #20420, .F. ) ;
#41494 = AXIS2_PLACEMENT_3D ( 'NONE', #10849, #23957, #33322 ) ;
#41495 = CARTESIAN_POINT ( 'NONE',  ( 18.00000000000000355, -36.06787431788703913, 37.45808914225474950 ) ) ;
#41496 = EDGE_LOOP ( 'NONE', ( #13674, #28506, #19137, #2729 ) ) ;
#41497 = CARTESIAN_POINT ( 'NONE',  ( 96.56285295106285105, 39.99999999999999289, 12.84127866192819312 ) ) ;
#41498 = CARTESIAN_POINT ( 'NONE',  ( -13.43146050690766380, 31.00000000000000355, 27.15249184975281693 ) ) ;
#41499 = VECTOR ( 'NONE', #21618, 1000.000000000000000 ) ;
#41501 = DIRECTION ( 'NONE',  ( -1.000000000000000000, 0.000000000000000000, -0.000000000000000000 ) ) ;
#41500 = CARTESIAN_POINT ( 'NONE',  ( 158.5000000000000284, 0.000000000000000000, 6.999999999999998224 ) ) ;
#41502 = AXIS2_PLACEMENT_3D ( 'NONE', #2436, #35814, #40109 ) ;
#41503 = AXIS2_PLACEMENT_3D ( 'NONE', #23268, #17538, #888 ) ;
#41504 = DIRECTION ( 'NONE',  ( 0.000000000000000000, 0.000000000000000000, 1.000000000000000000 ) ) ;
#41505 = CARTESIAN_POINT ( 'NONE',  ( -8.920000000000003482, 0.000000000000000000, 11.00000000000000000 ) ) ;
#41506 = ORIENTED_EDGE ( 'NONE', *, *, #28452, .T. ) ;
#41507 = FILL_AREA_STYLE_COLOUR ( '', #37871 ) ;
#41508 = VECTOR ( 'NONE', #23554, 1000.000000000000000 ) ;
#41509 = ADVANCED_FACE ( 'NONE', ( #12923 ), #3046, .T. ) ;
#41510 = CARTESIAN_POINT ( 'NONE',  ( 17.99999999999999645, 64.69195966009891663, 96.28577441832274530 ) ) ;
#41511 = ORIENTED_EDGE ( 'NONE', *, *, #39057, .F. ) ;
#41512 = DIRECTION ( 'NONE',  ( -1.000000000000000000, 0.000000000000000000, 0.000000000000000000 ) ) ;
#41513 = CARTESIAN_POINT ( 'NONE',  ( 61.87885091699251916, 31.00000000000000000, -70.55635664373320992 ) ) ;
#41514 = DIRECTION ( 'NONE',  ( -1.000000000000000000, 0.000000000000000000, -0.000000000000000000 ) ) ;
#41515 = ORIENTED_EDGE ( 'NONE', *, *, #7199, .F. ) ;
#41516 = CARTESIAN_POINT ( 'NONE',  ( 1.622176940739286310, 40.00000000000000000, -24.60292901074089045 ) ) ;
#41517 = ORIENTED_EDGE ( 'NONE', *, *, #17271, .F. ) ;
#41518 = ORIENTED_EDGE ( 'NONE', *, *, #24612, .T. ) ;
#41519 = CYLINDRICAL_SURFACE ( 'NONE', #9529, 59.00000000000000000 ) ;
#41520 = DIRECTION ( 'NONE',  ( -1.000000000000000000, -0.000000000000000000, -0.000000000000000000 ) ) ;
#41522 = DIRECTION ( 'NONE',  ( -1.000000000000000000, -0.000000000000000000, 0.000000000000000000 ) ) ;
#41521 = AXIS2_PLACEMENT_3D ( 'NONE', #8354, #37801, #41728 ) ;
#41523 = DIRECTION ( 'NONE',  ( 0.000000000000000000, 0.000000000000000000, 1.000000000000000000 ) ) ;
#41524 = VECTOR ( 'NONE', #24436, 1000.000000000000000 ) ;
#41525 = AXIS2_PLACEMENT_3D ( 'NONE', #34209, #27251, #30944 ) ;
#41526 = CIRCLE ( 'NONE', #12284, 59.00000000000001421 ) ;
#41527 = VERTEX_POINT ( 'NONE', #35793 ) ;
#41528 = CARTESIAN_POINT ( 'NONE',  ( 0.000000000000000000, 0.000000000000000000, 0.000000000000000000 ) ) ;
#41529 = ORIENTED_EDGE ( 'NONE', *, *, #8749, .F. ) ;
#41530 = CARTESIAN_POINT ( 'NONE',  ( 17.99999999999999645, 93.26762629039428987, 76.29967815892386795 ) ) ;
#41531 = CARTESIAN_POINT ( 'NONE',  ( 17.99999999999999645, -40.13512380273891011, -113.6206972269525863 ) ) ;
#41532 = AXIS2_PLACEMENT_3D ( 'NONE', #4871, #18236, #5518 ) ;
#41533 = CIRCLE ( 'NONE', #18585, 158.5000000000000284 ) ;
#41534 = EDGE_CURVE ( 'NONE', #29429, #17680, #39079, .T. ) ;
#41535 = AXIS2_PLACEMENT_3D ( 'NONE', #41411, #41849, #34880 ) ;
#41536 = DIRECTION ( 'NONE',  ( 1.000000000000000000, 0.000000000000000000, 0.000000000000000000 ) ) ;
#41537 = ADVANCED_FACE ( 'NONE', ( #42995 ), #15779, .T. ) ;
#41538 = EDGE_CURVE ( 'NONE', #21041, #21374, #21785, .T. ) ;
#41539 = AXIS2_PLACEMENT_3D ( 'NONE', #42353, #39078, #32549 ) ;
#41540 = DIRECTION ( 'NONE',  ( 0.000000000000000000, 0.000000000000000000, 1.000000000000000000 ) ) ;
#41541 = EDGE_LOOP ( 'NONE', ( #39030, #1824, #20086, #34095 ) ) ;
#41542 = EDGE_LOOP ( 'NONE', ( #2311, #16323, #5235, #26976 ) ) ;
#41543 = DIRECTION ( 'NONE',  ( 0.000000000000000000, 0.6783118362696123338, 0.7347741508630706297 ) ) ;
#41544 = CYLINDRICAL_SURFACE ( 'NONE', #10979, 2.649999999999993694 ) ;
#41545 = ADVANCED_FACE ( 'NONE', ( #4146 ), #10285, .T. ) ;
#41546 = CIRCLE ( 'NONE', #27650, 13.59999999999999964 ) ;
#41547 = ORIENTED_EDGE ( 'NONE', *, *, #28685, .T. ) ;
#41549 = EDGE_LOOP ( 'NONE', ( #35855, #41172, #2866, #40229 ) ) ;
#41548 = CARTESIAN_POINT ( 'NONE',  ( 0.000000000000000000, -42.87700105098536341, -107.7847984684009219 ) ) ;
#41550 = CARTESIAN_POINT ( 'NONE',  ( 2.511863649308172519, 31.00000000000000355, 39.39933062586388957 ) ) ;
#41551 = ORIENTED_EDGE ( 'NONE', *, *, #19819, .T. ) ;
#41552 = FACE_OUTER_BOUND ( 'NONE', #15677, .T. ) ;
#41554 = DIRECTION ( 'NONE',  ( -3.996523416598930318E-16, 2.658563593772947863E-15, 1.000000000000000000 ) ) ;
#41553 = CARTESIAN_POINT ( 'NONE',  ( 17.99999999999999645, -114.6488492393077081, -37.09625815500128709 ) ) ;
#41555 = ORIENTED_EDGE ( 'NONE', *, *, #35966, .F. ) ;
#41556 = CARTESIAN_POINT ( 'NONE',  ( -15.99999999999997691, 17.11489954122026447, 5.571627607371296764E-15 ) ) ;
#41557 = CARTESIAN_POINT ( 'NONE',  ( 45.08926718327026606, 40.00000000000000000, 51.56349680124436219 ) ) ;
#41558 = AXIS2_PLACEMENT_3D ( 'NONE', #11086, #21146, #17872 ) ;
#41559 = CARTESIAN_POINT ( 'NONE',  ( 0.000000000000000000, 0.000000000000000000, 0.000000000000000000 ) ) ;
#41560 = AXIS2_PLACEMENT_3D ( 'NONE', #18393, #17970, #25153 ) ;
#41561 = DIRECTION ( 'NONE',  ( 0.000000000000000000, -2.128711519673234442E-14, -1.000000000000000000 ) ) ;
#41563 = ORIENTED_EDGE ( 'NONE', *, *, #2238, .T. ) ;
#41562 = AXIS2_PLACEMENT_3D ( 'NONE', #31591, #11535, #24881 ) ;
#41564 = CARTESIAN_POINT ( 'NONE',  ( 0.000000000000000000, 0.000000000000000000, 0.000000000000000000 ) ) ;
#41565 = VECTOR ( 'NONE', #9271, 1000.000000000000000 ) ;
#41566 = ORIENTED_EDGE ( 'NONE', *, *, #33457, .F. ) ;
#41567 =( NAMED_UNIT ( * ) PLANE_ANGLE_UNIT ( ) SI_UNIT ( $, .RADIAN. ) );
#41568 = AXIS2_PLACEMENT_3D ( 'NONE', #9434, #39525, #9660 ) ;
#41569 = DIRECTION ( 'NONE',  ( 1.000000000000000000, 0.000000000000000000, 0.000000000000000000 ) ) ;
#41570 = CARTESIAN_POINT ( 'NONE',  ( 8.999999999999998224, 82.63181128086846172, -81.41243003646886223 ) ) ;
#41571 = CARTESIAN_POINT ( 'NONE',  ( -53.60515337853228601, 31.00000000000000355, -47.01024902908782366 ) ) ;
#41572 = CARTESIAN_POINT ( 'NONE',  ( 17.99999999999999645, -19.69434969228090893, 24.58291258574042004 ) ) ;
#41574 = ORIENTED_EDGE ( 'NONE', *, *, #17496, .F. ) ;
#41573 = VECTOR ( 'NONE', #15245, 1000.000000000000000 ) ;
#41575 = AXIS2_PLACEMENT_3D ( 'NONE', #33825, #21866, #15314 ) ;
#41576 = VECTOR ( 'NONE', #12556, 1000.000000000000000 ) ;
#41577 = ORIENTED_EDGE ( 'NONE', *, *, #39376, .F. ) ;
#41578 = DIRECTION ( 'NONE',  ( 0.000000000000000000, 0.3140767120219429276, 0.9493976084683832806 ) ) ;
#41579 = DIRECTION ( 'NONE',  ( 1.000000000000000000, 1.836909530733573776E-16, 0.000000000000000000 ) ) ;
#41580 = CARTESIAN_POINT ( 'NONE',  ( -71.82650799747224823, 31.00000000000000711, -41.60779115368423220 ) ) ;
#41581 = CARTESIAN_POINT ( 'NONE',  ( -79.74759331938361129, 40.00000000000000711, -21.47736420602193874 ) ) ;
#41582 = LINE ( 'NONE', #24406, #33424 ) ;
#41583 = ORIENTED_EDGE ( 'NONE', *, *, #2075, .T. ) ;
#41584 = CARTESIAN_POINT ( 'NONE',  ( -23.00000000000000000, 0.000000000000000000, -6.000000000000000000 ) ) ;
#41585 = ORIENTED_EDGE ( 'NONE', *, *, #15910, .T. ) ;
#41586 = CARTESIAN_POINT ( 'NONE',  ( 17.99999999999999645, 111.2559044912529345, -32.83479428644565701 ) ) ;
#41587 = DIRECTION ( 'NONE',  ( 0.000000000000000000, 0.3681245526846786964, -0.9297764858882511252 ) ) ;
#41588 = VECTOR ( 'NONE', #24134, 1000.000000000000000 ) ;
#41590 = EDGE_LOOP ( 'NONE', ( #9848, #20963, #33699, #28996 ) ) ;
#41589 = CARTESIAN_POINT ( 'NONE',  ( 18.00000000000000355, -44.47301969247432396, -16.68249143361957465 ) ) ;
#41591 = EDGE_CURVE ( 'NONE', #23465, #38913, #30360, .T. ) ;
#41592 = CARTESIAN_POINT ( 'NONE',  ( 17.99999999999999645, -109.4038418350907023, 50.51029986767514401 ) ) ;
#41593 = ORIENTED_EDGE ( 'NONE', *, *, #14298, .F. ) ;
#41594 = DIRECTION ( 'NONE',  ( 0.000000000000000000, 0.000000000000000000, 1.000000000000000000 ) ) ;
#41595 = VECTOR ( 'NONE', #33391, 1000.000000000000000 ) ;
#41596 = EDGE_CURVE ( 'NONE', #27814, #28643, #41927, .T. ) ;
#41597 = CARTESIAN_POINT ( 'NONE',  ( 94.17930118497612568, 39.99999999999999289, -12.41473344271720691 ) ) ;
#41598 = CARTESIAN_POINT ( 'NONE',  ( -2.500000000000000444, 3.061616997868383634E-16, -5.000000000000000888 ) ) ;
#41599 = AXIS2_PLACEMENT_3D ( 'NONE', #24954, #27991, #8745 ) ;
#41600 = VECTOR ( 'NONE', #20662, 1000.000000000000000 ) ;
#41601 = ORIENTED_EDGE ( 'NONE', *, *, #22669, .F. ) ;
#41602 = LINE ( 'NONE', #17880, #6691 ) ;
#41603 = DIRECTION ( 'NONE',  ( 0.000000000000000000, 0.000000000000000000, 1.000000000000000000 ) ) ;
#41604 = CIRCLE ( 'NONE', #19347, 51.99999999999999289 ) ;
#41605 = EDGE_CURVE ( 'NONE', #23084, #39350, #34273, .T. ) ;
#41606 = AXIS2_PLACEMENT_3D ( 'NONE', #33191, #29290, #26657 ) ;
#41608 = DIRECTION ( 'NONE',  ( -3.009274222672345096E-17, -1.000000000000000000, 2.455023325076454960E-18 ) ) ;
#41607 = LINE ( 'NONE', #37891, #732 ) ;
#41609 = ORIENTED_EDGE ( 'NONE', *, *, #11123, .F. ) ;
#41610 = CARTESIAN_POINT ( 'NONE',  ( 18.00000000000000355, 31.08872492059957793, 41.68322423723109438 ) ) ;
#41611 = ORIENTED_EDGE ( 'NONE', *, *, #15485, .F. ) ;
#41612 = CARTESIAN_POINT ( 'NONE',  ( 17.99999999999999645, 30.01658535635412406, -108.1077105353194838 ) ) ;
#41613 = CARTESIAN_POINT ( 'NONE',  ( 14.33709021557830887, 40.00000000000000000, 24.89380824183666618 ) ) ;
#41614 = CARTESIAN_POINT ( 'NONE',  ( 17.99999999999999645, 0.000000000000000000, 0.000000000000000000 ) ) ;
#41615 = AXIS2_PLACEMENT_3D ( 'NONE', #28235, #31495, #1368 ) ;
#41616 = EDGE_CURVE ( 'NONE', #26508, #28297, #8522, .T. ) ;
#41617 = CARTESIAN_POINT ( 'NONE',  ( 0.000000000000000000, 0.000000000000000000, -20.00000000000000000 ) ) ;
#41618 = DIRECTION ( 'NONE',  ( 0.000000000000000000, 0.9510565162951544194, -0.3090169943749448422 ) ) ;
#41619 = ORIENTED_EDGE ( 'NONE', *, *, #27583, .T. ) ;
#41620 = CARTESIAN_POINT ( 'NONE',  ( 17.99999999999999645, -110.8621702203451065, 34.14058016547499363 ) ) ;
#41621 = ORIENTED_EDGE ( 'NONE', *, *, #28638, .T. ) ;
#41622 = CARTESIAN_POINT ( 'NONE',  ( 0.000000000000000000, 29.68570942776472066, 10.53307442156944873 ) ) ;
#41623 = DIRECTION ( 'NONE',  ( 0.000000000000000000, 0.4610925014493207352, 0.8873520750565742077 ) ) ;
#41624 = CARTESIAN_POINT ( 'NONE',  ( 9.621748599878955588, 31.00000000000000355, 35.89595399306684698 ) ) ;
#41626 = EDGE_LOOP ( 'NONE', ( #12329, #34364 ) ) ;
#41625 = AXIS2_PLACEMENT_3D ( 'NONE', #30662, #10140, #76 ) ;
#41627 = DIRECTION ( 'NONE',  ( 0.000000000000000000, 0.000000000000000000, 1.000000000000000000 ) ) ;
#41628 = VECTOR ( 'NONE', #8107, 1000.000000000000000 ) ;
#41629 = CIRCLE ( 'NONE', #13100, 120.5010000000000474 ) ;
#41630 = CARTESIAN_POINT ( 'NONE',  ( 17.99999999999999645, 78.18175027177548486, -85.69488855492920720 ) ) ;
#41631 = CARTESIAN_POINT ( 'NONE',  ( -59.40286837853895463, 31.00000000000000711, 52.11376356991771530 ) ) ;
#41632 = CIRCLE ( 'NONE', #15875, 100.0000000000000000 ) ;
#41633 = CIRCLE ( 'NONE', #33972, 20.00000000000000711 ) ;
#41634 = AXIS2_PLACEMENT_3D ( 'NONE', #5336, #18473, #15403 ) ;
#41635 = ORIENTED_EDGE ( 'NONE', *, *, #41424, .F. ) ;
#41637 = CARTESIAN_POINT ( 'NONE',  ( 48.78760054486801323, 31.00000000000000355, -28.06521077754944926 ) ) ;
#41636 = AXIS2_PLACEMENT_3D ( 'NONE', #14960, #42161, #35424 ) ;
#41638 = CARTESIAN_POINT ( 'NONE',  ( -39.09256291070916944, 40.00000000000000000, 79.30589209199378331 ) ) ;
#41639 = ORIENTED_EDGE ( 'NONE', *, *, #24045, .T. ) ;
#41640 = DIRECTION ( 'NONE',  ( -0.000000000000000000, -0.000000000000000000, 1.000000000000000000 ) ) ;
#41641 = AXIS2_PLACEMENT_3D ( 'NONE', #4972, #25503, #28119 ) ;
#41642 = DIRECTION ( 'NONE',  ( 0.000000000000000000, 0.2113826236296247885, -0.9774033898178665636 ) ) ;
#41643 = FACE_OUTER_BOUND ( 'NONE', #7286, .T. ) ;
#41645 = ORIENTED_EDGE ( 'NONE', *, *, #38335, .T. ) ;
#41644 = CARTESIAN_POINT ( 'NONE',  ( 0.000000000000000000, -5.492704054965900973, -115.8698847939556771 ) ) ;
#41646 = ADVANCED_FACE ( 'NONE', ( #26658 ), #653, .T. ) ;
#41647 = CYLINDRICAL_SURFACE ( 'NONE', #22625, 20.00000000000000711 ) ;
#41648 = CYLINDRICAL_SURFACE ( 'NONE', #31397, 116.0000000000000000 ) ;
#41649 = EDGE_CURVE ( 'NONE', #30521, #17817, #2910, .T. ) ;
#41650 = VERTEX_POINT ( 'NONE', #3490 ) ;
#41651 = CARTESIAN_POINT ( 'NONE',  ( 28.01378275134445772, 40.00000000000000000, -56.83506808085938644 ) ) ;
#41652 = DIRECTION ( 'NONE',  ( -1.000000000000000000, 0.000000000000000000, 0.000000000000000000 ) ) ;
#41653 = EDGE_LOOP ( 'NONE', ( #23, #27550, #20928, #42173 ) ) ;
#41654 = AXIS2_PLACEMENT_3D ( 'NONE', #36699, #23017, #33646 ) ;
#41655 = CARTESIAN_POINT ( 'NONE',  ( 18.00000000000000355, 0.000000000000000000, 0.000000000000000000 ) ) ;
#41656 = DIRECTION ( 'NONE',  ( 0.000000000000000000, 0.000000000000000000, 1.000000000000000000 ) ) ;
#41657 = DIRECTION ( 'NONE',  ( -1.000000000000000000, 0.000000000000000000, 0.000000000000000000 ) ) ;
#41658 = VERTEX_POINT ( 'NONE', #440 ) ;
#41659 = EDGE_CURVE ( 'NONE', #35211, #33710, #23402, .T. ) ;
#41660 = CIRCLE ( 'NONE', #9614, 13.60000000000000320 ) ;
#41661 = VERTEX_POINT ( 'NONE', #14010 ) ;
#41662 = CIRCLE ( 'NONE', #37490, 116.0000000000000000 ) ;
#41663 = DIRECTION ( 'NONE',  ( -3.009274222672345096E-17, -1.000000000000000000, 2.455023325076454960E-18 ) ) ;
#41664 = EDGE_LOOP ( 'NONE', ( #626, #37581, #9400, #4929 ) ) ;
#41665 = AXIS2_PLACEMENT_3D ( 'NONE', #22857, #70, #13441 ) ;
#41666 = FACE_OUTER_BOUND ( 'NONE', #33360, .T. ) ;
#41667 = FACE_OUTER_BOUND ( 'NONE', #688, .T. ) ;
#41668 = ADVANCED_FACE ( 'NONE', ( #33615 ), #3698, .F. ) ;
#41669 = CIRCLE ( 'NONE', #543, 120.5010000000000190 ) ;
#41670 = DIRECTION ( 'NONE',  ( 0.000000000000000000, 0.8660254037844380415, -0.5000000000000009992 ) ) ;
#41671 = DIRECTION ( 'NONE',  ( 0.000000000000000000, 0.000000000000000000, 1.000000000000000000 ) ) ;
#41672 = VERTEX_POINT ( 'NONE', #23631 ) ;
#41673 = FACE_BOUND ( 'NONE', #34573, .T. ) ;
#41674 = DIRECTION ( 'NONE',  ( 1.000000000000000000, -0.000000000000000000, -0.000000000000000000 ) ) ;
#41675 = ORIENTED_EDGE ( 'NONE', *, *, #16912, .F. ) ;
#41676 = DIRECTION ( 'NONE',  ( 0.000000000000000000, 1.243708525996931132E-14, -1.000000000000000000 ) ) ;
#41677 = VECTOR ( 'NONE', #10392, 999.9999999999998863 ) ;
#41678 = CARTESIAN_POINT ( 'NONE',  ( 17.99999999999999645, 0.000000000000000000, 0.000000000000000000 ) ) ;
#41679 = ADVANCED_FACE ( 'NONE', ( #23838 ), #20149, .F. ) ;
#41680 = CARTESIAN_POINT ( 'NONE',  ( -3.662251155509560450E-15, 17.99999999999998934, -150.5000000000000284 ) ) ;
#41681 = CARTESIAN_POINT ( 'NONE',  ( 0.000000000000000000, 93.26762629039427566, 76.29967815892388217 ) ) ;
#41682 = CARTESIAN_POINT ( 'NONE',  ( -49.88601606984090608, 31.00000000000000355, -6.565487524765669214 ) ) ;
#41683 = ADVANCED_FACE ( 'NONE', ( #6559 ), #33832, .F. ) ;
#41684 = ORIENTED_EDGE ( 'NONE', *, *, #42315, .T. ) ;
#41686 = FACE_OUTER_BOUND ( 'NONE', #40636, .T. ) ;
#41685 = CARTESIAN_POINT ( 'NONE',  ( 17.99999999999999645, 0.000000000000000000, 0.000000000000000000 ) ) ;
#41687 = EDGE_CURVE ( 'NONE', #27790, #5016, #27346, .T. ) ;
#41688 = VECTOR ( 'NONE', #12059, 1000.000000000000000 ) ;
#41689 = VERTEX_POINT ( 'NONE', #33409 ) ;
#41690 = AXIS2_PLACEMENT_3D ( 'NONE', #25328, #12220, #18804 ) ;
#41691 = CARTESIAN_POINT ( 'NONE',  ( -52.79687664379660816, 40.00000000000000000, -30.48099731442381710 ) ) ;
#41692 = VECTOR ( 'NONE', #35718, 1000.000000000000000 ) ;
#41693 = CARTESIAN_POINT ( 'NONE',  ( 67.09393615765254992, 39.99999999999999289, 4.495243625008655819 ) ) ;
#41694 = CIRCLE ( 'NONE', #30567, 11.00000000000000178 ) ;
#41695 = CARTESIAN_POINT ( 'NONE',  ( 0.000000000000000000, -119.0898412705473390, -18.38751498043854227 ) ) ;
#41696 = DIRECTION ( 'NONE',  ( 0.000000000000000000, 0.000000000000000000, 1.000000000000000000 ) ) ;
#41697 = CARTESIAN_POINT ( 'NONE',  ( 17.99999999999999645, 0.000000000000000000, 0.000000000000000000 ) ) ;
#41698 = CARTESIAN_POINT ( 'NONE',  ( 18.00000000000000355, 26.17370628620709638, -39.63700417846136048 ) ) ;
#41699 = EDGE_CURVE ( 'NONE', #4861, #18607, #28075, .T. ) ;
#41700 = VERTEX_POINT ( 'NONE', #36889 ) ;
#41701 = CARTESIAN_POINT ( 'NONE',  ( -4.233603722440171246, 40.00000000000000000, -32.08218167604271542 ) ) ;
#41702 = ORIENTED_EDGE ( 'NONE', *, *, #41944, .T. ) ;
#41703 = DIRECTION ( 'NONE',  ( -1.000000000000000000, 0.000000000000000000, -0.000000000000000000 ) ) ;
#41704 = DIRECTION ( 'NONE',  ( -1.000000000000000000, 0.000000000000000000, 0.000000000000000000 ) ) ;
#41705 = ORIENTED_EDGE ( 'NONE', *, *, #36895, .T. ) ;
#41706 = CYLINDRICAL_SURFACE ( 'NONE', #8932, 58.99999999999999289 ) ;
#41707 = CARTESIAN_POINT ( 'NONE',  ( 0.000000000000000000, -47.49120266317494554, -0.8606222198180160099 ) ) ;
#41708 = ORIENTED_EDGE ( 'NONE', *, *, #17703, .T. ) ;
#41709 = CARTESIAN_POINT ( 'NONE',  ( 0.000000000000000000, 0.000000000000000000, 0.000000000000000000 ) ) ;
#41710 = ORIENTED_EDGE ( 'NONE', *, *, #5983, .T. ) ;
#41711 = EDGE_CURVE ( 'NONE', #34938, #10000, #37320, .T. ) ;
#41712 = VERTEX_POINT ( 'NONE', #16657 ) ;
#41713 = DIRECTION ( 'NONE',  ( -1.000000000000000000, 0.000000000000000000, 0.000000000000000000 ) ) ;
#41714 = CARTESIAN_POINT ( 'NONE',  ( 20.39742982868580157, 31.00000000000000355, 76.57971376064386959 ) ) ;
#41715 = EDGE_CURVE ( 'NONE', #16239, #25951, #40575, .T. ) ;
#41716 = ORIENTED_EDGE ( 'NONE', *, *, #5330, .F. ) ;
#41717 = CARTESIAN_POINT ( 'NONE',  ( 17.99999999999999645, -35.78484819117565507, -110.3423972910436390 ) ) ;
#41718 = CIRCLE ( 'NONE', #38229, 36.00000000000000000 ) ;
#41719 = AXIS2_PLACEMENT_3D ( 'NONE', #32850, #9931, #6233 ) ;
#41720 = ADVANCED_FACE ( 'NONE', ( #11594 ), #15100, .F. ) ;
#41721 = DIRECTION ( 'NONE',  ( -1.000000000000000000, -0.000000000000000000, -0.000000000000000000 ) ) ;
#41722 = ORIENTED_EDGE ( 'NONE', *, *, #27984, .F. ) ;
#41723 = CYLINDRICAL_SURFACE ( 'NONE', #34950, 116.0000000000000000 ) ;
#41724 = DIRECTION ( 'NONE',  ( -1.000000000000000000, 0.000000000000000000, 0.000000000000000000 ) ) ;
#41725 = CARTESIAN_POINT ( 'NONE',  ( -7.793954689941437586, 31.00000000000000355, 28.94896179907300748 ) ) ;
#41727 = DIRECTION ( 'NONE',  ( -1.000000000000000000, 0.000000000000000000, 0.000000000000000000 ) ) ;
#41726 = CARTESIAN_POINT ( 'NONE',  ( 0.000000000000000000, 83.49789599728782719, 86.88263557826796557 ) ) ;
#41728 = DIRECTION ( 'NONE',  ( 0.000000000000000000, 0.000000000000000000, 1.000000000000000000 ) ) ;
#41729 = CYLINDRICAL_SURFACE ( 'NONE', #20818, 51.99999999999999289 ) ;
#41730 = ORIENTED_EDGE ( 'NONE', *, *, #14303, .F. ) ;
#41731 = DIRECTION ( 'NONE',  ( 0.000000000000000000, 0.000000000000000000, 1.000000000000000000 ) ) ;
#41732 = ORIENTED_EDGE ( 'NONE', *, *, #20578, .T. ) ;
#41733 = DIRECTION ( 'NONE',  ( 0.000000000000000000, 0.000000000000000000, 1.000000000000000000 ) ) ;
#41734 = CARTESIAN_POINT ( 'NONE',  ( 76.36724925129128394, 31.00000000000000000, 58.57876755120444301 ) ) ;
#41735 = EDGE_CURVE ( 'NONE', #31572, #26713, #24601, .T. ) ;
#41736 = CARTESIAN_POINT ( 'NONE',  ( 17.99999999999999645, 0.000000000000000000, 0.000000000000000000 ) ) ;
#41737 = ORIENTED_EDGE ( 'NONE', *, *, #19902, .T. ) ;
#41738 = CARTESIAN_POINT ( 'NONE',  ( 23.62253089228586944, 40.00000000000000000, -11.62353008834529255 ) ) ;
#41739 = ORIENTED_EDGE ( 'NONE', *, *, #6752, .T. ) ;
#41740 = ORIENTED_EDGE ( 'NONE', *, *, #36791, .T. ) ;
#41741 = CARTESIAN_POINT ( 'NONE',  ( 17.99999999999999645, 108.8684555192046872, 27.12806418649654105 ) ) ;
#41742 = CARTESIAN_POINT ( 'NONE',  ( 17.99999999999999645, 19.47322409167269086, 30.27859877001407085 ) ) ;
#41743 = AXIS2_PLACEMENT_3D ( 'NONE', #31100, #21756, #1186 ) ;
#41744 = CARTESIAN_POINT ( 'NONE',  ( 18.00000000000000355, 0.000000000000000000, 0.000000000000000000 ) ) ;
#41745 = AXIS2_PLACEMENT_3D ( 'NONE', #24142, #40456, #17393 ) ;
#41746 = CARTESIAN_POINT ( 'NONE',  ( -2.797566391619251075E-15, 1.860994515641065082E-14, 7.000000000000002665 ) ) ;
#41747 = AXIS2_PLACEMENT_3D ( 'NONE', #37566, #8114, #7677 ) ;
#41748 = EDGE_CURVE ( 'NONE', #1441, #30171, #32226, .T. ) ;
#41749 = CARTESIAN_POINT ( 'NONE',  ( 17.99999999999999645, 5.919241748379588053, 31.39643714728458690 ) ) ;
#41750 = EDGE_LOOP ( 'NONE', ( #20600, #17629, #32740, #7679 ) ) ;
#41751 = DIRECTION ( 'NONE',  ( -1.000000000000000000, -0.000000000000000000, 0.000000000000000000 ) ) ;
#41752 = EDGE_LOOP ( 'NONE', ( #21565, #16041, #36291, #9579 ) ) ;
#41753 = DIRECTION ( 'NONE',  ( -1.000000000000000000, -0.000000000000000000, -0.000000000000000000 ) ) ;
#41754 = DIRECTION ( 'NONE',  ( 0.000000000000000000, 0.000000000000000000, 1.000000000000000000 ) ) ;
#41755 = APPLICATION_CONTEXT ( 'automotive_design' ) ;
#41756 = FACE_OUTER_BOUND ( 'NONE', #22779, .T. ) ;
#41757 = DIRECTION ( 'NONE',  ( 0.000000000000000000, 0.000000000000000000, 1.000000000000000000 ) ) ;
#41758 = ORIENTED_EDGE ( 'NONE', *, *, #16094, .F. ) ;
#41759 = EDGE_LOOP ( 'NONE', ( #22880, #19361, #15579, #37565 ) ) ;
#41760 = DIRECTION ( 'NONE',  ( -1.000000000000000000, -0.000000000000000000, -0.000000000000000000 ) ) ;
#41761 = CARTESIAN_POINT ( 'NONE',  ( -5.991980000000000750, 1.847259681127465666E-15, -15.08402000000000065 ) ) ;
#41762 = ADVANCED_FACE ( 'NONE', ( #1087 ), #31648, .T. ) ;
#41763 = VECTOR ( 'NONE', #27262, 1000.000000000000000 ) ;
#41764 = EDGE_LOOP ( 'NONE', ( #40337, #12152, #4679, #5905 ) ) ;
#41766 = ORIENTED_EDGE ( 'NONE', *, *, #23226, .T. ) ;
#41765 = CARTESIAN_POINT ( 'NONE',  ( 0.000000000000000000, 0.000000000000000000, 9.999999999999998224 ) ) ;
#41767 = CARTESIAN_POINT ( 'NONE',  ( -38.36856355434107257, 31.00000000000000355, 33.53830235993100217 ) ) ;
#41768 = ADVANCED_FACE ( 'NONE', ( #14443 ), #17730, .F. ) ;
#41769 = VERTEX_POINT ( 'NONE', #37540 ) ;
#41770 = LINE ( 'NONE', #17615, #11216 ) ;
#41771 = CARTESIAN_POINT ( 'NONE',  ( 17.99999999999999645, 51.27532863109366446, 99.79535634195144667 ) ) ;
#41772 = UNCERTAINTY_MEASURE_WITH_UNIT (LENGTH_MEASURE( 1.000000000000000082E-05 ), #4708, 'distance_accuracy_value', 'NONE');
#41773 = VERTEX_POINT ( 'NONE', #18608 ) ;
#41774 = CARTESIAN_POINT ( 'NONE',  ( 60.45897909546184934, 39.99999999999999289, -46.24578392211154210 ) ) ;
#41775 = AXIS2_PLACEMENT_3D ( 'NONE', #43101, #13254, #39817 ) ;
#41776 = VECTOR ( 'NONE', #42400, 1000.000000000000000 ) ;
#41777 = CYLINDRICAL_SURFACE ( 'NONE', #13052, 59.00000000000000000 ) ;
#41778 = CARTESIAN_POINT ( 'NONE',  ( 0.000000000000000000, 13.85708833600031298, -45.43276465116649376 ) ) ;
#41779 = ORIENTED_EDGE ( 'NONE', *, *, #34346, .T. ) ;
#41780 = CARTESIAN_POINT ( 'NONE',  ( 0.000000000000000000, 103.4151313792879421, -61.85306461934304423 ) ) ;
#41781 = VERTEX_POINT ( 'NONE', #8306 ) ;
#41782 = CARTESIAN_POINT ( 'NONE',  ( 0.000000000000000000, -99.97660604680010010, 67.26937820704856108 ) ) ;
#41783 = CARTESIAN_POINT ( 'NONE',  ( 17.99999999999999645, -116.0452958106482981, 32.46506308663420270 ) ) ;
#41784 = EDGE_CURVE ( 'NONE', #2747, #8333, #34475, .T. ) ;
#41785 = CARTESIAN_POINT ( 'NONE',  ( 21.58803501788969115, 31.00000000000000355, 63.55567069162312777 ) ) ;
#41786 = EDGE_CURVE ( 'NONE', #30139, #23467, #1567, .T. ) ;
#41787 = DIRECTION ( 'NONE',  ( 0.000000000000000000, 0.000000000000000000, 1.000000000000000000 ) ) ;
#41788 = ORIENTED_EDGE ( 'NONE', *, *, #7271, .T. ) ;
#41789 = EDGE_CURVE ( 'NONE', #18411, #37133, #25145, .T. ) ;
#41790 = EDGE_CURVE ( 'NONE', #12306, #2405, #5061, .T. ) ;
#41791 = CARTESIAN_POINT ( 'NONE',  ( 0.000000000000000000, -35.20873326984102647, 31.88259874184018372 ) ) ;
#41792 = VERTEX_POINT ( 'NONE', #31232 ) ;
#41793 = CARTESIAN_POINT ( 'NONE',  ( 8.999999999999998224, -79.18387647320821543, 84.76976882518735579 ) ) ;
#41794 = DIRECTION ( 'NONE',  ( 0.000000000000000000, 0.000000000000000000, 1.000000000000000000 ) ) ;
#41795 = CARTESIAN_POINT ( 'NONE',  ( -79.00001692110807028, 31.00000000000000711, 21.04436337235335230 ) ) ;
#41796 = CARTESIAN_POINT ( 'NONE',  ( 74.83201185296370284, 39.99999999999999289, -43.08100868844128684 ) ) ;
#41797 = CARTESIAN_POINT ( 'NONE',  ( -153.1500000000000057, -5.251434100941175950E-13, 6.999999999999998224 ) ) ;
#41798 = ORIENTED_EDGE ( 'NONE', *, *, #28981, .T. ) ;
#41799 = DIRECTION ( 'NONE',  ( -1.000000000000000000, -0.000000000000000000, 0.000000000000000000 ) ) ;
#41800 = VERTEX_POINT ( 'NONE', #4818 ) ;
#41801 = VECTOR ( 'NONE', #3071, 1000.000000000000000 ) ;
#41802 = CARTESIAN_POINT ( 'NONE',  ( 0.000000000000000000, 0.000000000000000000, 0.000000000000000000 ) ) ;
#41803 = AXIS2_PLACEMENT_3D ( 'NONE', #21791, #5146, #18510 ) ;
#41804 = CARTESIAN_POINT ( 'NONE',  ( 0.000000000000000000, 23.87611429743691360, -20.54551452399595135 ) ) ;
#41805 = AXIS2_PLACEMENT_3D ( 'NONE', #10487, #6544, #42982 ) ;
#41807 = VERTEX_POINT ( 'NONE', #34917 ) ;
#41806 = DIRECTION ( 'NONE',  ( 0.000000000000000000, -0.5264321628773627193, 0.8502171357296098853 ) ) ;
#41808 = CARTESIAN_POINT ( 'NONE',  ( 0.000000000000000000, 39.55064067543099071, -25.36340625197318488 ) ) ;
#41809 = ORIENTED_EDGE ( 'NONE', *, *, #17043, .T. ) ;
#41810 = DIRECTION ( 'NONE',  ( 0.000000000000000000, 0.9822872507286879440, 0.1873813145857285145 ) ) ;
#41811 = DIRECTION ( 'NONE',  ( 0.000000000000000000, 0.000000000000000000, 1.000000000000000000 ) ) ;
#41812 = DIRECTION ( 'NONE',  ( -1.847415842360817977E-16, 1.000000000000000000, 0.000000000000000000 ) ) ;
#41813 = ORIENTED_EDGE ( 'NONE', *, *, #16747, .F. ) ;
#41814 = CARTESIAN_POINT ( 'NONE',  ( 0.000000000000000000, 0.000000000000000000, 0.000000000000000000 ) ) ;
#41815 = EDGE_CURVE ( 'NONE', #28933, #2262, #19698, .T. ) ;
#41816 = FACE_OUTER_BOUND ( 'NONE', #10890, .T. ) ;
#41818 = DIRECTION ( 'NONE',  ( 0.000000000000000000, 0.000000000000000000, 1.000000000000000000 ) ) ;
#41817 = CARTESIAN_POINT ( 'NONE',  ( 0.000000000000000000, 0.000000000000000000, 0.000000000000000000 ) ) ;
#41819 = EDGE_LOOP ( 'NONE', ( #17671, #18976 ) ) ;
#41820 = CARTESIAN_POINT ( 'NONE',  ( 17.99999999999999645, -23.10276247328181398, 118.2656051737069021 ) ) ;
#41821 = EDGE_LOOP ( 'NONE', ( #8376, #31632, #5903, #23816 ) ) ;
#41822 = CYLINDRICAL_SURFACE ( 'NONE', #32864, 130.0000000000000000 ) ;
#41823 = CARTESIAN_POINT ( 'NONE',  ( 15.66220904948252546, 40.00000000000000000, -31.63873590539992975 ) ) ;
#41824 = FACE_OUTER_BOUND ( 'NONE', #6867, .T. ) ;
#41825 = AXIS2_PLACEMENT_3D ( 'NONE', #11824, #21665, #39235 ) ;
#41826 = FACE_OUTER_BOUND ( 'NONE', #5559, .T. ) ;
#41827 = CARTESIAN_POINT ( 'NONE',  ( 18.00000000000000355, -6.109652351742118626, 46.58570277113506819 ) ) ;
#41828 = VERTEX_POINT ( 'NONE', #5029 ) ;
#41829 = CARTESIAN_POINT ( 'NONE',  ( 17.99999999999999645, -13.22719389141998825, 28.58720592780592185 ) ) ;
#41830 = EDGE_LOOP ( 'NONE', ( #20543, #38648, #17771, #5585 ) ) ;
#41831 = CIRCLE ( 'NONE', #6321, 47.49900000000000233 ) ;
#41832 = CARTESIAN_POINT ( 'NONE',  ( 18.00000000000000355, -32.00046193115174731, 34.40241257139675923 ) ) ;
#41833 = DIRECTION ( 'NONE',  ( 1.000000000000000000, 0.000000000000000000, 0.000000000000000000 ) ) ;
#41834 = AXIS2_PLACEMENT_3D ( 'NONE', #11257, #25240, #28507 ) ;
#41835 = CARTESIAN_POINT ( 'NONE',  ( -25.53337963587170023, 31.00000000000000355, 29.12008199578403023 ) ) ;
#41836 = ORIENTED_EDGE ( 'NONE', *, *, #42019, .T. ) ;
#41837 = DIRECTION ( 'NONE',  ( 0.000000000000000000, 0.000000000000000000, 1.000000000000000000 ) ) ;
#41838 = EDGE_CURVE ( 'NONE', #22001, #22222, #21455, .T. ) ;
#41839 = EDGE_CURVE ( 'NONE', #10857, #29797, #835, .T. ) ;
#41840 = CIRCLE ( 'NONE', #1408, 116.0000000000000000 ) ;
#41841 = EDGE_CURVE ( 'NONE', #37209, #3729, #28177, .T. ) ;
#41842 = DIRECTION ( 'NONE',  ( 1.000000000000000000, 0.000000000000000000, 0.000000000000000000 ) ) ;
#41843 = CARTESIAN_POINT ( 'NONE',  ( 5.399612364985509672, 31.00000000000000355, -82.60416666586320389 ) ) ;
#41844 = EDGE_LOOP ( 'NONE', ( #40848, #8247, #7890, #38637 ) ) ;
#41845 = CARTESIAN_POINT ( 'NONE',  ( -49.95450512538511134, 31.00000000000000355, 13.28959769214884545 ) ) ;
#41846 = AXIS2_PLACEMENT_3D ( 'NONE', #40158, #23641, #26454 ) ;
#41847 = CARTESIAN_POINT ( 'NONE',  ( 22.58587702529213104, 40.00000000000000000, 84.29678642628191199 ) ) ;
#41848 = ORIENTED_EDGE ( 'NONE', *, *, #20882, .F. ) ;
#41849 = DIRECTION ( 'NONE',  ( 3.009274222672345096E-17, 1.000000000000000000, -2.455023325076454960E-18 ) ) ;
#41850 = EDGE_CURVE ( 'NONE', #36637, #30242, #19030, .T. ) ;
#41851 = CIRCLE ( 'NONE', #6313, 59.00000000000000711 ) ;
#41852 = CARTESIAN_POINT ( 'NONE',  ( 17.99999999999999645, -30.71634675606060227, 8.790889055186445589 ) ) ;
#41853 = DIRECTION ( 'NONE',  ( 0.000000000000000000, 0.000000000000000000, -1.000000000000000000 ) ) ;
#41855 = ORIENTED_EDGE ( 'NONE', *, *, #15432, .F. ) ;
#41854 = CARTESIAN_POINT ( 'NONE',  ( -5.991980000000000750, 0.000000000000000000, 0.000000000000000000 ) ) ;
#41856 = DIRECTION ( 'NONE',  ( -1.000000000000000000, 0.000000000000000000, 0.000000000000000000 ) ) ;
#41857 = VECTOR ( 'NONE', #12989, 1000.000000000000000 ) ;
#41858 = CYLINDRICAL_SURFACE ( 'NONE', #33460, 139.4999999999992610 ) ;
#41859 = VERTEX_POINT ( 'NONE', #7865 ) ;
#41860 = CARTESIAN_POINT ( 'NONE',  ( -30.22953878324074495, 40.00000000000000000, 61.32923288305941867 ) ) ;
#41861 = DIRECTION ( 'NONE',  ( 3.996523416598930318E-16, -2.658563593772947863E-15, -1.000000000000000000 ) ) ;
#41862 = AXIS2_PLACEMENT_3D ( 'NONE', #42180, #9249, #36074 ) ;
#41863 = AXIS2_PLACEMENT_3D ( 'NONE', #34749, #34956, #17776 ) ;
#41864 = VERTEX_POINT ( 'NONE', #21223 ) ;
#41865 = FACE_OUTER_BOUND ( 'NONE', #14107, .T. ) ;
#41866 = CARTESIAN_POINT ( 'NONE',  ( 17.99999999999999645, 110.3490479609632615, -20.28201389785435182 ) ) ;
#41867 = CIRCLE ( 'NONE', #28663, 116.0000000000000000 ) ;
#41868 = DIRECTION ( 'NONE',  ( 1.000000000000000000, 0.000000000000000000, 0.000000000000000000 ) ) ;
#41869 = ORIENTED_EDGE ( 'NONE', *, *, #8076, .F. ) ;
#41870 = EDGE_CURVE ( 'NONE', #14903, #27389, #9235, .T. ) ;
#41871 = ORIENTED_EDGE ( 'NONE', *, *, #11556, .F. ) ;
#41872 = DIRECTION ( 'NONE',  ( 0.000000000000000000, -0.9957341762950354669, 0.09226835946329131621 ) ) ;
#41873 = ORIENTED_EDGE ( 'NONE', *, *, #41815, .T. ) ;
#41874 = DIRECTION ( 'NONE',  ( 0.000000000000000000, 0.3140767120219427611, 0.9493976084683832806 ) ) ;
#41875 = CARTESIAN_POINT ( 'NONE',  ( 9.000000000000001776, -106.6051926090968180, -45.73109345704926909 ) ) ;
#41876 = CARTESIAN_POINT ( 'NONE',  ( 0.000000000000000000, 0.000000000000000000, 0.000000000000000000 ) ) ;
#41877 = FACE_OUTER_BOUND ( 'NONE', #21738, .T. ) ;
#41878 = EDGE_LOOP ( 'NONE', ( #2396, #22664 ) ) ;
#41879 = LINE ( 'NONE', #42302, #10551 ) ;
#41880 = DIRECTION ( 'NONE',  ( 0.000000000000000000, 0.000000000000000000, 1.000000000000000000 ) ) ;
#41881 = ORIENTED_EDGE ( 'NONE', *, *, #8368, .F. ) ;
#41882 = DIRECTION ( 'NONE',  ( 0.000000000000000000, 0.000000000000000000, 1.000000000000000000 ) ) ;
#41883 = ADVANCED_FACE ( 'NONE', ( #17959 ), #1319, .F. ) ;
#41884 = CARTESIAN_POINT ( 'NONE',  ( 18.00000000000000355, 0.000000000000000000, 0.000000000000000000 ) ) ;
#41885 = CARTESIAN_POINT ( 'NONE',  ( 106.4195705685741302, 17.99999999999998934, -106.4195705685767166 ) ) ;
#41886 = CARTESIAN_POINT ( 'NONE',  ( -104.8158553526607477, 17.11489954122027157, 3.963965400206364453 ) ) ;
#41887 = CARTESIAN_POINT ( 'NONE',  ( -13.51098712749246467, 31.00000000000000355, -50.41620372279128048 ) ) ;
#41888 = CIRCLE ( 'NONE', #20320, 59.00000000000000711 ) ;
#41889 = EDGE_LOOP ( 'NONE', ( #12999, #4083, #19524, #25600 ) ) ;
#41890 = FACE_OUTER_BOUND ( 'NONE', #10345, .T. ) ;
#41891 = AXIS2_PLACEMENT_3D ( 'NONE', #9194, #12069, #15768 ) ;
#41892 = ORIENTED_EDGE ( 'NONE', *, *, #32769, .F. ) ;
#41893 = EDGE_CURVE ( 'NONE', #42630, #4481, #33613, .T. ) ;
#41894 = CIRCLE ( 'NONE', #37690, 20.00000000000000711 ) ;
#41895 = SHAPE_REPRESENTATION ( 'Return Coil Spring', ( #13552 ), #18474 ) ;
#41896 = CARTESIAN_POINT ( 'NONE',  ( -38.74991464700507748, 40.00000000000000000, 44.18781823130588293 ) ) ;
#41897 = EDGE_CURVE ( 'NONE', #20272, #5216, #37100, .T. ) ;
#41898 = AXIS2_PLACEMENT_3D ( 'NONE', #23461, #3543, #17132 ) ;
#41899 = CARTESIAN_POINT ( 'NONE',  ( 17.99999999999999645, -19.47322409167248480, -30.27859877001420230 ) ) ;
#41900 = EDGE_CURVE ( 'NONE', #40959, #13405, #42948, .T. ) ;
#41901 = CYLINDRICAL_SURFACE ( 'NONE', #36070, 51.99999999999999289 ) ;
#41902 = CYLINDRICAL_SURFACE ( 'NONE', #23986, 2.649999999999985700 ) ;
#41903 = CARTESIAN_POINT ( 'NONE',  ( 9.000000000000001776, -19.74581912682808849, -48.10512059033413834 ) ) ;
#41904 = VERTEX_POINT ( 'NONE', #22719 ) ;
#41905 = CARTESIAN_POINT ( 'NONE',  ( -23.50435451693408950, 40.00000000000000000, 30.64856077952424940 ) ) ;
#41906 = ORIENTED_EDGE ( 'NONE', *, *, #15135, .F. ) ;
#41907 = DIRECTION ( 'NONE',  ( 0.000000000000000000, 0.000000000000000000, 1.000000000000000000 ) ) ;
#41908 = DIRECTION ( 'NONE',  ( 0.000000000000000000, 0.05322217484217878214, -0.9985826956767620555 ) ) ;
#41909 = EDGE_LOOP ( 'NONE', ( #38365, #33565 ) ) ;
#41910 = DIRECTION ( 'NONE',  ( 0.000000000000000000, 0.9714298932647107421, -0.2373266998711119347 ) ) ;
#41911 = EDGE_LOOP ( 'NONE', ( #21995, #18692, #31682, #33462 ) ) ;
#41912 = DIRECTION ( 'NONE',  ( 0.000000000000000000, 0.000000000000000000, -1.000000000000000000 ) ) ;
#41913 = VERTEX_POINT ( 'NONE', #32082 ) ;
#41915 = ADVANCED_FACE ( 'NONE', ( #32502 ), #22299, .F. ) ;
#41914 = CIRCLE ( 'NONE', #22444, 2.649999999999957723 ) ;
#41916 = ORIENTED_EDGE ( 'NONE', *, *, #42431, .F. ) ;
#41917 = CARTESIAN_POINT ( 'NONE',  ( 4.858130855304160865E-15, 5.778671572660278980E-15, 2.000000000000001776 ) ) ;
#41918 = CIRCLE ( 'NONE', #37745, 58.99999999999999289 ) ;
#41919 = CARTESIAN_POINT ( 'NONE',  ( 37.87019299815447937, 31.00000000000000355, -76.55254356380190472 ) ) ;
#41920 = ORIENTED_EDGE ( 'NONE', *, *, #7382, .F. ) ;
#41921 = CARTESIAN_POINT ( 'NONE',  ( 0.000000000000000000, -37.91532898920940653, 28.61088654061626357 ) ) ;
#41922 = CIRCLE ( 'NONE', #39821, 58.99999999999999289 ) ;
#41923 = CARTESIAN_POINT ( 'NONE',  ( 17.99999999999999645, -28.57802095670097131, 14.28532136906662586 ) ) ;
#41924 = ORIENTED_EDGE ( 'NONE', *, *, #1053, .T. ) ;
#41925 = DIRECTION ( 'NONE',  ( 0.000000000000000000, 0.000000000000000000, 1.000000000000000000 ) ) ;
#41926 = CARTESIAN_POINT ( 'NONE',  ( -6.200000000000001066, 19.19999999999999929, 0.000000000000000000 ) ) ;
#41927 = CIRCLE ( 'NONE', #23165, 36.00000000000000000 ) ;
#41928 = CARTESIAN_POINT ( 'NONE',  ( 26.89767027507546615, 31.00000000000000355, -1.736414864505229527 ) ) ;
#41930 = DIRECTION ( 'NONE',  ( 0.000000000000000000, 0.000000000000000000, 1.000000000000000000 ) ) ;
#41929 = DIRECTION ( 'NONE',  ( -0.8191520442889902442, 0.000000000000000000, -0.5735764363510482688 ) ) ;
#41931 = CYLINDRICAL_SURFACE ( 'NONE', #20642, 13.60000000000000142 ) ;
#41932 = CARTESIAN_POINT ( 'NONE',  ( 0.000000000000000000, -30.71634675606047793, -8.790889055186887902 ) ) ;
#41933 = ADVANCED_FACE ( 'NONE', ( #5874 ), #42517, .T. ) ;
#41934 = EDGE_LOOP ( 'NONE', ( #30282, #33659, #28248, #10988 ) ) ;
#41935 =( NAMED_UNIT ( * ) PLANE_ANGLE_UNIT ( ) SI_UNIT ( $, .RADIAN. ) );
#41936 = DIRECTION ( 'NONE',  ( -1.000000000000000000, -0.000000000000000000, -0.000000000000000000 ) ) ;
#41937 = ORIENTED_EDGE ( 'NONE', *, *, #1246, .F. ) ;
#41938 = CARTESIAN_POINT ( 'NONE',  ( 17.99999999999999645, 56.51398178981952469, -96.92493144647394843 ) ) ;
#41939 = CARTESIAN_POINT ( 'NONE',  ( 81.71702119589899382, 31.00000000000000000, -47.19735719316410183 ) ) ;
#41940 = DIRECTION ( 'NONE',  ( 1.000000000000000000, 0.000000000000000000, 0.000000000000000000 ) ) ;
#41941 = ORIENTED_EDGE ( 'NONE', *, *, #22784, .T. ) ;
#41942 = CARTESIAN_POINT ( 'NONE',  ( 22.42277067908921850, 40.00000000000000000, 12.94072372014797701 ) ) ;
#41943 = CARTESIAN_POINT ( 'NONE',  ( 9.106956811744730373, 40.00000000000000000, -33.78410985268681799 ) ) ;
#41944 = EDGE_CURVE ( 'NONE', #35377, #9926, #19232, .T. ) ;
#41945 = AXIS2_PLACEMENT_3D ( 'NONE', #2999, #29672, #25772 ) ;
#41946 = AXIS2_PLACEMENT_3D ( 'NONE', #20348, #40146, #4144 ) ;
#41947 = VERTEX_POINT ( 'NONE', #12240 ) ;
#41948 = CIRCLE ( 'NONE', #21116, 116.0000000000000000 ) ;
#41949 = ORIENTED_EDGE ( 'NONE', *, *, #26526, .T. ) ;
#41950 = FACE_OUTER_BOUND ( 'NONE', #33992, .T. ) ;
#41951 = CYLINDRICAL_SURFACE ( 'NONE', #38110, 18.77999999999999048 ) ;
#41952 = CARTESIAN_POINT ( 'NONE',  ( 17.99999999999999645, 0.000000000000000000, 0.000000000000000000 ) ) ;
#41953 = VECTOR ( 'NONE', #18586, 1000.000000000000000 ) ;
#41954 = EDGE_CURVE ( 'NONE', #6044, #21659, #9911, .T. ) ;
#41955 = CARTESIAN_POINT ( 'NONE',  ( 17.99999999999999645, 5.456439917446431309, -112.0647122740741253 ) ) ;
#41956 = FACE_OUTER_BOUND ( 'NONE', #39328, .T. ) ;
#41957 = ORIENTED_EDGE ( 'NONE', *, *, #22262, .F. ) ;
#41958 = FACE_OUTER_BOUND ( 'NONE', #27514, .T. ) ;
#41959 = ORIENTED_EDGE ( 'NONE', *, *, #22850, .F. ) ;
#41960 = DIRECTION ( 'NONE',  ( 0.000000000000000000, 0.000000000000000000, -1.000000000000000000 ) ) ;
#41961 = FACE_OUTER_BOUND ( 'NONE', #35214, .T. ) ;
#41962 = DIRECTION ( 'NONE',  ( 1.000000000000000000, 0.000000000000000000, -0.000000000000000000 ) ) ;
#41963 = DIRECTION ( 'NONE',  ( 0.000000000000000000, 0.000000000000000000, 1.000000000000000000 ) ) ;
#41964 = VERTEX_POINT ( 'NONE', #29038 ) ;
#41965 = ORIENTED_EDGE ( 'NONE', *, *, #19582, .T. ) ;
#41966 = CARTESIAN_POINT ( 'NONE',  ( -105.9879088449591933, 17.11489954122026447, -2.880719929157669945 ) ) ;
#41967 = EDGE_CURVE ( 'NONE', #29185, #26760, #15531, .T. ) ;
#41968 = VERTEX_POINT ( 'NONE', #2166 ) ;
#41970 = ORIENTED_EDGE ( 'NONE', *, *, #43009, .T. ) ;
#41969 = DIRECTION ( 'NONE',  ( 1.000000000000000000, 0.000000000000000000, 0.000000000000000000 ) ) ;
#41971 = CARTESIAN_POINT ( 'NONE',  ( -51.89982240187124063, 31.00000000000000355, 3.308651922604603168 ) ) ;
#41973 = EDGE_CURVE ( 'NONE', #32693, #566, #6100, .T. ) ;
#41972 = ORIENTED_EDGE ( 'NONE', *, *, #18946, .T. ) ;
#41974 = DIRECTION ( 'NONE',  ( 0.000000000000000000, 0.000000000000000000, 1.000000000000000000 ) ) ;
#41975 = CYLINDRICAL_SURFACE ( 'NONE', #42561, 116.0000000000000000 ) ;
#41976 = ORIENTED_EDGE ( 'NONE', *, *, #17408, .T. ) ;
#41977 = CARTESIAN_POINT ( 'NONE',  ( -43.11175393642376719, 40.00000000000000000, 56.02072642018850246 ) ) ;
#41978 = CARTESIAN_POINT ( 'NONE',  ( 0.000000000000000000, 44.25018368420743542, 27.31155879685196552 ) ) ;
#41979 = AXIS2_PLACEMENT_3D ( 'NONE', #12441, #39653, #42288 ) ;
#41980 = CARTESIAN_POINT ( 'NONE',  ( 0.000000000000000000, 0.000000000000000000, 6.999999999999998224 ) ) ;
#41981 = VERTEX_POINT ( 'NONE', #26184 ) ;
#41982 = DIRECTION ( 'NONE',  ( 1.000000000000000000, 0.000000000000000000, 0.000000000000000000 ) ) ;
#41983 = EDGE_CURVE ( 'NONE', #42855, #38496, #26656, .T. ) ;
#41984 = ORIENTED_EDGE ( 'NONE', *, *, #29915, .T. ) ;
#41985 = AXIS2_PLACEMENT_3D ( 'NONE', #13966, #27260, #40096 ) ;
#41986 = CARTESIAN_POINT ( 'NONE',  ( -6.004904395537136175, 0.000000000000000000, 0.000000000000000000 ) ) ;
#41987 = DIRECTION ( 'NONE',  ( 1.000000000000000000, 0.000000000000000000, 0.000000000000000000 ) ) ;
#41988 = CARTESIAN_POINT ( 'NONE',  ( 40.54457361686378647, 31.00000000000000355, 52.83773991529862712 ) ) ;
#41989 = FACE_OUTER_BOUND ( 'NONE', #13266, .T. ) ;
#41990 = VERTEX_POINT ( 'NONE', #9363 ) ;
#41991 = CARTESIAN_POINT ( 'NONE',  ( -10.00000000000000000, 0.000000000000000000, 0.000000000000000000 ) ) ;
#41992 = EDGE_CURVE ( 'NONE', #28304, #15576, #12772, .T. ) ;
#41993 = ORIENTED_EDGE ( 'NONE', *, *, #9169, .F. ) ;
#41994 = DIRECTION ( 'NONE',  ( 1.000000000000000000, 0.000000000000000000, 0.000000000000000000 ) ) ;
#41995 = ADVANCED_FACE ( 'NONE', ( #35746 ), #35549, .F. ) ;
#41996 = DIRECTION ( 'NONE',  ( 0.000000000000000000, 0.000000000000000000, -1.000000000000000000 ) ) ;
#41997 = CARTESIAN_POINT ( 'NONE',  ( -73.09555549758189841, 31.00000000000000711, 35.91380138263622257 ) ) ;
#41998 = CARTESIAN_POINT ( 'NONE',  ( -79.17211738000736432, 40.00000000000000711, 45.58486055166100215 ) ) ;
#41999 = DIRECTION ( 'NONE',  ( -1.000000000000000000, -0.000000000000000000, 0.000000000000000000 ) ) ;
#42000 = EDGE_CURVE ( 'NONE', #33321, #36878, #3001, .T. ) ;
#42001 = CIRCLE ( 'NONE', #35039, 116.0000000000000000 ) ;
#42002 = VERTEX_POINT ( 'NONE', #32924 ) ;
#42003 = DIRECTION ( 'NONE',  ( 0.000000000000000000, 0.000000000000000000, 1.000000000000000000 ) ) ;
#42004 = ORIENTED_EDGE ( 'NONE', *, *, #564, .F. ) ;
#42005 = DIRECTION ( 'NONE',  ( -1.000000000000000000, -0.000000000000000000, 0.000000000000000000 ) ) ;
#42007 = VERTEX_POINT ( 'NONE', #42087 ) ;
#42006 = DIRECTION ( 'NONE',  ( -1.000000000000000000, 0.000000000000000000, 0.000000000000000000 ) ) ;
#42008 = CARTESIAN_POINT ( 'NONE',  ( 17.99999999999999645, -41.60679253225688967, -108.2814610871950265 ) ) ;
#42009 = ORIENTED_EDGE ( 'NONE', *, *, #39888, .T. ) ;
#42010 = DIRECTION ( 'NONE',  ( -1.000000000000000000, -0.000000000000000000, 0.000000000000000000 ) ) ;
#42011 = CARTESIAN_POINT ( 'NONE',  ( 0.000000000000000000, 29.68570942776486987, -10.53307442156903662 ) ) ;
#42012 = FACE_OUTER_BOUND ( 'NONE', #15952, .T. ) ;
#42013 = AXIS2_PLACEMENT_3D ( 'NONE', #16768, #36350, #40269 ) ;
#42014 = ORIENTED_EDGE ( 'NONE', *, *, #33914, .T. ) ;
#42015 = EDGE_CURVE ( 'NONE', #23269, #37692, #16368, .T. ) ;
#42016 = CARTESIAN_POINT ( 'NONE',  ( 0.000000000000000000, 84.77518783075197462, -73.49448960231268302 ) ) ;
#42017 = EDGE_CURVE ( 'NONE', #5275, #40032, #40601, .T. ) ;
#42018 = DIRECTION ( 'NONE',  ( -3.009274222672345712E-17, -1.000000000000000000, 2.455023325076455345E-18 ) ) ;
#42019 = EDGE_CURVE ( 'NONE', #17691, #40502, #4358, .T. ) ;
#42020 = ADVANCED_FACE ( 'NONE', ( #30315 ), #7164, .F. ) ;
#42022 = LINE ( 'NONE', #18115, #28305 ) ;
#42021 = DIRECTION ( 'NONE',  ( 0.000000000000000000, -0.4610925014493144625, -0.8873520750565775383 ) ) ;
#42023 = ORIENTED_EDGE ( 'NONE', *, *, #35482, .T. ) ;
#42024 = DIRECTION ( 'NONE',  ( -1.000000000000000000, 0.000000000000000000, 0.000000000000000000 ) ) ;
#42025 = CARTESIAN_POINT ( 'NONE',  ( -4.000000000000000000, 2.309401076758498483, -0.4999999999999927280 ) ) ;
#42026 = CARTESIAN_POINT ( 'NONE',  ( -40.32452739091078797, 40.00000000000000000, -13.76986825753265720 ) ) ;
#42027 = DIRECTION ( 'NONE',  ( -1.000000000000000000, -0.000000000000000000, 0.000000000000000000 ) ) ;
#42028 = CARTESIAN_POINT ( 'NONE',  ( 17.99999999999999645, 53.40478689619730090, 108.0204598100367548 ) ) ;
#42029 = VECTOR ( 'NONE', #37968, 1000.000000000000000 ) ;
#42030 = DIRECTION ( 'NONE',  ( -1.000000000000000000, -0.000000000000000000, -0.000000000000000000 ) ) ;
#42031 = ORIENTED_EDGE ( 'NONE', *, *, #26374, .T. ) ;
#42032 = DIRECTION ( 'NONE',  ( 0.000000000000000000, 0.000000000000000000, 1.000000000000000000 ) ) ;
#42033 = ORIENTED_EDGE ( 'NONE', *, *, #2021, .T. ) ;
#42034 = DIRECTION ( 'NONE',  ( -1.000000000000000000, -0.000000000000000000, 0.000000000000000000 ) ) ;
#42035 = LINE ( 'NONE', #12190, #9423 ) ;
#42036 = CARTESIAN_POINT ( 'NONE',  ( -12.24460912605626106, 31.00000000000000355, 36.08157028455360660 ) ) ;
#42037 = VERTEX_POINT ( 'NONE', #43166 ) ;
#42038 = CARTESIAN_POINT ( 'NONE',  ( 12.49999999999995026, -1.235163061630884815E-13, -40.00000000000000711 ) ) ;
#42039 = VERTEX_POINT ( 'NONE', #16823 ) ;
#42040 = STYLED_ITEM ( 'NONE', ( #34972 ), #10920 ) ;
#42041 = DIRECTION ( 'NONE',  ( -1.000000000000000000, -0.000000000000000000, 0.000000000000000000 ) ) ;
#42042 = ADVANCED_FACE ( 'NONE', ( #30542 ), #37057, .F. ) ;
#42043 = CARTESIAN_POINT ( 'NONE',  ( 6.054110834496887250, 31.00000000000000355, -92.60416666599778068 ) ) ;
#42044 = EDGE_CURVE ( 'NONE', #27751, #42728, #35051, .T. ) ;
#42045 = ORIENTED_EDGE ( 'NONE', *, *, #19883, .F. ) ;
#42046 = CARTESIAN_POINT ( 'NONE',  ( -35.18788409414197815, 31.00000000000000355, -40.25400722681192178 ) ) ;
#42047 = CARTESIAN_POINT ( 'NONE',  ( 57.05379307147669721, 39.99999999999999289, -74.37948018729004218 ) ) ;
#42048 = ORIENTED_EDGE ( 'NONE', *, *, #5201, .F. ) ;
#42049 =( REPRESENTATION_RELATIONSHIP ('NONE','NONE', #330, #37437 ) REPRESENTATION_RELATIONSHIP_WITH_TRANSFORMATION ( #11329 )SHAPE_REPRESENTATION_RELATIONSHIP( ) );
#42050 = CYLINDRICAL_SURFACE ( 'NONE', #6004, 2.649999999999985700 ) ;
#42051 = CARTESIAN_POINT ( 'NONE',  ( -10.00000000000000000, 0.000000000000000000, 0.000000000000000000 ) ) ;
#42052 = LINE ( 'NONE', #5635, #38663 ) ;
#42053 = AXIS2_PLACEMENT_3D ( 'NONE', #8090, #18830, #1748 ) ;
#42055 = VERTEX_POINT ( 'NONE', #3873 ) ;
#42054 = DIRECTION ( 'NONE',  ( 0.000000000000000000, 0.000000000000000000, 1.000000000000000000 ) ) ;
#42056 = CARTESIAN_POINT ( 'NONE',  ( 17.99999999999999645, 115.6826031496113529, -8.575274253896266075 ) ) ;
#42057 = CARTESIAN_POINT ( 'NONE',  ( 17.99999999999999645, 0.000000000000000000, 0.000000000000000000 ) ) ;
#42058 = AXIS2_PLACEMENT_3D ( 'NONE', #30717, #9978, #39643 ) ;
#42059 = ORIENTED_EDGE ( 'NONE', *, *, #25429, .F. ) ;
#42060 = CARTESIAN_POINT ( 'NONE',  ( -62.77658523491555798, 40.00000000000000711, 48.16944601536268777 ) ) ;
#42061 = DIRECTION ( 'NONE',  ( 1.000000000000000000, 0.000000000000000000, 0.000000000000000000 ) ) ;
#42062 = ORIENTED_EDGE ( 'NONE', *, *, #37415, .T. ) ;
#42063 = EDGE_CURVE ( 'NONE', #6563, #20905, #8575, .T. ) ;
#42064 = CARTESIAN_POINT ( 'NONE',  ( 0.000000000000000000, 0.000000000000000000, 0.000000000000000000 ) ) ;
#42065 = ADVANCED_FACE ( 'NONE', ( #40530, #26613 ), #610, .F. ) ;
#42066 = EDGE_CURVE ( 'NONE', #17546, #18529, #27055, .T. ) ;
#42067 = ORIENTED_EDGE ( 'NONE', *, *, #33387, .T. ) ;
#42068 = PRODUCT_DEFINITION_FORMATION_WITH_SPECIFIED_SOURCE ( 'ANY', '', #29412, .NOT_KNOWN. ) ;
#42069 = EDGE_CURVE ( 'NONE', #41404, #6009, #7169, .T. ) ;
#42070 = EDGE_LOOP ( 'NONE', ( #22155, #31040, #31095, #39364 ) ) ;
#42071 = CARTESIAN_POINT ( 'NONE',  ( 18.00000000000000355, -2.123073309834832667, -47.45152853935337589 ) ) ;
#42072 = AXIS2_PLACEMENT_3D ( 'NONE', #33554, #17451, #21158 ) ;
#42073 = VERTEX_POINT ( 'NONE', #30107 ) ;
#42074 = DIRECTION ( 'NONE',  ( -1.000000000000000000, -0.000000000000000000, 0.000000000000000000 ) ) ;
#42075 = CARTESIAN_POINT ( 'NONE',  ( 17.99999999999999645, -112.1702510623870239, -2.471285140323770335 ) ) ;
#42076 = CARTESIAN_POINT ( 'NONE',  ( -10.00000000000000000, 0.000000000000000000, 0.000000000000000000 ) ) ;
#42077 = DIRECTION ( 'NONE',  ( -1.000000000000000000, -0.000000000000000000, -0.000000000000000000 ) ) ;
#42079 = ORIENTED_EDGE ( 'NONE', *, *, #14431, .T. ) ;
#42078 = CIRCLE ( 'NONE', #15650, 47.49900000000000233 ) ;
#42080 = DIRECTION ( 'NONE',  ( 0.000000000000000000, 0.000000000000000000, -1.000000000000000000 ) ) ;
#42081 = AXIS2_PLACEMENT_3D ( 'NONE', #12023, #5233, #18815 ) ;
#42082 = ORIENTED_EDGE ( 'NONE', *, *, #21333, .T. ) ;
#42083 = AXIS2_PLACEMENT_3D ( 'NONE', #41746, #41083, #11888 ) ;
#42084 = CYLINDRICAL_SURFACE ( 'NONE', #10598, 116.0000000000000000 ) ;
#42085 = EDGE_CURVE ( 'NONE', #20139, #25483, #38499, .T. ) ;
#42086 = VERTEX_POINT ( 'NONE', #20745 ) ;
#42087 = CARTESIAN_POINT ( 'NONE',  ( 17.99999999999999645, -104.6166166098442147, -50.11350645393781633 ) ) ;
#42088 = AXIS2_PLACEMENT_3D ( 'NONE', #10842, #37009, #37217 ) ;
#42089 = LINE ( 'NONE', #31877, #8381 ) ;
#42090 = DIRECTION ( 'NONE',  ( -0.7071067811865389130, 0.000000000000000000, 0.7071067811865561215 ) ) ;
#42091 = DIRECTION ( 'NONE',  ( 0.000000000000000000, -1.000000000000000000, 0.000000000000000000 ) ) ;
#42092 = CARTESIAN_POINT ( 'NONE',  ( -12.41726970680908515, 31.00000000000000355, 46.38546114896210071 ) ) ;
#42093 = VERTEX_POINT ( 'NONE', #10009 ) ;
#42094 = CARTESIAN_POINT ( 'NONE',  ( 22.90854556226710415, -14.05525454449572997, -74.83297477053821467 ) ) ;
#42095 = EDGE_CURVE ( 'NONE', #1613, #16471, #37271, .T. ) ;
#42096 = EDGE_LOOP ( 'NONE', ( #9359, #13492 ) ) ;
#42097 = ADVANCED_FACE ( 'NONE', ( #13530 ), #40322, .T. ) ;
#42098 = CARTESIAN_POINT ( 'NONE',  ( 42.05404839982585941, 40.00000000000000000, -47.95475229022623864 ) ) ;
#42099 = DIRECTION ( 'NONE',  ( -1.000000000000000000, 0.000000000000000000, 0.000000000000000000 ) ) ;
#42100 = DIRECTION ( 'NONE',  ( -1.000000000000000000, 0.000000000000000000, -0.000000000000000000 ) ) ;
#42101 = CARTESIAN_POINT ( 'NONE',  ( 0.000000000000000000, 0.000000000000000000, 0.000000000000000000 ) ) ;
#42102 = CIRCLE ( 'NONE', #10072, 116.0000000000000000 ) ;
#42103 = DIRECTION ( 'NONE',  ( -1.000000000000000000, -0.000000000000000000, -0.000000000000000000 ) ) ;
#42104 = ORIENTED_EDGE ( 'NONE', *, *, #38827, .F. ) ;
#42105 = CARTESIAN_POINT ( 'NONE',  ( -26.76192867387533170, 40.00000000000000000, -15.44647709060871321 ) ) ;
#42106 = ORIENTED_EDGE ( 'NONE', *, *, #35665, .F. ) ;
#42107 = CARTESIAN_POINT ( 'NONE',  ( 17.99999999999999645, 46.83041522348496954, 101.9567785075603155 ) ) ;
#42108 = DIRECTION ( 'NONE',  ( 0.000000000000000000, 0.000000000000000000, 1.000000000000000000 ) ) ;
#42109 = VECTOR ( 'NONE', #13978, 1000.000000000000000 ) ;
#42110 = ORIENTED_EDGE ( 'NONE', *, *, #38606, .F. ) ;
#42111 = EDGE_CURVE ( 'NONE', #36025, #3831, #18383, .T. ) ;
#42112 = LINE ( 'NONE', #9391, #2635 ) ;
#42113 = CIRCLE ( 'NONE', #305, 59.00000000000000000 ) ;
#42114 = EDGE_CURVE ( 'NONE', #14037, #43080, #13107, .T. ) ;
#42115 = ORIENTED_EDGE ( 'NONE', *, *, #24368, .F. ) ;
#42116 = DIRECTION ( 'NONE',  ( 0.000000000000000000, 0.000000000000000000, -1.000000000000000000 ) ) ;
#42117 = ORIENTED_EDGE ( 'NONE', *, *, #39785, .T. ) ;
#42118 = VERTEX_POINT ( 'NONE', #6512 ) ;
#42119 = DIRECTION ( 'NONE',  ( 0.000000000000000000, 0.000000000000000000, 1.000000000000000000 ) ) ;
#42120 = CARTESIAN_POINT ( 'NONE',  ( -37.02054590706428172, 31.00000000000000355, -75.34311506435014394 ) ) ;
#42121 = ORIENTED_EDGE ( 'NONE', *, *, #7615, .F. ) ;
#42122 = LINE ( 'NONE', #42551, #770 ) ;
#42123 = CYLINDRICAL_SURFACE ( 'NONE', #26136, 20.00000000000000355 ) ;
#42124 = ORIENTED_EDGE ( 'NONE', *, *, #38620, .T. ) ;
#42125 = EDGE_CURVE ( 'NONE', #26365, #38244, #16609, .T. ) ;
#42127 = VECTOR ( 'NONE', #18238, 1000.000000000000000 ) ;
#42126 = DIRECTION ( 'NONE',  ( -1.000000000000000000, 0.000000000000000000, 0.000000000000000000 ) ) ;
#42128 = CARTESIAN_POINT ( 'NONE',  ( -13.16936484334534008, 40.00000000000000000, 99.04657264458933241 ) ) ;
#42129 = CARTESIAN_POINT ( 'NONE',  ( 24.14050371820132668, 31.00000000000000355, 13.97356841391235704 ) ) ;
#42130 = ADVANCED_FACE ( 'NONE', ( #23357 ), #36618, .F. ) ;
#42132 = CARTESIAN_POINT ( 'NONE',  ( 0.000000000000000000, 0.000000000000000000, -0.2800830152838844622 ) ) ;
#42131 = DIRECTION ( 'NONE',  ( 0.000000000000000000, 0.000000000000000000, 1.000000000000000000 ) ) ;
#42133 = AXIS2_PLACEMENT_3D ( 'NONE', #26863, #36655, #40140 ) ;
#42134 = CARTESIAN_POINT ( 'NONE',  ( 17.99999999999999645, 0.000000000000000000, 0.000000000000000000 ) ) ;
#42135 = CARTESIAN_POINT ( 'NONE',  ( 18.00000000000000355, 8.053585752061904302, 46.81126742072025593 ) ) ;
#42136 = AXIS2_PLACEMENT_3D ( 'NONE', #10155, #34522, #11210 ) ;
#42137 = VERTEX_POINT ( 'NONE', #10232 ) ;
#42138 = FILL_AREA_STYLE_COLOUR ( '', #28838 ) ;
#42139 =( LENGTH_UNIT ( ) NAMED_UNIT ( * ) SI_UNIT ( .MILLI., .METRE. ) );
#42140 = ORIENTED_EDGE ( 'NONE', *, *, #9490, .T. ) ;
#42141 = CIRCLE ( 'NONE', #37267, 58.99999999999999289 ) ;
#42142 = CARTESIAN_POINT ( 'NONE',  ( 17.99999999999999645, -101.8011932243951634, 55.61040422519296555 ) ) ;
#42143 = CARTESIAN_POINT ( 'NONE',  ( -12.69999999999999929, 0.000000000000000000, -12.59999999999999964 ) ) ;
#42144 = EDGE_LOOP ( 'NONE', ( #36806, #555, #1187, #21099 ) ) ;
#42145 = CIRCLE ( 'NONE', #17134, 36.00000000000000000 ) ;
#42146 = CARTESIAN_POINT ( 'NONE',  ( -21.73352778766994575, 40.00000000000000000, 19.07242603999910457 ) ) ;
#42147 = CARTESIAN_POINT ( 'NONE',  ( 10.06970066534629815, 40.00000000000000000, 37.84957806120350199 ) ) ;
#42148 = CIRCLE ( 'NONE', #31028, 0.08401999999999715252 ) ;
#42149 = ORIENTED_EDGE ( 'NONE', *, *, #27985, .F. ) ;
#42150 = VERTEX_POINT ( 'NONE', #23581 ) ;
#42151 = DIRECTION ( 'NONE',  ( 1.000000000000000000, -1.373900992973642263E-15, -3.996523416598957436E-16 ) ) ;
#42152 = CARTESIAN_POINT ( 'NONE',  ( -16.80298683001097260, 31.00000000000000355, -2.367532924972505892 ) ) ;
#42153 = DIRECTION ( 'NONE',  ( 1.000000000000000000, 0.000000000000000000, 0.000000000000000000 ) ) ;
#42154 = DIRECTION ( 'NONE',  ( -1.000000000000000000, -0.000000000000000000, -0.000000000000000000 ) ) ;
#42155 = DIRECTION ( 'NONE',  ( 0.000000000000000000, 0.000000000000000000, 1.000000000000000000 ) ) ;
#42156 = ORIENTED_EDGE ( 'NONE', *, *, #10562, .F. ) ;
#42157 = CARTESIAN_POINT ( 'NONE',  ( -102.4608013043457362, -35.35525454449571470, 14.45886780445633946 ) ) ;
#42158 = ORIENTED_EDGE ( 'NONE', *, *, #29769, .F. ) ;
#42159 = DIRECTION ( 'NONE',  ( 1.000000000000000000, 0.000000000000000000, 0.000000000000000000 ) ) ;
#42160 = AXIS2_PLACEMENT_3D ( 'NONE', #19933, #13373, #10509 ) ;
#42161 = DIRECTION ( 'NONE',  ( -1.000000000000000000, -0.000000000000000000, -0.000000000000000000 ) ) ;
#42162 = CIRCLE ( 'NONE', #36596, 58.99999999999999289 ) ;
#42163 = CARTESIAN_POINT ( 'NONE',  ( 8.999999999999998224, 0.000000000000000000, -12.59999999999999964 ) ) ;
#42164 = EDGE_CURVE ( 'NONE', #1568, #34051, #9943, .T. ) ;
#42165 = CARTESIAN_POINT ( 'NONE',  ( 9.000000000000001776, -115.0622509503831452, -14.72000021165260897 ) ) ;
#42166 = ORIENTED_EDGE ( 'NONE', *, *, #30582, .T. ) ;
#42167 = VERTEX_POINT ( 'NONE', #37915 ) ;
#42168 = CIRCLE ( 'NONE', #6641, 59.00000000000000711 ) ;
#42169 = EDGE_CURVE ( 'NONE', #22999, #1479, #42689, .T. ) ;
#42170 = CARTESIAN_POINT ( 'NONE',  ( 17.99999999999999645, 107.2885202478273783, -54.86040852957203384 ) ) ;
#42171 = ORIENTED_EDGE ( 'NONE', *, *, #2772, .T. ) ;
#42173 = ORIENTED_EDGE ( 'NONE', *, *, #21737, .T. ) ;
#42172 = CARTESIAN_POINT ( 'NONE',  ( 8.999999999999998224, -87.74575819880217864, 75.87280091124445391 ) ) ;
#42174 = CARTESIAN_POINT ( 'NONE',  ( 36.84045577241590763, 31.00000000000000355, -41.86038302678687018 ) ) ;
#42175 = CIRCLE ( 'NONE', #35218, 142.4999999999992610 ) ;
#42176 = ORIENTED_EDGE ( 'NONE', *, *, #36270, .T. ) ;
#42177 = CARTESIAN_POINT ( 'NONE',  ( 18.00000000000000355, -47.49120266317495975, 0.8606222198173691940 ) ) ;
#42178 = CIRCLE ( 'NONE', #38018, 126.0000000000000284 ) ;
#42179 = ADVANCED_FACE ( 'NONE', ( #11327 ), #24658, .F. ) ;
#42180 = CARTESIAN_POINT ( 'NONE',  ( 17.99999999999999645, 0.000000000000000000, 0.000000000000000000 ) ) ;
#42181 = AXIS2_PLACEMENT_3D ( 'NONE', #14694, #11407, #11197 ) ;
#42182 = ORIENTED_EDGE ( 'NONE', *, *, #17921, .F. ) ;
#42183 = CARTESIAN_POINT ( 'NONE',  ( 66.15140951845482675, 39.99999999999999289, -38.07406969931857077 ) ) ;
#42184 = EDGE_CURVE ( 'NONE', #6476, #19975, #14873, .T. ) ;
#42186 = DIRECTION ( 'NONE',  ( -1.000000000000000000, -0.000000000000000000, -0.000000000000000000 ) ) ;
#42185 = DIRECTION ( 'NONE',  ( 0.000000000000000000, 1.000000000000000000, -1.287488025362403787E-15 ) ) ;
#42187 = EDGE_CURVE ( 'NONE', #40723, #23356, #39202, .T. ) ;
#42188 = DIRECTION ( 'NONE',  ( 1.000000000000000000, 0.000000000000000000, 0.000000000000000000 ) ) ;
#42189 = ORIENTED_EDGE ( 'NONE', *, *, #25942, .T. ) ;
#42190 = CYLINDRICAL_SURFACE ( 'NONE', #25887, 99.99999999999994316 ) ;
#42191 = ORIENTED_EDGE ( 'NONE', *, *, #34321, .F. ) ;
#42192 = CARTESIAN_POINT ( 'NONE',  ( -10.00000000000000000, 0.000000000000000000, 0.000000000000000000 ) ) ;
#42193 = CARTESIAN_POINT ( 'NONE',  ( 6.075999999999997847, 0.000000000000000000, 19.11697999999999809 ) ) ;
#42194 = CARTESIAN_POINT ( 'NONE',  ( 61.18335543008118549, 31.00000000000000000, -20.78249587198964576 ) ) ;
#42196 = CARTESIAN_POINT ( 'NONE',  ( 0.000000000000000000, 0.000000000000000000, 0.000000000000000000 ) ) ;
#42195 = DIRECTION ( 'NONE',  ( 0.000000000000000000, 0.000000000000000000, 1.000000000000000000 ) ) ;
#42197 = VECTOR ( 'NONE', #17572, 1000.000000000000000 ) ;
#42198 = EDGE_LOOP ( 'NONE', ( #13695, #14437, #34099, #29984 ) ) ;
#42199 = AXIS2_PLACEMENT_3D ( 'NONE', #2098, #34408, #41157 ) ;
#42200 = CIRCLE ( 'NONE', #29684, 47.49899999999999523 ) ;
#42201 = CIRCLE ( 'NONE', #23442, 59.00000000000000711 ) ;
#42202 = CARTESIAN_POINT ( 'NONE',  ( 17.99999999999999645, 18.25486108452660972, -25.66996392254254644 ) ) ;
#42203 = EDGE_CURVE ( 'NONE', #29542, #3729, #1596, .T. ) ;
#42204 = AXIS2_PLACEMENT_3D ( 'NONE', #38243, #38447, #41731 ) ;
#42205 = VERTEX_POINT ( 'NONE', #34870 ) ;
#42206 = FACE_OUTER_BOUND ( 'NONE', #35632, .T. ) ;
#42207 = EDGE_CURVE ( 'NONE', #23236, #2013, #27405, .T. ) ;
#42208 = FACE_OUTER_BOUND ( 'NONE', #8711, .T. ) ;
#42209 = CARTESIAN_POINT ( 'NONE',  ( 83.51212062385671686, 31.00000000000000000, -48.08891344041042970 ) ) ;
#42211 = CARTESIAN_POINT ( 'NONE',  ( 91.58570893733640617, 39.99999999999999289, -30.97307622143650718 ) ) ;
#42210 = AXIS2_PLACEMENT_3D ( 'NONE', #8275, #25117, #15493 ) ;
#42212 = AXIS2_PLACEMENT_3D ( 'NONE', #12502, #9638, #19491 ) ;
#42213 = CARTESIAN_POINT ( 'NONE',  ( 0.000000000000000000, -23.87611429743677505, 20.54551452399611478 ) ) ;
#42214 = AXIS2_PLACEMENT_3D ( 'NONE', #40567, #11362, #10938 ) ;
#42215 = ORIENTED_EDGE ( 'NONE', *, *, #41190, .F. ) ;
#42216 = CARTESIAN_POINT ( 'NONE',  ( 17.99999999999999645, 111.2721026680460596, -14.38025178762657852 ) ) ;
#42217 = ORIENTED_EDGE ( 'NONE', *, *, #1513, .F. ) ;
#42218 = DIRECTION ( 'NONE',  ( 0.000000000000000000, 0.000000000000000000, 1.000000000000000000 ) ) ;
#42220 = ORIENTED_EDGE ( 'NONE', *, *, #20049, .T. ) ;
#42219 = CARTESIAN_POINT ( 'NONE',  ( 0.000000000000000000, 6.007673836298521586, -35.49518073029990717 ) ) ;
#42221 = CYLINDRICAL_SURFACE ( 'NONE', #33036, 120.5010000000000190 ) ;
#42222 = ORIENTED_EDGE ( 'NONE', *, *, #2057, .T. ) ;
#42223 = DIRECTION ( 'NONE',  ( 1.000000000000000000, 0.000000000000000000, 0.000000000000000000 ) ) ;
#42224 = EDGE_CURVE ( 'NONE', #17691, #9181, #31185, .T. ) ;
#42225 = DIRECTION ( 'NONE',  ( 0.000000000000000000, 0.000000000000000000, 1.000000000000000000 ) ) ;
#42226 = CARTESIAN_POINT ( 'NONE',  ( 17.99999999999999645, -59.47573314508669284, -99.59235496188668435 ) ) ;
#42227 = ORIENTED_EDGE ( 'NONE', *, *, #35064, .T. ) ;
#42228 = CARTESIAN_POINT ( 'NONE',  ( -15.43003214871278139, 31.00000000000000355, -17.59684744742187945 ) ) ;
#42229 = DIRECTION ( 'NONE',  ( 3.009274222672345096E-17, 1.000000000000000000, -2.455023325076454960E-18 ) ) ;
#42230 = AXIS2_PLACEMENT_3D ( 'NONE', #32685, #36162, #23121 ) ;
#42231 = AXIS2_PLACEMENT_3D ( 'NONE', #22763, #32753, #23999 ) ;
#42232 = CIRCLE ( 'NONE', #12314, 59.00000000000000000 ) ;
#42233 = AXIS2_PLACEMENT_3D ( 'NONE', #32624, #12367, #22211 ) ;
#42234 = EDGE_CURVE ( 'NONE', #952, #18374, #32952, .T. ) ;
#42236 = ORIENTED_EDGE ( 'NONE', *, *, #31172, .T. ) ;
#42235 = DIRECTION ( 'NONE',  ( 0.000000000000000000, -0.4817536741017036661, -0.8763066800438700232 ) ) ;
#42237 = UNCERTAINTY_MEASURE_WITH_UNIT (LENGTH_MEASURE( 1.000000000000000082E-05 ), #1625, 'distance_accuracy_value', 'NONE');
#42238 = ORIENTED_EDGE ( 'NONE', *, *, #17496, .T. ) ;
#42239 = DIRECTION ( 'NONE',  ( 0.000000000000000000, 0.000000000000000000, 1.000000000000000000 ) ) ;
#42240 = DIRECTION ( 'NONE',  ( 1.000000000000000000, 0.000000000000000000, 0.000000000000000000 ) ) ;
#42241 = CARTESIAN_POINT ( 'NONE',  ( 44.12914893502614433, 40.00000000000000000, -14.89880614700436645 ) ) ;
#42242 = AXIS2_PLACEMENT_3D ( 'NONE', #7451, #671, #30808 ) ;
#42243 = DIRECTION ( 'NONE',  ( 0.000000000000000000, 0.000000000000000000, 1.000000000000000000 ) ) ;
#42244 = ADVANCED_FACE ( 'NONE', ( #28130 ), #4534, .T. ) ;
#42245 = PRESENTATION_LAYER_ASSIGNMENT (  '', '', ( #442 ) ) ;
#42246 = CARTESIAN_POINT ( 'NONE',  ( -0.6937372685066653943, 4.453844082567723461, -3.610536846335889116 ) ) ;
#42247 = CARTESIAN_POINT ( 'NONE',  ( 17.99999999999999645, -35.54274411428134073, 115.1399337407605259 ) ) ;
#42248 = ORIENTED_EDGE ( 'NONE', *, *, #37767, .F. ) ;
#42249 = DIRECTION ( 'NONE',  ( -1.000000000000000000, 0.000000000000000000, 0.000000000000000000 ) ) ;
#42251 = ORIENTED_EDGE ( 'NONE', *, *, #38185, .T. ) ;
#42250 = AXIS2_PLACEMENT_3D ( 'NONE', #26602, #32702, #36178 ) ;
#42252 = DIRECTION ( 'NONE',  ( 0.000000000000000000, 0.000000000000000000, -1.000000000000000000 ) ) ;
#42253 = CARTESIAN_POINT ( 'NONE',  ( 0.000000000000000000, 0.000000000000000000, 0.000000000000000000 ) ) ;
#42254 = CARTESIAN_POINT ( 'NONE',  ( 8.528031178950213231, 31.00000000000000355, -31.86521141804621493 ) ) ;
#42255 = EDGE_LOOP ( 'NONE', ( #6157, #36305, #36173, #35099 ) ) ;
#42256 = LINE ( 'NONE', #38774, #35081 ) ;
#42257 = ORIENTED_EDGE ( 'NONE', *, *, #30693, .F. ) ;
#42258 = AXIS2_PLACEMENT_3D ( 'NONE', #12360, #12777, #38936 ) ;
#42259 = CYLINDRICAL_SURFACE ( 'NONE', #14984, 120.5010000000000190 ) ;
#42260 = CARTESIAN_POINT ( 'NONE',  ( 74.70319961851696178, 31.00000000000000000, -57.31929289364909152 ) ) ;
#42261 = ADVANCED_FACE ( 'NONE', ( #38141 ), #8264, .T. ) ;
#42262 = DIRECTION ( 'NONE',  ( 1.000000000000000000, -1.373900992973642066E-15, -3.979293995072266947E-16 ) ) ;
#42264 = ORIENTED_EDGE ( 'NONE', *, *, #37174, .F. ) ;
#42263 = AXIS2_PLACEMENT_3D ( 'NONE', #11746, #15248, #18952 ) ;
#42265 = CARTESIAN_POINT ( 'NONE',  ( 21.04585062970478759, 31.00000000000000355, -61.66509230325024049 ) ) ;
#42266 = EDGE_CURVE ( 'NONE', #25997, #28092, #19731, .T. ) ;
#42267 = CARTESIAN_POINT ( 'NONE',  ( -12.78314611188302052, 40.00000000000000000, 97.07982689498881257 ) ) ;
#42268 = AXIS2_PLACEMENT_3D ( 'NONE', #10793, #24123, #19088 ) ;
#42269 = ORIENTED_EDGE ( 'NONE', *, *, #11556, .T. ) ;
#42270 = AXIS2_PLACEMENT_3D ( 'NONE', #26197, #39472, #20482 ) ;
#42271 = LINE ( 'NONE', #34668, #33159 ) ;
#42272 = AXIS2_PLACEMENT_3D ( 'NONE', #4338, #8649, #37724 ) ;
#42273 = CARTESIAN_POINT ( 'NONE',  ( 17.99999999999999645, 0.000000000000000000, 0.000000000000000000 ) ) ;
#42274 = CARTESIAN_POINT ( 'NONE',  ( 17.99999999999999645, 30.74337109795208178, 8.695908345466650147 ) ) ;
#42275 = VECTOR ( 'NONE', #17599, 1000.000000000000000 ) ;
#42277 = ORIENTED_EDGE ( 'NONE', *, *, #37666, .F. ) ;
#42276 = CARTESIAN_POINT ( 'NONE',  ( 18.00000000000000355, 0.6505223195690489346, -51.99593080916756804 ) ) ;
#42279 = CIRCLE ( 'NONE', #6782, 59.00000000000000000 ) ;
#42278 = FACE_OUTER_BOUND ( 'NONE', #26387, .T. ) ;
#42280 = DIRECTION ( 'NONE',  ( 0.000000000000000000, 0.000000000000000000, 1.000000000000000000 ) ) ;
#42281 = AXIS2_PLACEMENT_3D ( 'NONE', #8402, #41109, #38070 ) ;
#42282 = ORIENTED_EDGE ( 'NONE', *, *, #40638, .F. ) ;
#42283 = CARTESIAN_POINT ( 'NONE',  ( 74.72486387243833406, 39.99999999999999289, 9.837939412698395003 ) ) ;
#42284 = ADVANCED_FACE ( 'NONE', ( #24890 ), #40971, .F. ) ;
#42285 = CARTESIAN_POINT ( 'NONE',  ( -106.4195705685756081, 106.4195705685752529, 9.999999999999998224 ) ) ;
#42286 = AXIS2_PLACEMENT_3D ( 'NONE', #27360, #10553, #26926 ) ;
#42287 = ORIENTED_EDGE ( 'NONE', *, *, #32241, .T. ) ;
#42288 = DIRECTION ( 'NONE',  ( 0.000000000000000000, 0.000000000000000000, 1.000000000000000000 ) ) ;
#42289 = VERTEX_POINT ( 'NONE', #20964 ) ;
#42290 = EDGE_CURVE ( 'NONE', #40845, #25590, #28789, .T. ) ;
#42291 = ORIENTED_EDGE ( 'NONE', *, *, #22685, .T. ) ;
#42292 = DIRECTION ( 'NONE',  ( 0.000000000000000000, 0.7164567402983164079, -0.6976315211349833900 ) ) ;
#42293 = ORIENTED_EDGE ( 'NONE', *, *, #26825, .F. ) ;
#42294 = CARTESIAN_POINT ( 'NONE',  ( 17.99999999999999645, 0.000000000000000000, 0.000000000000000000 ) ) ;
#42295 = DIRECTION ( 'NONE',  ( 1.000000000000000000, 0.000000000000000000, 0.000000000000000000 ) ) ;
#42296 = EDGE_CURVE ( 'NONE', #28773, #596, #34332, .T. ) ;
#42297 = AXIS2_PLACEMENT_3D ( 'NONE', #23274, #40007, #528 ) ;
#42298 = CARTESIAN_POINT ( 'NONE',  ( 17.99999999999999645, -107.1354928292866759, -44.47455650398174498 ) ) ;
#42299 = CARTESIAN_POINT ( 'NONE',  ( -107.9608013043457930, -14.05525454449570866, 14.45886780445738395 ) ) ;
#42300 = ORIENTED_EDGE ( 'NONE', *, *, #5774, .T. ) ;
#42301 = CIRCLE ( 'NONE', #20747, 58.99999999999999289 ) ;
#42302 = CARTESIAN_POINT ( 'NONE',  ( -12.50000000000000000, 1.530808498934191521E-15, -25.00000000000000000 ) ) ;
#42303 = ORIENTED_EDGE ( 'NONE', *, *, #16505, .F. ) ;
#42304 = AXIS2_PLACEMENT_3D ( 'NONE', #37231, #28946, #12578 ) ;
#42305 = CARTESIAN_POINT ( 'NONE',  ( 0.000000000000000000, 39.55064067543064965, 25.36340625197373555 ) ) ;
#42306 = ORIENTED_EDGE ( 'NONE', *, *, #21666, .T. ) ;
#42307 = CARTESIAN_POINT ( 'NONE',  ( 8.999999999999998224, -68.63002662989681824, -93.51962064069581970 ) ) ;
#42308 = AXIS2_PLACEMENT_3D ( 'NONE', #2663, #35624, #42802 ) ;
#42309 = CARTESIAN_POINT ( 'NONE',  ( 17.99999999999999645, 0.000000000000000000, 0.000000000000000000 ) ) ;
#42310 = CARTESIAN_POINT ( 'NONE',  ( 18.00000000000000355, 0.000000000000000000, 0.000000000000000000 ) ) ;
#42311 = CARTESIAN_POINT ( 'NONE',  ( 54.89583333452979730, 31.00000000000000355, -3.599741573803383332 ) ) ;
#42312 = VERTEX_POINT ( 'NONE', #17685 ) ;
#42313 = CARTESIAN_POINT ( 'NONE',  ( 1.734723475976807094E-15, 4.618802153517012954, -0.4999999999999995559 ) ) ;
#42314 = AXIS2_PLACEMENT_3D ( 'NONE', #32229, #8458, #21820 ) ;
#42315 = EDGE_CURVE ( 'NONE', #25188, #2586, #26686, .T. ) ;
#42316 = EDGE_CURVE ( 'NONE', #10423, #17165, #42717, .T. ) ;
#42317 = VERTEX_POINT ( 'NONE', #21178 ) ;
#42318 = ADVANCED_FACE ( 'NONE', ( #34428 ), #22461, .T. ) ;
#42319 = EDGE_CURVE ( 'NONE', #4351, #31916, #36427, .T. ) ;
#42320 = CARTESIAN_POINT ( 'NONE',  ( 64.78932475141161262, 39.99999999999999289, 8.528958657501300777 ) ) ;
#42321 = DIRECTION ( 'NONE',  ( 0.000000000000000000, 0.5076658003388410112, -0.8615540813938056264 ) ) ;
#42322 = DIRECTION ( 'NONE',  ( 0.000000000000000000, 1.000000000000000000, 0.000000000000000000 ) ) ;
#42323 = AXIS2_PLACEMENT_3D ( 'NONE', #29532, #35627, #42803 ) ;
#42324 = MANIFOLD_SOLID_BREP ( 'Extrude-Thin1', #1724 ) ;
#42325 = EDGE_CURVE ( 'NONE', #7533, #41913, #15682, .T. ) ;
#42326 = CARTESIAN_POINT ( 'NONE',  ( 0.000000000000000000, -97.89532456239533076, 54.81585448086167389 ) ) ;
#42327 = FACE_OUTER_BOUND ( 'NONE', #34143, .T. ) ;
#42328 = AXIS2_PLACEMENT_3D ( 'NONE', #21190, #4545, #13766 ) ;
#42329 = VECTOR ( 'NONE', #30703, 1000.000000000000000 ) ;
#42330 = VERTEX_POINT ( 'NONE', #42676 ) ;
#42331 = CARTESIAN_POINT ( 'NONE',  ( -38.45388554590046937, 40.00000000000000000, -13.05014827191142679 ) ) ;
#42332 = AXIS2_PLACEMENT_3D ( 'NONE', #21457, #17312, #31003 ) ;
#42333 = CARTESIAN_POINT ( 'NONE',  ( -12.55910585664918422, 0.7408941433508191565, -1.199999999999999956 ) ) ;
#42334 = FACE_OUTER_BOUND ( 'NONE', #14389, .T. ) ;
#42335 = AXIS2_PLACEMENT_3D ( 'NONE', #9020, #38681, #32360 ) ;
#42336 = ORIENTED_EDGE ( 'NONE', *, *, #1044, .T. ) ;
#42337 = AXIS2_PLACEMENT_3D ( 'NONE', #38852, #2187, #5898 ) ;
#42338 = DIRECTION ( 'NONE',  ( 0.000000000000000000, 0.1062934856473589651, 0.9943348002101377592 ) ) ;
#42339 = ORIENTED_EDGE ( 'NONE', *, *, #4703, .F. ) ;
#42340 = DIRECTION ( 'NONE',  ( -1.000000000000000000, 0.000000000000000000, -0.000000000000000000 ) ) ;
#42341 = ORIENTED_EDGE ( 'NONE', *, *, #39441, .T. ) ;
#42342 = ORIENTED_EDGE ( 'NONE', *, *, #24792, .T. ) ;
#42343 = CARTESIAN_POINT ( 'NONE',  ( -10.00000000000000000, 0.000000000000000000, 0.000000000000000000 ) ) ;
#42344 = AXIS2_PLACEMENT_3D ( 'NONE', #20902, #17184, #34151 ) ;
#42345 = CARTESIAN_POINT ( 'NONE',  ( 64.75392801420538547, 31.00000000000000000, -56.64582372546510669 ) ) ;
#42346 = ORIENTED_EDGE ( 'NONE', *, *, #21887, .F. ) ;
#42347 = CARTESIAN_POINT ( 'NONE',  ( 0.000000000000000000, 111.8797445107943531, 8.437727291344614855 ) ) ;
#42348 = DIRECTION ( 'NONE',  ( -1.000000000000000000, 3.469446951953614189E-17, 0.000000000000000000 ) ) ;
#42349 = B_SPLINE_CURVE_WITH_KNOTS ( 'NONE', 3,
 ( #12803, #25909, #32646, #19583, #2295, #2933, #26115, #22873, #32427, #42228, #12390, #16087, #42872, #5804, #22437, #39170, #8653, #38961, #39380, #22647, #22234, #6022, #42653, #22010, #29387, #6237, #32853, #16294, #13029, #35266, #5392, #18757, #35685, #32013, #2095, #19159, #28754, #25490, #38750, #8880, #35478, #18962, #32216, #25711, #2511, #33293, #36536, #26969, #7302, #3375, #36765, #40247, #13671, #3150, #40460, #16744, #4022, #20667, #40018, #10592, #16523, #19794, #33934, #3790, #10150, #9935, #17397, #6444, #16954, #302, #26536, #33498, #39808, #30035, #30674, #23925, #29826, #39602, #749, #27190, #6660, #541, #10380, #7090, #14108, #85, #9731, #13891, #37192, #20235, #13456, #26749, #17175, #23080, #6880, #23501, #23718, #36327, #3581, #33061, #36980, #20443, #30237, #30459, #43092, #33706, #13242, #23284, #20024, #5116, #28060, #21550, #41550, #14543, #1842, #18061, #27846, #20894, #34576, #34145, #4242, #31322, #14973, #10816, #4686, #34359, #1405, #38064, #34798, #37411, #41103, #14759, #41320, #11469, #38277, #18478, #14312, #30883, #31102, #11695, #962, #17614, #7535, #17826, #24807, #37835, #27624, #28279, #1188, #31748, #4907, #11256, #8186, #40892, #25036, #24585, #1620, #35007, #7959, #4455, #8394, #21758, #27399, #21324, #18269, #31534, #40666, #24147, #11048, #24374, #37626, #7747, #21106, #16038, #42402, #15823, #35217, #35637, #25237, #32593, #15606, #22597, #35839, #32801, #12119, #41767, #38919, #22180, #18707, #5966, #18911, #22390, #41971, #25659, #15409, #35436, #5555, #42603, #2247, #2676, #19112, #12546, #5754, #19324, #15203, #2460, #12755, #29337, #9246, #36066, #29130, #26060, #39323, #28910, #28505, #32375, #42174, #8599, #25862, #21961, #5341, #39126, #9461, #11910, #22816, #32168, #6188, #19533, #38482, #31971, #12336, #2047, #28706, #25439, #38701, #8824, #9034, #6397, #6602, #30409, #19744, #9684, #26278, #36485, #6830, #13404, #33007, #3737, #19971, #23879, #23671, #33240, #26916, #3094, #484, #29983, #20395, #10541, #3321, #9887, #13843, #33655, #17120, #36, #16697, #10329, #26700, #7250, #30188, #249, #36277, #23028, #27144, #40407, #13620, #3533, #16465, #23447, #12973, #37142, #39967, #36928, #7040, #20608, #43041, #29545, #10097, #23237, #29768, #2882, #36712, #20189, #13194, #33447, #26485, #16909, #40192, #16246, #42814, #39549, #39757, #14917, #28221, #21495, #695, #11638, #38002, #37788, #1355, #1570, #27565, #41487, #8130, #34746, #14487, #24324, #37580, #41270, #24980, #31044, #34308, #21056, #20842, #38226, #8343, #4854, #14056, #33883, #18213, #7907, #14702, #3971, #40839, #17350, #31484, #30628, #27796, #7689, #4401, #11414, #27350, #17773, #21269, #40613, #1136, #10759, #34516, #4185, #24093, #41053, #11203, #37363, #7480, #24536, #4629, #18005, #31269, #34098, #17561, #30835, #907, #28009, #24751, #14261, #10994, #28446, #41714, #15766, #11858, #28853, #21908, #25605, #32117, #15355, #18651, #8984, #32538, #28646, #18857, #22334, #38863, #12700, #8550, #25183, #25385, #5911, #38431, #26005, #35161, #1785, #15985, #29075, #22125, #5280, #29282, #31688, #42120, #35582, #31915, #15558, #1995, #5500, #39066, #42549, #8765, #41919, #19264, #12067, #2626, #42345, #39266, #12492, #2198, #22544, #5065, #38644, #35384, #12277, #5702, #25809, #19058, #32320, #2400, #9192, #15145, #35780, #21698, #34954, #18423, #36877, #3035, #33177, #39915, #32956, #9833, #2828, #33395, #42754, #26648, #29932, #9630, #29707, #42983, #6985, #13141, #20342, #33605, #3687, #36430, #26860, #17065, #39702, #16406, #30350, #39494, #426, #16858, #13792, #30142, #3266, #10272, #36651, #6778, #12914, #16192, #23619, #27088, #20138, #10045, #29490, #19854, #19481, #40133, #23185, #9399, #22752, #36008, #26432, #16645, #23389, #6546, #26218, #197, #19910, #13354, #36222, #3481, #22978, #13566, #6134, #32745, #6342, #19690, #24695, #3910, #40355, #1517, #27961, #37311, #17298, #21004, #7855, #8075, #34047, #34693, #14654, #41216, #34255, #30782, #858, #4574, #18168, #37532, #40784 ),
 .UNSPECIFIED., .F., .F.,
 ( 4, 2, 2, 2, 2, 2, 2, 2, 2, 2, 2, 2, 2, 2, 2, 2, 2, 2, 2, 2, 2, 2, 2, 2, 2, 2, 2, 2, 2, 2, 2, 2, 2, 2, 2, 2, 2, 2, 2, 2, 2, 2, 2, 2, 2, 2, 2, 2, 2, 2, 2, 2, 2, 2, 2, 2, 2, 2, 2, 2, 2, 2, 2, 2, 2, 2, 2, 2, 2, 2, 2, 2, 2, 2, 2, 2, 2, 2, 2, 2, 2, 2, 2, 2, 2, 2, 2, 2, 2, 2, 2, 2, 2, 2, 2, 2, 2, 2, 2, 2, 2, 2, 2, 2, 2, 2, 2, 2, 2, 2, 2, 2, 2, 2, 2, 2, 2, 2, 2, 2, 2, 2, 2, 2, 2, 2, 2, 2, 2, 2, 2, 2, 2, 2, 2, 2, 2, 2, 2, 2, 2, 2, 2, 2, 2, 2, 2, 2, 2, 2, 2, 2, 2, 2, 2, 2, 2, 2, 2, 2, 2, 2, 2, 2, 2, 2, 2, 2, 2, 2, 2, 2, 2, 2, 2, 2, 2, 2, 2, 2, 2, 2, 2, 2, 2, 2, 2, 2, 2, 2, 2, 2, 2, 2, 2, 2, 2, 2, 2, 2, 2, 2, 2, 2, 2, 2, 2, 2, 2, 2, 2, 2, 2, 2, 2, 2, 2, 2, 2, 2, 2, 2, 2, 2, 2, 2, 2, 2, 2, 2, 2, 2, 2, 2, 2, 2, 2, 2, 2, 2, 2, 2, 2, 2, 2, 2, 2, 2, 2, 2, 2, 2, 2, 2, 2, 2, 4 ),
 ( 0.000000000000000000, 0.003906250000000000000, 0.007812500000000000000, 0.01171875000000000000, 0.01562500000000000000, 0.01953125000000000000, 0.02343750000000000000, 0.02734375000000000000, 0.03125000000000000000, 0.03515625000000000000, 0.03906250000000000000, 0.04296875000000000000, 0.04687500000000000000, 0.05078125000000000000, 0.05468750000000000000, 0.05859375000000000000, 0.06250000000000000000, 0.06640625000000000000, 0.07031250000000000000, 0.07421875000000000000, 0.07812500000000000000, 0.08203125000000000000, 0.08593750000000000000, 0.08984375000000000000, 0.09375000000000000000, 0.09765625000000000000, 0.1015625000000000000, 0.1054687500000000000, 0.1093750000000000000, 0.1132812500000000000, 0.1171875000000000000, 0.1210937500000000000, 0.1250000000000000000, 0.1289062500000000000, 0.1328125000000000000, 0.1367187500000000000, 0.1406250000000000000, 0.1445312500000000000, 0.1484375000000000000, 0.1523437500000000000, 0.1562500000000000000, 0.1601562500000000000, 0.1640625000000000000, 0.1679687500000000000, 0.1718750000000000000, 0.1757812500000000000, 0.1796875000000000000, 0.1835937500000000000, 0.1875000000000000000, 0.1914062500000000000, 0.1953125000000000000, 0.1992187500000000000, 0.2031250000000000000, 0.2070312500000000000, 0.2109375000000000000, 0.2148437500000000000, 0.2187500000000000000, 0.2226562500000000000, 0.2265625000000000000, 0.2304687500000000000, 0.2343750000000000000, 0.2382812500000000000, 0.2421875000000000000, 0.2460937500000000000, 0.2500000000000000000, 0.2539062500000000000, 0.2578125000000000000, 0.2617187500000000000, 0.2656250000000000000, 0.2695312500000000000, 0.2734375000000000000, 0.2773437500000000000, 0.2812500000000000000, 0.2851562500000000000, 0.2890625000000000000, 0.2929687500000000000, 0.2968750000000000000, 0.3007812500000000000, 0.3046875000000000000, 0.3085937500000000000, 0.3125000000000000000, 0.3164062500000000000, 0.3203125000000000000, 0.3242187500000000000, 0.3281250000000000000, 0.3320312500000000000, 0.3359375000000000000, 0.3398437500000000000, 0.3437500000000000000, 0.3476562500000000000, 0.3515625000000000000, 0.3554687500000000000, 0.3593750000000000000, 0.3632812500000000000, 0.3671875000000000000, 0.3710937500000000000, 0.3750000000000000000, 0.3789062500000000000, 0.3828125000000000000, 0.3867187500000000000, 0.3906250000000000000, 0.3945312500000000000, 0.3984375000000000000, 0.4023437500000000000, 0.4062500000000000000, 0.4101562500000000000, 0.4140625000000000000, 0.4179687500000000000, 0.4218750000000000000, 0.4257812500000000000, 0.4296875000000000000, 0.4335937500000000000, 0.4375000000000000000, 0.4414062500000000000, 0.4453125000000000000, 0.4492187500000000000, 0.4531250000000000000, 0.4570312500000000000, 0.4609375000000000000, 0.4648437500000000000, 0.4687500000000000000, 0.4726562500000000000, 0.4765625000000000000, 0.4804687500000000000, 0.4843750000000000000, 0.4882812500000000000, 0.4921875000000000000, 0.4960937500000000000, 0.5000000000000000000, 0.5039062500000000000, 0.5078125000000000000, 0.5117187500000000000, 0.5156250000000000000, 0.5195312500000000000, 0.5234375000000000000, 0.5273437500000000000, 0.5312500000000000000, 0.5351562500000000000, 0.5390625000000000000, 0.5429687500000000000, 0.5468750000000000000, 0.5507812500000000000, 0.5546875000000000000, 0.5585937500000000000, 0.5625000000000000000, 0.5664062500000000000, 0.5703125000000000000, 0.5742187500000000000, 0.5781250000000000000, 0.5820312500000000000, 0.5859375000000000000, 0.5898437500000000000, 0.5937500000000000000, 0.5976562500000000000, 0.6015625000000000000, 0.6054687500000000000, 0.6093750000000000000, 0.6132812500000000000, 0.6171875000000000000, 0.6210937500000000000, 0.6250000000000000000, 0.6289062500000000000, 0.6328125000000000000, 0.6367187500000000000, 0.6406250000000000000, 0.6445312500000000000, 0.6484375000000000000, 0.6523437500000000000, 0.6562500000000000000, 0.6601562500000000000, 0.6640625000000000000, 0.6679687500000000000, 0.6718750000000000000, 0.6757812500000000000, 0.6796875000000000000, 0.6835937500000000000, 0.6875000000000000000, 0.6914062500000000000, 0.6953125000000000000, 0.6992187500000000000, 0.7031250000000000000, 0.7070312500000000000, 0.7109375000000000000, 0.7148437500000000000, 0.7187500000000000000, 0.7226562500000000000, 0.7265625000000000000, 0.7304687500000000000, 0.7343750000000000000, 0.7382812500000000000, 0.7421875000000000000, 0.7460937500000000000, 0.7500000000000000000, 0.7539062500000000000, 0.7578125000000000000, 0.7617187500000000000, 0.7656250000000000000, 0.7695312500000000000, 0.7734375000000000000, 0.7773437500000000000, 0.7812500000000000000, 0.7851562500000000000, 0.7890625000000000000, 0.7929687500000000000, 0.7968750000000000000, 0.8007812500000000000, 0.8046875000000000000, 0.8085937500000000000, 0.8125000000000000000, 0.8164062500000000000, 0.8203125000000000000, 0.8242187500000000000, 0.8281250000000000000, 0.8320312500000000000, 0.8359375000000000000, 0.8398437500000000000, 0.8437500000000000000, 0.8476562500000000000, 0.8515625000000000000, 0.8554687500000000000, 0.8593750000000000000, 0.8632812500000000000, 0.8671875000000000000, 0.8710937500000000000, 0.8750000000000000000, 0.8789062500000000000, 0.8828125000000000000, 0.8867187500000000000, 0.8906250000000000000, 0.8945312500000000000, 0.8984375000000000000, 0.9023437500000000000, 0.9062500000000000000, 0.9101562500000000000, 0.9140625000000000000, 0.9179687500000000000, 0.9218750000000000000, 0.9257812500000000000, 0.9296875000000000000, 0.9335937500000000000, 0.9375000000000000000, 0.9414062500000000000, 0.9453125000000000000, 0.9492187500000000000, 0.9531250000000000000, 0.9570312500000000000, 0.9609375000000000000, 0.9648437500000000000, 0.9687500000000000000, 0.9726562500000000000, 0.9765625000000000000, 0.9804687500000000000, 0.9843750000000000000, 0.9882812500000000000, 0.9921875000000000000, 0.9960937500000000000, 1.000000000000000000 ),
 .UNSPECIFIED. ) ;
#42350 = ORIENTED_EDGE ( 'NONE', *, *, #39694, .F. ) ;
#42351 = FACE_OUTER_BOUND ( 'NONE', #365, .T. ) ;
#42352 = CARTESIAN_POINT ( 'NONE',  ( 25.57473013256711880, 40.00000000000000000, 95.94174708832935039 ) ) ;
#42353 = CARTESIAN_POINT ( 'NONE',  ( 17.99999999999999645, -31.81777574834308098, 2.898764365605205562 ) ) ;
#42354 = CIRCLE ( 'NONE', #33311, 47.49900000000000233 ) ;
#42355 = CIRCLE ( 'NONE', #25115, 116.0000000000000000 ) ;
#42357 = DIRECTION ( 'NONE',  ( 0.000000000000000000, 0.000000000000000000, -1.000000000000000000 ) ) ;
#42356 = DIRECTION ( 'NONE',  ( 0.000000000000000000, 0.000000000000000000, 1.000000000000000000 ) ) ;
#42358 = CARTESIAN_POINT ( 'NONE',  ( 17.99999999999999645, 0.000000000000000000, 0.000000000000000000 ) ) ;
#42359 = CARTESIAN_POINT ( 'NONE',  ( 17.99999999999999645, -106.5605152861899256, -56.26142179985931335 ) ) ;
#42360 = AXIS2_PLACEMENT_3D ( 'NONE', #3415, #25944, #19200 ) ;
#42361 = ORIENTED_EDGE ( 'NONE', *, *, #26266, .F. ) ;
#42362 = AXIS2_PLACEMENT_3D ( 'NONE', #11727, #25065, #38304 ) ;
#42363 = FILL_AREA_STYLE ('',( #41507 ) ) ;
#42364 = AXIS2_PLACEMENT_3D ( 'NONE', #10113, #40209, #29782 ) ;
#42365 = CARTESIAN_POINT ( 'NONE',  ( 3.579113344806025054, 31.00000000000000355, 27.11441211503905535 ) ) ;
#42366 = CIRCLE ( 'NONE', #22938, 51.99999999999999289 ) ;
#42367 = EDGE_LOOP ( 'NONE', ( #10917, #19231, #3546, #25876 ) ) ;
#42368 = DIRECTION ( 'NONE',  ( -1.000000000000000000, 0.000000000000000000, 0.000000000000000000 ) ) ;
#42369 = CARTESIAN_POINT ( 'NONE',  ( 0.000000000000000000, -18.35539002514308038, -110.6858262410711831 ) ) ;
#42371 = EDGE_LOOP ( 'NONE', ( #40295, #27195, #11555, #4964 ) ) ;
#42370 = AXIS2_PLACEMENT_3D ( 'NONE', #2508, #15872, #16289 ) ;
#42372 = ADVANCED_FACE ( 'NONE', ( #28571 ), #8677, .T. ) ;
#42373 = EDGE_CURVE ( 'NONE', #8238, #28805, #9546, .T. ) ;
#42374 = CARTESIAN_POINT ( 'NONE',  ( 24.89583333603155069, 40.00000000000000000, -1.636246165087041016 ) ) ;
#42375 = CARTESIAN_POINT ( 'NONE',  ( -26.24023198663969580, 40.00000000000000000, -20.19409642360271917 ) ) ;
#42376 = ADVANCED_FACE ( 'NONE', ( #15480 ), #22038, .T. ) ;
#42377 = ORIENTED_EDGE ( 'NONE', *, *, #12743, .F. ) ;
#42378 = VERTEX_POINT ( 'NONE', #32668 ) ;
#42379 = CYLINDRICAL_SURFACE ( 'NONE', #28399, 116.0000000000000000 ) ;
#42380 = CARTESIAN_POINT ( 'NONE',  ( 0.000000000000000000, 0.000000000000000000, 0.000000000000000000 ) ) ;
#42381 = CARTESIAN_POINT ( 'NONE',  ( 0.000000000000000000, -2.007101075700183035, 31.43498920425968990 ) ) ;
#42382 = EDGE_CURVE ( 'NONE', #21931, #34938, #20484, .T. ) ;
#42383 = FACE_OUTER_BOUND ( 'NONE', #22954, .T. ) ;
#42384 = ORIENTED_EDGE ( 'NONE', *, *, #33949, .T. ) ;
#42385 = DIRECTION ( 'NONE',  ( -1.000000000000000000, 0.000000000000000000, 0.000000000000000000 ) ) ;
#42386 = ORIENTED_EDGE ( 'NONE', *, *, #41449, .F. ) ;
#42387 = CYLINDRICAL_SURFACE ( 'NONE', #34062, 120.5010000000000190 ) ;
#42388 = DIRECTION ( 'NONE',  ( -0.2140725878556618000, 0.9768177553304300265, 2.796485154102059642E-15 ) ) ;
#42389 = EDGE_CURVE ( 'NONE', #6539, #10288, #38558, .T. ) ;
#42390 = VECTOR ( 'NONE', #19901, 1000.000000000000000 ) ;
#42391 = AXIS2_PLACEMENT_3D ( 'NONE', #34401, #4741, #7580 ) ;
#42392 = DIRECTION ( 'NONE',  ( 0.000000000000000000, 0.000000000000000000, -1.000000000000000000 ) ) ;
#42393 = FACE_OUTER_BOUND ( 'NONE', #41821, .T. ) ;
#42394 = VERTEX_POINT ( 'NONE', #16110 ) ;
#42395 = CARTESIAN_POINT ( 'NONE',  ( -87.52616871875942195, 40.00000000000000711, -23.43677886868077209 ) ) ;
#42396 = VERTEX_POINT ( 'NONE', #15902 ) ;
#42397 = AXIS2_PLACEMENT_3D ( 'NONE', #28490, #18254, #1607 ) ;
#42398 = DIRECTION ( 'NONE',  ( -3.009274222672345096E-17, -1.000000000000000000, 2.455023325076455345E-18 ) ) ;
#42399 = EDGE_LOOP ( 'NONE', ( #26719, #40115, #12104, #5548 ) ) ;
#42401 = VERTEX_POINT ( 'NONE', #42038 ) ;
#42400 = DIRECTION ( 'NONE',  ( 0.000000000000000000, 1.000000000000000000, 0.000000000000000000 ) ) ;
#42402 = CARTESIAN_POINT ( 'NONE',  ( 12.64472494877221997, 31.00000000000000355, 47.53373494968589341 ) ) ;
#42403 = ORIENTED_EDGE ( 'NONE', *, *, #39991, .F. ) ;
#42404 = CARTESIAN_POINT ( 'NONE',  ( -105.9879088449591933, 40.00000000000000000, 2.119280070842335384 ) ) ;
#42405 = EDGE_CURVE ( 'NONE', #40129, #28564, #42256, .T. ) ;
#42406 = CARTESIAN_POINT ( 'NONE',  ( 0.000000000000000000, 0.000000000000000000, 0.000000000000000000 ) ) ;
#42407 = ORIENTED_EDGE ( 'NONE', *, *, #30326, .T. ) ;
#42408 = CARTESIAN_POINT ( 'NONE',  ( 51.69257347811147696, 40.00000000000000000, 59.10123636508003386 ) ) ;
#42410 = CARTESIAN_POINT ( 'NONE',  ( 17.99999999999999645, 113.8630351447208824, -22.16324045874292636 ) ) ;
#42409 = DIRECTION ( 'NONE',  ( 0.000000000000000000, 0.000000000000000000, 1.000000000000000000 ) ) ;
#42411 = CARTESIAN_POINT ( 'NONE',  ( 0.000000000000000000, 35.78484819117785776, -110.3423972910429143 ) ) ;
#42412 = VERTEX_POINT ( 'NONE', #8903 ) ;
#42413 = FACE_OUTER_BOUND ( 'NONE', #2627, .T. ) ;
#42414 = ORIENTED_EDGE ( 'NONE', *, *, #20698, .F. ) ;
#42415 = DIRECTION ( 'NONE',  ( 0.000000000000000000, 0.000000000000000000, 1.000000000000000000 ) ) ;
#42416 = LINE ( 'NONE', #16055, #24056 ) ;
#42417 = CARTESIAN_POINT ( 'NONE',  ( -5.399612364985466151, 31.00000000000000355, -82.39583333413678190 ) ) ;
#42418 = VECTOR ( 'NONE', #31746, 1000.000000000000000 ) ;
#42420 = DIRECTION ( 'NONE',  ( -1.000000000000000000, -0.000000000000000000, -0.000000000000000000 ) ) ;
#42419 = DIRECTION ( 'NONE',  ( 0.000000000000000000, -0.9714298932647122964, 0.2373266998711055509 ) ) ;
#42421 = AXIS2_PLACEMENT_3D ( 'NONE', #2509, #6018, #42444 ) ;
#42422 = ORIENTED_EDGE ( 'NONE', *, *, #18277, .F. ) ;
#42423 = EDGE_CURVE ( 'NONE', #29146, #33962, #5800, .T. ) ;
#42424 = CIRCLE ( 'NONE', #4820, 58.99999999999999289 ) ;
#42425 = CARTESIAN_POINT ( 'NONE',  ( 17.99999999999999645, 110.3490479609629489, 20.28201389785587949 ) ) ;
#42426 = ORIENTED_EDGE ( 'NONE', *, *, #22924, .T. ) ;
#42427 = CARTESIAN_POINT ( 'NONE',  ( 17.99999999999999645, 13.22719389141978930, 28.58720592780601066 ) ) ;
#42428 = DIRECTION ( 'NONE',  ( -1.000000000000000000, -0.000000000000000000, -0.000000000000000000 ) ) ;
#42429 = CARTESIAN_POINT ( 'NONE',  ( -59.98614492175870794, 31.00000000000000711, 68.21249229744711329 ) ) ;
#42430 = CARTESIAN_POINT ( 'NONE',  ( -87.75478321342750121, 40.00000000000000711, -29.92102470460831753 ) ) ;
#42431 = EDGE_CURVE ( 'NONE', #12907, #14877, #28818, .T. ) ;
#42432 = CARTESIAN_POINT ( 'NONE',  ( 0.000000000000000000, 51.85248208264521708, -3.914090171285657949 ) ) ;
#42433 = EDGE_CURVE ( 'NONE', #27860, #38361, #23966, .T. ) ;
#42434 = ORIENTED_EDGE ( 'NONE', *, *, #20110, .F. ) ;
#42435 = DIRECTION ( 'NONE',  ( 0.000000000000000000, 0.000000000000000000, 1.000000000000000000 ) ) ;
#42436 = VERTEX_POINT ( 'NONE', #13263 ) ;
#42437 = CARTESIAN_POINT ( 'NONE',  ( 4.000000000000000000, 2.309401076758497151, -3.433295621305379353 ) ) ;
#42438 = EDGE_CURVE ( 'NONE', #22974, #36853, #4388, .T. ) ;
#42439 = DIRECTION ( 'NONE',  ( 0.000000000000000000, 0.000000000000000000, 1.000000000000000000 ) ) ;
#42440 = DIRECTION ( 'NONE',  ( 1.000000000000000000, 0.000000000000000000, 0.000000000000000000 ) ) ;
#42441 = EDGE_LOOP ( 'NONE', ( #23574, #15729 ) ) ;
#42442 = LINE ( 'NONE', #2290, #26562 ) ;
#42443 = LINE ( 'NONE', #35889, #6064 ) ;
#42444 = DIRECTION ( 'NONE',  ( 0.000000000000000000, 0.000000000000000000, 1.000000000000000000 ) ) ;
#42445 = AXIS2_PLACEMENT_3D ( 'NONE', #9091, #35281, #12600 ) ;
#42446 = VERTEX_POINT ( 'NONE', #26357 ) ;
#42447 = DIRECTION ( 'NONE',  ( -1.000000000000000000, 0.000000000000000000, 0.000000000000000000 ) ) ;
#42448 = AXIS2_PLACEMENT_3D ( 'NONE', #14053, #7037, #23235 ) ;
#42449 = CARTESIAN_POINT ( 'NONE',  ( 9.000000000000001776, -5.871425383721900815, 51.66745943012280406 ) ) ;
#42450 = CIRCLE ( 'NONE', #41043, 120.5010000000000190 ) ;
#42451 = CIRCLE ( 'NONE', #15933, 130.0000000000000000 ) ;
#42452 = EDGE_CURVE ( 'NONE', #2287, #4247, #39831, .T. ) ;
#42454 = ORIENTED_EDGE ( 'NONE', *, *, #19700, .F. ) ;
#42453 = CYLINDRICAL_SURFACE ( 'NONE', #18224, 20.00000000000000355 ) ;
#42455 = VERTEX_POINT ( 'NONE', #42895 ) ;
#42456 = CARTESIAN_POINT ( 'NONE',  ( 17.99999999999999645, 0.000000000000000000, 0.000000000000000000 ) ) ;
#42457 = EDGE_CURVE ( 'NONE', #20175, #33403, #40478, .T. ) ;
#42458 = DIRECTION ( 'NONE',  ( 0.000000000000000000, 0.8747630845319623871, -0.4845508703326481537 ) ) ;
#42459 = CARTESIAN_POINT ( 'NONE',  ( 45.87644943786595064, 40.00000000000000000, 12.37342411884007731 ) ) ;
#42460 = FACE_OUTER_BOUND ( 'NONE', #31213, .T. ) ;
#42461 = EDGE_CURVE ( 'NONE', #6563, #14428, #32983, .T. ) ;
#42462 = DIRECTION ( 'NONE',  ( 0.000000000000000000, 0.000000000000000000, -1.000000000000000000 ) ) ;
#42463 = DIRECTION ( 'NONE',  ( -1.000000000000000000, -0.000000000000000000, -0.000000000000000000 ) ) ;
#42464 = ORIENTED_EDGE ( 'NONE', *, *, #37073, .F. ) ;
#42465 = CARTESIAN_POINT ( 'NONE',  ( 0.000000000000000000, 109.1131968883998695, -26.12628443611929896 ) ) ;
#42466 = ORIENTED_EDGE ( 'NONE', *, *, #23969, .F. ) ;
#42467 = DIRECTION ( 'NONE',  ( 0.000000000000000000, 0.8183027759081662467, 0.5747874102144109321 ) ) ;
#42468 = CARTESIAN_POINT ( 'NONE',  ( 17.99999999999999645, -6.486220790509180212, 112.0098273076987283 ) ) ;
#42469 = CARTESIAN_POINT ( 'NONE',  ( 31.10108666877329853, 31.00000000000000355, 17.95223046116557697 ) ) ;
#42470 = CARTESIAN_POINT ( 'NONE',  ( -3.333333333333335258, 2.694301256218251783, -3.300726591567079815 ) ) ;
#42471 = ORIENTED_EDGE ( 'NONE', *, *, #30393, .F. ) ;
#42472 = ADVANCED_FACE ( 'NONE', ( #6463 ), #10614, .F. ) ;
#42473 = CARTESIAN_POINT ( 'NONE',  ( 18.00000000000000355, 19.44205635905542096, 43.33776004284615624 ) ) ;
#42474 = CARTESIAN_POINT ( 'NONE',  ( -86.71682804797315214, 31.00000000000000711, 23.23408344657299196 ) ) ;
#42475 = VECTOR ( 'NONE', #5536, 1000.000000000000114 ) ;
#42476 = AXIS2_PLACEMENT_3D ( 'NONE', #37019, #13489, #33967 ) ;
#42477 = CIRCLE ( 'NONE', #6950, 120.5010000000000474 ) ;
#42478 = DIRECTION ( 'NONE',  ( 3.996523416598930318E-16, -2.658563593772947863E-15, -1.000000000000000000 ) ) ;
#42479 = ORIENTED_EDGE ( 'NONE', *, *, #19419, .T. ) ;
#42480 = CARTESIAN_POINT ( 'NONE',  ( 16.92944795086299337, 31.00000000000000355, -62.81076020704204410 ) ) ;
#42481 = CARTESIAN_POINT ( 'NONE',  ( -59.29355402628473826, 40.00000000000000000, -20.23837177251483155 ) ) ;
#42482 = CARTESIAN_POINT ( 'NONE',  ( 58.84426737335365232, 40.00000000000000000, 76.69096868241209108 ) ) ;
#42483 = ADVANCED_FACE ( 'NONE', ( #20047 ), #19606, .T. ) ;
#42484 = EDGE_LOOP ( 'NONE', ( #763, #39620, #17299, #32839 ) ) ;
#42485 = SURFACE_STYLE_FILL_AREA ( #9328 ) ;
#42486 = DIRECTION ( 'NONE',  ( 0.000000000000000000, 0.6783118362696173298, -0.7347741508630660778 ) ) ;
#42487 = CARTESIAN_POINT ( 'NONE',  ( 0.000000000000000000, -73.78980555658542073, -95.26571049922065981 ) ) ;
#42489 = VERTEX_POINT ( 'NONE', #36789 ) ;
#42488 = FACE_OUTER_BOUND ( 'NONE', #25846, .T. ) ;
#42490 = DIRECTION ( 'NONE',  ( 1.000000000000000000, -0.000000000000000000, -0.000000000000000000 ) ) ;
#42491 = CARTESIAN_POINT ( 'NONE',  ( 18.00000000000000355, 0.000000000000000000, 0.000000000000000000 ) ) ;
#42492 = ORIENTED_EDGE ( 'NONE', *, *, #9475, .F. ) ;
#42493 = CARTESIAN_POINT ( 'NONE',  ( -63.57631528421845957, 40.00000000000000711, -31.33741679916209222 ) ) ;
#42494 = DIRECTION ( 'NONE',  ( 7.709882115452478166E-16, -1.000000000000000000, -0.000000000000000000 ) ) ;
#42495 = ORIENTED_EDGE ( 'NONE', *, *, #32431, .F. ) ;
#42496 = FACE_OUTER_BOUND ( 'NONE', #41934, .T. ) ;
#42497 = LINE ( 'NONE', #2773, #23868 ) ;
#42498 = ORIENTED_EDGE ( 'NONE', *, *, #34054, .T. ) ;
#42499 = VERTEX_POINT ( 'NONE', #3813 ) ;
#42500 = FACE_OUTER_BOUND ( 'NONE', #29317, .T. ) ;
#42503 = ORIENTED_EDGE ( 'NONE', *, *, #4434, .F. ) ;
#42502 = ADVANCED_FACE ( 'NONE', ( #17199 ), #33084, .F. ) ;
#42501 = CIRCLE ( 'NONE', #37621, 116.0000000000000000 ) ;
#42504 = DIRECTION ( 'NONE',  ( -1.000000000000000000, 0.000000000000000000, -0.000000000000000000 ) ) ;
#42505 = CIRCLE ( 'NONE', #34866, 47.49900000000000944 ) ;
#42506 = FACE_OUTER_BOUND ( 'NONE', #34454, .T. ) ;
#42508 = EDGE_CURVE ( 'NONE', #16661, #34831, #37160, .T. ) ;
#42507 = CIRCLE ( 'NONE', #11184, 13.59999999999999964 ) ;
#42509 = FACE_OUTER_BOUND ( 'NONE', #22017, .T. ) ;
#42510 = AXIS2_PLACEMENT_3D ( 'NONE', #23372, #17276, #3669 ) ;
#42511 = DIRECTION ( 'NONE',  ( -1.000000000000000000, 0.000000000000000000, 0.000000000000000000 ) ) ;
#42512 = ORIENTED_EDGE ( 'NONE', *, *, #24190, .T. ) ;
#42513 = DIRECTION ( 'NONE',  ( 0.000000000000000000, 0.000000000000000000, 1.000000000000000000 ) ) ;
#42514 = ORIENTED_EDGE ( 'NONE', *, *, #15662, .F. ) ;
#42515 = FACE_OUTER_BOUND ( 'NONE', #29376, .T. ) ;
#42516 = ORIENTED_EDGE ( 'NONE', *, *, #32480, .F. ) ;
#42517 = CYLINDRICAL_SURFACE ( 'NONE', #28761, 20.00000000000000355 ) ;
#42518 = CARTESIAN_POINT ( 'NONE',  ( 17.99999999999999645, 34.74871106919766106, -106.6808302961368327 ) ) ;
#42519 = EDGE_CURVE ( 'NONE', #24013, #33535, #32280, .T. ) ;
#42520 = DIRECTION ( 'NONE',  ( 0.000000000000000000, 0.000000000000000000, 1.000000000000000000 ) ) ;
#42521 = CARTESIAN_POINT ( 'NONE',  ( 55.10416666547021691, 31.00000000000000355, 3.599741573803287853 ) ) ;
#42522 = DIRECTION ( 'NONE',  ( 0.000000000000000000, 0.7164567402983164079, -0.6976315211349833900 ) ) ;
#42523 = ORIENTED_EDGE ( 'NONE', *, *, #42207, .T. ) ;
#42524 = CARTESIAN_POINT ( 'NONE',  ( 37.09854380387523776, 31.00000000000000355, 2.490183985263670685 ) ) ;
#42525 = CARTESIAN_POINT ( 'NONE',  ( 43.85342918759069164, 40.00000000000000000, 49.98553323097543455 ) ) ;
#42526 = AXIS2_PLACEMENT_3D ( 'NONE', #13258, #20459, #17189 ) ;
#42527 = EDGE_CURVE ( 'NONE', #42394, #33710, #19084, .T. ) ;
#42528 = VECTOR ( 'NONE', #34362, 1000.000000000000000 ) ;
#42529 = CARTESIAN_POINT ( 'NONE',  ( 17.99999999999999645, -100.8494052988175298, 65.95368414178875582 ) ) ;
#42530 = DIRECTION ( 'NONE',  ( 1.000000000000000000, 0.000000000000000000, 0.000000000000000000 ) ) ;
#42531 = ADVANCED_FACE ( 'NONE', ( #20466 ), #9751, .F. ) ;
#42532 = CIRCLE ( 'NONE', #2148, 47.49900000000000233 ) ;
#42533 = DIRECTION ( 'NONE',  ( 0.000000000000000000, 0.000000000000000000, 1.000000000000000000 ) ) ;
#42534 = LINE ( 'NONE', #19040, #25165 ) ;
#42535 = ORIENTED_EDGE ( 'NONE', *, *, #40675, .F. ) ;
#42536 = CARTESIAN_POINT ( 'NONE',  ( -24.21661388771557100, 40.00000000000000000, 41.94898165618241137 ) ) ;
#42537 = DIRECTION ( 'NONE',  ( 1.000000000000000000, -0.000000000000000000, -0.000000000000000000 ) ) ;
#42538 = DIRECTION ( 'NONE',  ( 1.000000000000000000, 0.000000000000000000, -0.000000000000000000 ) ) ;
#42539 = ORIENTED_EDGE ( 'NONE', *, *, #14566, .F. ) ;
#42540 = CARTESIAN_POINT ( 'NONE',  ( 17.99999999999999645, 114.1529630473454944, -38.59523323561318620 ) ) ;
#42541 = DIRECTION ( 'NONE',  ( -1.000000000000000000, 0.000000000000000000, -0.000000000000000000 ) ) ;
#42542 = AXIS2_PLACEMENT_3D ( 'NONE', #23848, #37113, #30161 ) ;
#42543 = ORIENTED_EDGE ( 'NONE', *, *, #13058, .T. ) ;
#42544 = DIRECTION ( 'NONE',  ( 0.000000000000000000, 0.000000000000000000, 1.000000000000000000 ) ) ;
#42545 = EDGE_LOOP ( 'NONE', ( #2299, #24489 ) ) ;
#42546 = VERTEX_POINT ( 'NONE', #16548 ) ;
#42547 = CYLINDRICAL_SURFACE ( 'NONE', #6263, 47.49900000000000233 ) ;
#42548 = ADVANCED_FACE ( 'NONE', ( #16976 ), #30259, .F. ) ;
#42549 = CARTESIAN_POINT ( 'NONE',  ( 22.12670472278668399, 31.00000000000000355, -82.16725659058067777 ) ) ;
#42550 = ORIENTED_EDGE ( 'NONE', *, *, #14270, .T. ) ;
#42551 = CARTESIAN_POINT ( 'NONE',  ( 0.5999999999999994227, -12.75000000000000000, -1.199999999999999956 ) ) ;
#42552 = EDGE_CURVE ( 'NONE', #32639, #25151, #26768, .T. ) ;
#42553 = ADVANCED_FACE ( 'NONE', ( #36557 ), #6686, .T. ) ;
#42554 = ADVANCED_FACE ( 'NONE', ( #110 ), #24605, .F. ) ;
#42555 = CARTESIAN_POINT ( 'NONE',  ( 17.99999999999999645, -52.88069566989388903, -103.2454939717374032 ) ) ;
#42556 = CIRCLE ( 'NONE', #34198, 58.99999999999999289 ) ;
#42557 = DIRECTION ( 'NONE',  ( 0.000000000000000000, 0.000000000000000000, 1.000000000000000000 ) ) ;
#42558 = ORIENTED_EDGE ( 'NONE', *, *, #10282, .T. ) ;
#42559 = FACE_OUTER_BOUND ( 'NONE', #34511, .T. ) ;
#42560 = DIRECTION ( 'NONE',  ( 1.000000000000000000, 0.000000000000000000, 0.000000000000000000 ) ) ;
#42561 = AXIS2_PLACEMENT_3D ( 'NONE', #12124, #21327, #11259 ) ;
#42562 = CIRCLE ( 'NONE', #34927, 19.19999999999999574 ) ;
#42563 = CARTESIAN_POINT ( 'NONE',  ( 17.99999999999999645, 93.26762629039527042, -76.29967815892260319 ) ) ;
#42565 = DIRECTION ( 'NONE',  ( -1.000000000000000000, 0.000000000000000000, -0.000000000000000000 ) ) ;
#42564 = DIRECTION ( 'NONE',  ( 0.000000000000000000, 0.000000000000000000, 1.000000000000000000 ) ) ;
#42566 = VECTOR ( 'NONE', #32848, 1000.000000000000000 ) ;
#42567 = CARTESIAN_POINT ( 'NONE',  ( 18.00000000000000355, -30.03615769709762517, 42.44795908868979950 ) ) ;
#42568 = EDGE_LOOP ( 'NONE', ( #18513, #29776 ) ) ;
#42569 = SURFACE_STYLE_FILL_AREA ( #13582 ) ;
#42570 = CARTESIAN_POINT ( 'NONE',  ( -27.62299686580952240, 31.00000000000000355, -13.61136854378590577 ) ) ;
#42571 = EDGE_LOOP ( 'NONE', ( #11856, #41924, #41993, #31860 ) ) ;
#42572 = DIRECTION ( 'NONE',  ( 0.000000000000000000, 0.000000000000000000, 1.000000000000000000 ) ) ;
#42573 = DIRECTION ( 'NONE',  ( -1.000000000000000000, 0.000000000000000000, 0.000000000000000000 ) ) ;
#42574 = ORIENTED_EDGE ( 'NONE', *, *, #20, .T. ) ;
#42575 = FACE_OUTER_BOUND ( 'NONE', #34714, .T. ) ;
#42576 = CARTESIAN_POINT ( 'NONE',  ( -27.33276042269523387, 40.00000000000000000, -31.15086293565511966 ) ) ;
#42577 = CARTESIAN_POINT ( 'NONE',  ( 25.29542371717657545, 40.00000000000000000, 28.93716311999360613 ) ) ;
#42578 = EDGE_CURVE ( 'NONE', #2232, #10112, #30888, .T. ) ;
#42579 = CIRCLE ( 'NONE', #33534, 31.49899999999999878 ) ;
#42580 = ORIENTED_EDGE ( 'NONE', *, *, #21126, .T. ) ;
#42581 = ORIENTED_EDGE ( 'NONE', *, *, #326, .T. ) ;
#42582 = CARTESIAN_POINT ( 'NONE',  ( 17.99999999999999645, 64.58410930313661424, -101.7319213743675732 ) ) ;
#42583 = DIRECTION ( 'NONE',  ( 0.000000000000000000, 0.000000000000000000, -1.000000000000000000 ) ) ;
#42584 = CARTESIAN_POINT ( 'NONE',  ( 17.99999999999999645, 0.000000000000000000, 0.000000000000000000 ) ) ;
#42585 = DIRECTION ( 'NONE',  ( 1.000000000000000000, 0.000000000000000000, 0.000000000000000000 ) ) ;
#42586 = DIRECTION ( 'NONE',  ( 1.000000000000000000, -1.373900992973641868E-15, -4.049512215214018063E-16 ) ) ;
#42587 = ORIENTED_EDGE ( 'NONE', *, *, #30133, .F. ) ;
#42588 = DIRECTION ( 'NONE',  ( 0.000000000000000000, 0.000000000000000000, 1.000000000000000000 ) ) ;
#42589 = VERTEX_POINT ( 'NONE', #30696 ) ;
#42590 = CARTESIAN_POINT ( 'NONE',  ( 17.99999999999999645, 28.57802095670086828, 14.28532136906683370 ) ) ;
#42591 = CIRCLE ( 'NONE', #20349, 59.00000000000000711 ) ;
#42592 = CARTESIAN_POINT ( 'NONE',  ( -10.00000000000000000, 0.000000000000000000, 0.000000000000000000 ) ) ;
#42593 = LINE ( 'NONE', #19100, #25662 ) ;
#42594 = AXIS2_PLACEMENT_3D ( 'NONE', #10035, #6767, #22534 ) ;
#42595 = CARTESIAN_POINT ( 'NONE',  ( 2.500000000000000000, 1.178949249685217415, 2.041999999999998483 ) ) ;
#42596 = EDGE_LOOP ( 'NONE', ( #19336, #17565 ) ) ;
#42597 = CYLINDRICAL_SURFACE ( 'NONE', #18745, 13.59999999999999964 ) ;
#42598 = ORIENTED_EDGE ( 'NONE', *, *, #26699, .T. ) ;
#42599 = CYLINDRICAL_SURFACE ( 'NONE', #20066, 1.399999999999998579 ) ;
#42600 = ORIENTED_EDGE ( 'NONE', *, *, #5000, .T. ) ;
#42602 = ORIENTED_EDGE ( 'NONE', *, *, #30147, .F. ) ;
#42601 = CARTESIAN_POINT ( 'NONE',  ( 17.99999999999999645, 0.000000000000000000, 0.000000000000000000 ) ) ;
#42603 = CARTESIAN_POINT ( 'NONE',  ( -47.35250803175854628, 31.00000000000000355, -23.44639516808300073 ) ) ;
#42604 = VERTEX_POINT ( 'NONE', #27868 ) ;
#42605 = DIRECTION ( 'NONE',  ( 0.000000000000000000, 0.000000000000000000, 1.000000000000000000 ) ) ;
#42606 = EDGE_CURVE ( 'NONE', #14728, #33431, #26714, .T. ) ;
#42607 = ADVANCED_FACE ( 'NONE', ( #37858 ), #24826, .T. ) ;
#42608 = VERTEX_POINT ( 'NONE', #41572 ) ;
#42609 = DIRECTION ( 'NONE',  ( 0.000000000000000000, 0.9957341762950349118, -0.09226835946329871307 ) ) ;
#42610 = PRODUCT ( 'spur gear_iso_ISO - Spur gear 2M 34T 20PA 18FW ---S34A75H50L30.0N', 'spur gear_iso_ISO - Spur gear 2M 34T 20PA 18FW ---S34A75H50L30.0N', '', ( #42724 ) ) ;
#42611 = ADVANCED_FACE ( 'NONE', ( #11723 ), #31126, .T. ) ;
#42612 = ORIENTED_EDGE ( 'NONE', *, *, #36375, .F. ) ;
#42613 = CARTESIAN_POINT ( 'NONE',  ( 46.16409756962309530, 40.00000000000000000, -59.99419878592187416 ) ) ;
#42615 = CARTESIAN_POINT ( 'NONE',  ( 17.99999999999999645, 0.000000000000000000, 0.000000000000000000 ) ) ;
#42614 = CARTESIAN_POINT ( 'NONE',  ( 0.000000000000000000, 0.000000000000000000, 0.000000000000000000 ) ) ;
#42616 = LINE ( 'NONE', #32388, #26903 ) ;
#42617 = VERTEX_POINT ( 'NONE', #24171 ) ;
#42618 = CARTESIAN_POINT ( 'NONE',  ( 0.000000000000000000, 29.86146781000101669, -112.0905559814575696 ) ) ;
#42619 = EDGE_LOOP ( 'NONE', ( #22292, #26644, #26917, #11859 ) ) ;
#42620 = CIRCLE ( 'NONE', #17619, 20.00000000000000711 ) ;
#42621 = AXIS2_PLACEMENT_3D ( 'NONE', #23625, #40364, #649 ) ;
#42622 = LINE ( 'NONE', #12773, #19777 ) ;
#42623 = CARTESIAN_POINT ( 'NONE',  ( 0.000000000000000000, -17.08890430202718491, -43.76671000081963570 ) ) ;
#42624 = AXIS2_PLACEMENT_3D ( 'NONE', #17333, #675, #40595 ) ;
#42625 = EDGE_CURVE ( 'NONE', #35323, #35191, #5802, .T. ) ;
#42626 = CARTESIAN_POINT ( 'NONE',  ( 50.46169669344906339, 31.00000000000000355, 57.51940134901310131 ) ) ;
#42628 = CARTESIAN_POINT ( 'NONE',  ( 5.991979999999993645, 2.341154836636396601E-15, -19.11697999999999809 ) ) ;
#42627 = CARTESIAN_POINT ( 'NONE',  ( 0.000000000000000000, 0.000000000000000000, 0.000000000000000000 ) ) ;
#42629 = ORIENTED_EDGE ( 'NONE', *, *, #13223, .F. ) ;
#42630 = VERTEX_POINT ( 'NONE', #24396 ) ;
#42631 = DIRECTION ( 'NONE',  ( 1.000000000000000000, -0.000000000000000000, -0.000000000000000000 ) ) ;
#42632 = CARTESIAN_POINT ( 'NONE',  ( 17.99999999999999645, 3.803237743092368284, -31.26855263151010789 ) ) ;
#42633 = CARTESIAN_POINT ( 'NONE',  ( 58.37089435908782065, 31.00000000000000000, -75.89027429297952665 ) ) ;
#42634 = CARTESIAN_POINT ( 'NONE',  ( -50.38378093996033869, 40.00000000000000711, 87.00968337440519917 ) ) ;
#42635 = LINE ( 'NONE', #16068, #13564 ) ;
#42636 = EDGE_CURVE ( 'NONE', #2648, #5275, #8638, .T. ) ;
#42637 = DIRECTION ( 'NONE',  ( 0.000000000000000000, 0.6736956436465532105, 0.7390089172206627532 ) ) ;
#42638 = VERTEX_POINT ( 'NONE', #4475 ) ;
#42639 = CARTESIAN_POINT ( 'NONE',  ( 18.00000000000000355, 0.000000000000000000, 0.000000000000000000 ) ) ;
#42640 = ORIENTED_EDGE ( 'NONE', *, *, #11798, .F. ) ;
#42641 = CARTESIAN_POINT ( 'NONE',  ( 0.000000000000000000, 0.000000000000000000, 0.000000000000000000 ) ) ;
#42642 = CYLINDRICAL_SURFACE ( 'NONE', #26287, 59.00000000000000000 ) ;
#42643 = FACE_OUTER_BOUND ( 'NONE', #38894, .T. ) ;
#42644 = ORIENTED_EDGE ( 'NONE', *, *, #16008, .F. ) ;
#42645 = CARTESIAN_POINT ( 'NONE',  ( 0.000000000000000000, -19.44205635905570873, 43.33776004284602124 ) ) ;
#42646 = DIRECTION ( 'NONE',  ( 1.000000000000000000, -0.000000000000000000, 0.000000000000000000 ) ) ;
#42647 = CIRCLE ( 'NONE', #7160, 59.00000000000000000 ) ;
#42648 = DIRECTION ( 'NONE',  ( 0.000000000000000000, 0.000000000000000000, 1.000000000000000000 ) ) ;
#42649 = AXIS2_PLACEMENT_3D ( 'NONE', #2181, #42103, #14685 ) ;
#42651 = ORIENTED_EDGE ( 'NONE', *, *, #8199, .T. ) ;
#42650 = DIRECTION ( 'NONE',  ( 0.000000000000000000, -0.6382441836448108363, -0.7698339834299139373 ) ) ;
#42652 = EDGE_CURVE ( 'NONE', #30185, #26654, #3021, .T. ) ;
#42653 = CARTESIAN_POINT ( 'NONE',  ( 12.70938237924789327, 31.00000000000000355, -21.97768283340561979 ) ) ;
#42654 = CARTESIAN_POINT ( 'NONE',  ( 2.100000000000000089, 0.000000000000000000, -0.2800830152838844622 ) ) ;
#42655 = CIRCLE ( 'NONE', #2258, 59.00000000000000000 ) ;
#42656 = B_SPLINE_CURVE_WITH_KNOTS ( 'NONE', 3,
 ( #26404, #13318, #386, #35597, #39672, #40094, #36843, #19071, #9797, #23789, #6951, #36397, #7162, #19870, #20518, #28867, #22344, #32332, #33141, #40969, #4095, #30952, #21403, #11545, #34217, #10896, #31394, #34009, #28128, #11325, #14828, #24656, #41177, #27468, #14391, #20962, #17468, #1036, #7385, #37913, #14174, #37493, #7602, #30540, #13964, #34650, #4311, #24888, #21619, #1478, #40744, #27700, #34426, #24228, #17683, #40528, #27923, #37269, #21176, #24443, #7817, #31182, #11116, #41394, #37698, #38138, #8262, #10663, #3871, #17253, #4772, #820, #24004, #4532, #17906, #14616, #18130, #608, #20742, #1271, #8034, #27258, #30746, #42254, #12615, #32034, #35292, #38771, #9313, #22035, #9107, #8901, #5188, #25930, #8675, #12192, #15900, #5826, #2118, #25516, #5412, #35501, #42469, #15049, #38350, #2539, #25305, #15281, #25731, #22255, #41624, #28569, #2317, #35075, #32449, #28358, #42036, #28776, #5620, #8467, #41835, #18982, #21828, #32236, #18554, #31826, #19184, #15478, #15680, #28987, #38982, #31599, #22459, #29201, #18781, #12408, #35702, #39189, #34868, #1912, #4983, #18338, #11988, #1694, #38553, #11778, #25102, #33520, #13053, #26559, #40267, #16767, #30054, #109, #22667, #19604, #6048, #3171, #29619, #26134, #13476, #12824, #39830, #43116, #9954, #26356, #36141, #23303, #10171, #19400, #19816, #9545, #3604, #16975, #23525, #32667, #325, #26766, #36556, #33310, #30258, #13692, #40037, #6685, #23103, #33083, #16316, #36787, #26994, #16547, #36348, #20046, #35919, #9750, #6897, #3395, #6257, #2744, #39623, #13262, #16109, #20252, #29408, #42675, #39404, #22895, #32873, #2951, #42894, #6462, #29846, #33955, #1212, #14333, #17197, #30482, #4474, #558, #17634, #10612, #27646, #30897, #13913, #31125, #981, #34594, #3812, #24170, #771, #7322, #37434, #14561, #27207, #20687, #24394, #7764, #40477, #24604, #34160, #34375, #4263, #37857, #23947, #4712, #17845, #21342, #27867, #41122, #4039, #20912, #27415, #37213, #7552, #17415, #11273, #30695, #33727, #14126, #18078, #40687, #40915, #10837, #31343, #28078, #7979, #11065, #37643, #21127, #1425, #14778, #10401, #23734, #37001, #7113, #20465, #2065, #31767, #11722, #28727, #28930, #24825, #25679, #4927, #41339, #2480, #42194, #38299, #18287, #21979, #35233, #8844, #12358, #5773, #31551, #15226, #15427, #1863, #9056, #41988, #1640, #5360, #41785, #12138, #15843, #28521, #15624, #25459, #25054, #19130, #11932, #18729, #22407, #38934, #38503, #31984, #25253, #38718, #11492, #22202, #8620, #38083, #35454, #21779, #32187, #5571, #14994, #28301, #18929, #41571, #2267, #8413, #35655, #32396, #5136, #35028, #8210, #21570, #34818, #18496, #16713, #20206, #42835, #33260, #5988, #39346, #43061, #26505, #19344, #9483, #30004, #29565, #26081, #36732, #32819, #39778, #56, #13425, #33030, #16056, #23048, #29358, #42626, #10118, #36506, #39986, #6627, #23254, #22839, #39571, #2903, #12775, #26301, #32614, #19988, #36088, #9264, #22617, #23469, #19552, #3116, #3552, #6851, #29151, #26716, #6205, #9701, #16487, #16268, #12994, #35862, #9905, #2694, #29792, #6415, #13210, #36298, #19766, #3345, #33467, #12565, #42417, #25883, #39142, #21290, #4422, #13867, #23688, #40634, #10782, #27589, #31068, #24557, #36949, #33902, #34117, #20633, #27817, #20863, #7060, #24115, #1155, #4210, #34541, #3992, #34326, #17579, #30427, #37808, #17368, #37383, #41073, #14509, #14076, #7500, #30648, #30852, #16926, #927, #27369, #30209, #14280, #40428, #7713, #40860, #20415, #33677, #11015, #3760, #24344, #17142, #37596, #21077, #23898, #27162, #7927, #716, #17793, #511, #11224, #270, #13642, #26936, #10563, #37162, #40217, #10351, #7272, #31503, #15375, #38247, #4877, #8789, #41513, #8570, #28671, #41939, #28470, #8152, #18443, #21519, #38028, #5083, #21929, #31712, #18675, #28245, #34768, #41734, #12088, #18030, #21726, #18239, #38665, #22148, #25407, #14726, #35406, #31936, #11879, #35181, #5521, #18878, #41291, #11659, #25207, #25002, #4652, #38451, #24772, #1809, #31293, #8363, #34976, #11438 ),
 .UNSPECIFIED., .F., .F.,
 ( 4, 2, 2, 2, 2, 2, 2, 2, 2, 2, 2, 2, 2, 2, 2, 2, 2, 2, 2, 2, 2, 2, 2, 2, 2, 2, 2, 2, 2, 2, 2, 2, 2, 2, 2, 2, 2, 2, 2, 2, 2, 2, 2, 2, 2, 2, 2, 2, 2, 2, 2, 2, 2, 2, 2, 2, 2, 2, 2, 2, 2, 2, 2, 2, 2, 2, 2, 2, 2, 2, 2, 2, 2, 2, 2, 2, 2, 2, 2, 2, 2, 2, 2, 2, 2, 2, 2, 2, 2, 2, 2, 2, 2, 2, 2, 2, 2, 2, 2, 2, 2, 2, 2, 2, 2, 2, 2, 2, 2, 2, 2, 2, 2, 2, 2, 2, 2, 2, 2, 2, 2, 2, 2, 2, 2, 2, 2, 2, 2, 2, 2, 2, 2, 2, 2, 2, 2, 2, 2, 2, 2, 2, 2, 2, 2, 2, 2, 2, 2, 2, 2, 2, 2, 2, 2, 2, 2, 2, 2, 2, 2, 2, 2, 2, 2, 2, 2, 2, 2, 2, 2, 2, 2, 2, 2, 2, 2, 2, 2, 2, 2, 2, 2, 2, 2, 2, 2, 2, 2, 2, 2, 2, 2, 2, 2, 2, 2, 2, 2, 2, 2, 2, 2, 2, 2, 2, 2, 2, 2, 2, 2, 2, 2, 2, 2, 2, 2, 2, 2, 2, 2, 2, 2, 2, 2, 2, 2, 2, 2, 2, 2, 2, 2, 2, 2, 2, 2, 2, 2, 2, 2, 2, 2, 2, 2, 2, 2, 2, 2, 2, 2, 2, 2, 2, 2, 2, 4 ),
 ( 0.000000000000000000, 0.003906250000000000000, 0.007812500000000000000, 0.01171875000000000000, 0.01562500000000000000, 0.01953125000000000000, 0.02343750000000000000, 0.02734375000000000000, 0.03125000000000000000, 0.03515625000000000000, 0.03906250000000000000, 0.04296875000000000000, 0.04687500000000000000, 0.05078125000000000000, 0.05468750000000000000, 0.05859375000000000000, 0.06250000000000000000, 0.06640625000000000000, 0.07031250000000000000, 0.07421875000000000000, 0.07812500000000000000, 0.08203125000000000000, 0.08593750000000000000, 0.08984375000000000000, 0.09375000000000000000, 0.09765625000000000000, 0.1015625000000000000, 0.1054687500000000000, 0.1093750000000000000, 0.1132812500000000000, 0.1171875000000000000, 0.1210937500000000000, 0.1250000000000000000, 0.1289062500000000000, 0.1328125000000000000, 0.1367187500000000000, 0.1406250000000000000, 0.1445312500000000000, 0.1484375000000000000, 0.1523437500000000000, 0.1562500000000000000, 0.1601562500000000000, 0.1640625000000000000, 0.1679687500000000000, 0.1718750000000000000, 0.1757812500000000000, 0.1796875000000000000, 0.1835937500000000000, 0.1875000000000000000, 0.1914062500000000000, 0.1953125000000000000, 0.1992187500000000000, 0.2031250000000000000, 0.2070312500000000000, 0.2109375000000000000, 0.2148437500000000000, 0.2187500000000000000, 0.2226562500000000000, 0.2265625000000000000, 0.2304687500000000000, 0.2343750000000000000, 0.2382812500000000000, 0.2421875000000000000, 0.2460937500000000000, 0.2500000000000000000, 0.2539062500000000000, 0.2578125000000000000, 0.2617187500000000000, 0.2656250000000000000, 0.2695312500000000000, 0.2734375000000000000, 0.2773437500000000000, 0.2812500000000000000, 0.2851562500000000000, 0.2890625000000000000, 0.2929687500000000000, 0.2968750000000000000, 0.3007812500000000000, 0.3046875000000000000, 0.3085937500000000000, 0.3125000000000000000, 0.3164062500000000000, 0.3203125000000000000, 0.3242187500000000000, 0.3281250000000000000, 0.3320312500000000000, 0.3359375000000000000, 0.3398437500000000000, 0.3437500000000000000, 0.3476562500000000000, 0.3515625000000000000, 0.3554687500000000000, 0.3593750000000000000, 0.3632812500000000000, 0.3671875000000000000, 0.3710937500000000000, 0.3750000000000000000, 0.3789062500000000000, 0.3828125000000000000, 0.3867187500000000000, 0.3906250000000000000, 0.3945312500000000000, 0.3984375000000000000, 0.4023437500000000000, 0.4062500000000000000, 0.4101562500000000000, 0.4140625000000000000, 0.4179687500000000000, 0.4218750000000000000, 0.4257812500000000000, 0.4296875000000000000, 0.4335937500000000000, 0.4375000000000000000, 0.4414062500000000000, 0.4453125000000000000, 0.4492187500000000000, 0.4531250000000000000, 0.4570312500000000000, 0.4609375000000000000, 0.4648437500000000000, 0.4687500000000000000, 0.4726562500000000000, 0.4765625000000000000, 0.4804687500000000000, 0.4843750000000000000, 0.4882812500000000000, 0.4921875000000000000, 0.4960937500000000000, 0.5000000000000000000, 0.5039062500000000000, 0.5078125000000000000, 0.5117187500000000000, 0.5156250000000000000, 0.5195312500000000000, 0.5234375000000000000, 0.5273437500000000000, 0.5312500000000000000, 0.5351562500000000000, 0.5390625000000000000, 0.5429687500000000000, 0.5468750000000000000, 0.5507812500000000000, 0.5546875000000000000, 0.5585937500000000000, 0.5625000000000000000, 0.5664062500000000000, 0.5703125000000000000, 0.5742187500000000000, 0.5781250000000000000, 0.5820312500000000000, 0.5859375000000000000, 0.5898437500000000000, 0.5937500000000000000, 0.5976562500000000000, 0.6015625000000000000, 0.6054687500000000000, 0.6093750000000000000, 0.6132812500000000000, 0.6171875000000000000, 0.6210937500000000000, 0.6250000000000000000, 0.6289062500000000000, 0.6328125000000000000, 0.6367187500000000000, 0.6406250000000000000, 0.6445312500000000000, 0.6484375000000000000, 0.6523437500000000000, 0.6562500000000000000, 0.6601562500000000000, 0.6640625000000000000, 0.6679687500000000000, 0.6718750000000000000, 0.6757812500000000000, 0.6796875000000000000, 0.6835937500000000000, 0.6875000000000000000, 0.6914062500000000000, 0.6953125000000000000, 0.6992187500000000000, 0.7031250000000000000, 0.7070312500000000000, 0.7109375000000000000, 0.7148437500000000000, 0.7187500000000000000, 0.7226562500000000000, 0.7265625000000000000, 0.7304687500000000000, 0.7343750000000000000, 0.7382812500000000000, 0.7421875000000000000, 0.7460937500000000000, 0.7500000000000000000, 0.7539062500000000000, 0.7578125000000000000, 0.7617187500000000000, 0.7656250000000000000, 0.7695312500000000000, 0.7734375000000000000, 0.7773437500000000000, 0.7812500000000000000, 0.7851562500000000000, 0.7890625000000000000, 0.7929687500000000000, 0.7968750000000000000, 0.8007812500000000000, 0.8046875000000000000, 0.8085937500000000000, 0.8125000000000000000, 0.8164062500000000000, 0.8203125000000000000, 0.8242187500000000000, 0.8281250000000000000, 0.8320312500000000000, 0.8359375000000000000, 0.8398437500000000000, 0.8437500000000000000, 0.8476562500000000000, 0.8515625000000000000, 0.8554687500000000000, 0.8593750000000000000, 0.8632812500000000000, 0.8671875000000000000, 0.8710937500000000000, 0.8750000000000000000, 0.8789062500000000000, 0.8828125000000000000, 0.8867187500000000000, 0.8906250000000000000, 0.8945312500000000000, 0.8984375000000000000, 0.9023437500000000000, 0.9062500000000000000, 0.9101562500000000000, 0.9140625000000000000, 0.9179687500000000000, 0.9218750000000000000, 0.9257812500000000000, 0.9296875000000000000, 0.9335937500000000000, 0.9375000000000000000, 0.9414062500000000000, 0.9453125000000000000, 0.9492187500000000000, 0.9531250000000000000, 0.9570312500000000000, 0.9609375000000000000, 0.9648437500000000000, 0.9687500000000000000, 0.9726562500000000000, 0.9765625000000000000, 0.9804687500000000000, 0.9843750000000000000, 0.9882812500000000000, 0.9921875000000000000, 0.9960937500000000000, 1.000000000000000000 ),
 .UNSPECIFIED. ) ;
#42657 = EDGE_CURVE ( 'NONE', #32645, #2567, #24002, .T. ) ;
#42659 = ORIENTED_EDGE ( 'NONE', *, *, #32346, .T. ) ;
#42658 = CARTESIAN_POINT ( 'NONE',  ( 17.99999999999999645, -104.0201923570379137, 51.34003878071028026 ) ) ;
#42660 = UNCERTAINTY_MEASURE_WITH_UNIT (LENGTH_MEASURE( 1.000000000000000082E-05 ), #42139, 'distance_accuracy_value', 'NONE');
#42661 = ORIENTED_EDGE ( 'NONE', *, *, #35849, .F. ) ;
#42662 = DIRECTION ( 'NONE',  ( 0.000000000000000000, 0.000000000000000000, 1.000000000000000000 ) ) ;
#42663 = DIRECTION ( 'NONE',  ( 0.000000000000000000, -0.9510565162951500895, -0.3090169943749581649 ) ) ;
#42664 = CARTESIAN_POINT ( 'NONE',  ( -10.41556553088919834, 40.00000000000000000, 38.62046602037417387 ) ) ;
#42665 = CYLINDRICAL_SURFACE ( 'NONE', #20232, 120.5010000000000190 ) ;
#42666 = DIRECTION ( 'NONE',  ( 0.000000000000000000, -0.2486898871648622888, 0.9685831611286290777 ) ) ;
#42667 = DIRECTION ( 'NONE',  ( 1.000000000000000000, -0.000000000000000000, -0.000000000000000000 ) ) ;
#42668 = ORIENTED_EDGE ( 'NONE', *, *, #27910, .F. ) ;
#42669 = LINE ( 'NONE', #12819, #20288 ) ;
#42670 = EDGE_CURVE ( 'NONE', #17165, #17334, #32308, .T. ) ;
#42671 = VERTEX_POINT ( 'NONE', #25057 ) ;
#42672 = FACE_OUTER_BOUND ( 'NONE', #5861, .T. ) ;
#42673 = CARTESIAN_POINT ( 'NONE',  ( 17.99999999999999645, -91.51415974874635140, 64.91094698989267897 ) ) ;
#42674 = EDGE_CURVE ( 'NONE', #41139, #27343, #28163, .T. ) ;
#42675 = CARTESIAN_POINT ( 'NONE',  ( -25.89845354150052259, 31.00000000000000355, -44.83417823681238445 ) ) ;
#42676 = CARTESIAN_POINT ( 'NONE',  ( -16.80298683001097260, 40.00000000000000000, 2.367532924972517439 ) ) ;
#42677 = ORIENTED_EDGE ( 'NONE', *, *, #12106, .T. ) ;
#42678 = LINE ( 'NONE', #15906, #39302 ) ;
#42679 = VECTOR ( 'NONE', #34424, 1000.000000000000000 ) ;
#42680 = CARTESIAN_POINT ( 'NONE',  ( -66.93673649651354651, 31.00000000000000711, 58.72203107584222437 ) ) ;
#42681 = CARTESIAN_POINT ( 'NONE',  ( 17.99999999999999645, -17.77780072541773748, 114.6296200873375284 ) ) ;
#42682 = ORIENTED_EDGE ( 'NONE', *, *, #28951, .T. ) ;
#42683 = CARTESIAN_POINT ( 'NONE',  ( -56.33579487689731735, 31.00000000000000355, -27.88694065509425002 ) ) ;
#42684 = AXIS2_PLACEMENT_3D ( 'NONE', #11097, #1672, #15026 ) ;
#42685 = CARTESIAN_POINT ( 'NONE',  ( -71.90006454724937157, 40.00000000000000711, 4.599370544632132685 ) ) ;
#42686 = CARTESIAN_POINT ( 'NONE',  ( -31.57754862722326905, 40.00000000000000000, 93.01713655900283584 ) ) ;
#42687 = ORIENTED_EDGE ( 'NONE', *, *, #32355, .T. ) ;
#42688 = ADVANCED_FACE ( 'NONE', ( #4713 ), #41124, .F. ) ;
#42689 = CIRCLE ( 'NONE', #21871, 20.00000000000000711 ) ;
#42690 = DIRECTION ( 'NONE',  ( -1.000000000000000000, -0.000000000000000000, -0.000000000000000000 ) ) ;
#42691 = FACE_OUTER_BOUND ( 'NONE', #28820, .T. ) ;
#42692 = DIRECTION ( 'NONE',  ( 1.000000000000000000, -1.058513553088275437E-16, 0.000000000000000000 ) ) ;
#42694 = ORIENTED_EDGE ( 'NONE', *, *, #15690, .F. ) ;
#42693 = DIRECTION ( 'NONE',  ( 1.000000000000000000, -0.000000000000000000, -0.000000000000000000 ) ) ;
#42695 = CYLINDRICAL_SURFACE ( 'NONE', #19136, 59.00000000000000000 ) ;
#42696 = CARTESIAN_POINT ( 'NONE',  ( 4.197393957002303999, 7.772902908466098641E-14, -3.503767560748929810 ) ) ;
#42697 = CARTESIAN_POINT ( 'NONE',  ( 75.10416666583130052, 39.99999999999999289, 4.908738512847474311 ) ) ;
#42698 = DIRECTION ( 'NONE',  ( 0.000000000000000000, 0.000000000000000000, 1.000000000000000000 ) ) ;
#42699 = VERTEX_POINT ( 'NONE', #30898 ) ;
#42700 = DIRECTION ( 'NONE',  ( 0.000000000000000000, 0.000000000000000000, 1.000000000000000000 ) ) ;
#42701 = CARTESIAN_POINT ( 'NONE',  ( 0.000000000000000000, 0.000000000000000000, 0.000000000000000000 ) ) ;
#42702 = CIRCLE ( 'NONE', #26727, 13.59999999999999787 ) ;
#42703 = EDGE_LOOP ( 'NONE', ( #9130, #30902, #24828, #4239 ) ) ;
#42704 = ADVANCED_FACE ( 'NONE', ( #983 ), #14334, .T. ) ;
#42705 = AXIS2_PLACEMENT_3D ( 'NONE', #13689, #20463, #23301 ) ;
#42706 = ORIENTED_EDGE ( 'NONE', *, *, #10628, .T. ) ;
#42707 = DIRECTION ( 'NONE',  ( -1.000000000000000000, -0.000000000000000000, 0.000000000000000000 ) ) ;
#42708 = ORIENTED_EDGE ( 'NONE', *, *, #38446, .T. ) ;
#42709 = FACE_OUTER_BOUND ( 'NONE', #17372, .T. ) ;
#42710 = DIRECTION ( 'NONE',  ( -1.000000000000000000, 0.000000000000000000, -0.000000000000000000 ) ) ;
#42711 = DIRECTION ( 'NONE',  ( -1.000000000000000000, 0.000000000000000000, -0.000000000000000000 ) ) ;
#42712 = CARTESIAN_POINT ( 'NONE',  ( 0.000000000000000000, -63.24564713401724703, -102.5693868539701299 ) ) ;
#42713 = VERTEX_POINT ( 'NONE', #34376 ) ;
#42714 = CARTESIAN_POINT ( 'NONE',  ( 18.00000000000000355, -35.20873326984102647, 31.88259874184018372 ) ) ;
#42715 = EDGE_CURVE ( 'NONE', #30836, #21873, #17847, .T. ) ;
#42716 = VERTEX_POINT ( 'NONE', #41340 ) ;
#42717 = CIRCLE ( 'NONE', #35743, 20.00000000000000711 ) ;
#42718 = LINE ( 'NONE', #12661, #40533 ) ;
#42719 = EDGE_CURVE ( 'NONE', #24437, #36472, #19117, .T. ) ;
#42720 = ORIENTED_EDGE ( 'NONE', *, *, #39551, .F. ) ;
#42721 = DIRECTION ( 'NONE',  ( 1.000000000000000000, 1.836909530733573776E-16, 0.000000000000000000 ) ) ;
#42722 = DIRECTION ( 'NONE',  ( 0.000000000000000000, 0.000000000000000000, 1.000000000000000000 ) ) ;
#42723 = CIRCLE ( 'NONE', #25382, 11.00000000000000000 ) ;
#42724 = PRODUCT_CONTEXT ( 'NONE', #2979, 'mechanical' ) ;
#42725 = DIRECTION ( 'NONE',  ( -3.009274222672345096E-17, -1.000000000000000000, 2.455023325076454960E-18 ) ) ;
#42726 = CARTESIAN_POINT ( 'NONE',  ( -37.49462465745612860, 31.00000000000000355, -48.86220178749748300 ) ) ;
#42727 = DIRECTION ( 'NONE',  ( 1.000000000000000000, 0.000000000000000000, 0.000000000000000000 ) ) ;
#42728 = VERTEX_POINT ( 'NONE', #12359 ) ;
#42729 = CARTESIAN_POINT ( 'NONE',  ( 30.20675218207096790, 31.00000000000000355, 23.25504409023748309 ) ) ;
#42730 = CARTESIAN_POINT ( 'NONE',  ( 64.36038921521112854, 39.99999999999999289, -37.17434371002195803 ) ) ;
#42731 = CIRCLE ( 'NONE', #28833, 116.0000000000000000 ) ;
#42732 = ADVANCED_FACE ( 'NONE', ( #41989 ), #1864, .T. ) ;
#42733 = CARTESIAN_POINT ( 'NONE',  ( 17.99999999999999645, 41.60679253225906393, -108.2814610871942165 ) ) ;
#42734 = FACE_OUTER_BOUND ( 'NONE', #4575, .T. ) ;
#42735 = EDGE_CURVE ( 'NONE', #34842, #16033, #28843, .T. ) ;
#42736 = LINE ( 'NONE', #12681, #4409 ) ;
#42737 = DIRECTION ( 'NONE',  ( 0.000000000000000000, 0.000000000000000000, 1.000000000000000000 ) ) ;
#42738 = PRODUCT_DEFINITION_FORMATION_WITH_SPECIFIED_SOURCE ( 'ANY', '', #5687, .NOT_KNOWN. ) ;
#42739 = VERTEX_POINT ( 'NONE', #12139 ) ;
#42740 = CARTESIAN_POINT ( 'NONE',  ( 30.63689417572177831, 40.00000000000000000, 34.91779699477408627 ) ) ;
#42741 = DIRECTION ( 'NONE',  ( -1.000000000000000000, -0.000000000000000000, -0.000000000000000000 ) ) ;
#42742 = VECTOR ( 'NONE', #36089, 1000.000000000000000 ) ;
#42743 = CARTESIAN_POINT ( 'NONE',  ( 0.000000000000000000, 106.6051926090971023, 45.73109345704855855 ) ) ;
#42744 = ORIENTED_EDGE ( 'NONE', *, *, #8051, .F. ) ;
#42745 = CARTESIAN_POINT ( 'NONE',  ( 0.000000000000000000, 0.000000000000000000, 0.000000000000000000 ) ) ;
#42746 = LINE ( 'NONE', #23176, #4074 ) ;
#42747 = VERTEX_POINT ( 'NONE', #28931 ) ;
#42748 = DIRECTION ( 'NONE',  ( -1.000000000000000000, 0.000000000000000000, 0.000000000000000000 ) ) ;
#42749 = ORIENTED_EDGE ( 'NONE', *, *, #34577, .T. ) ;
#42750 = AXIS2_PLACEMENT_3D ( 'NONE', #25134, #18594, #1949 ) ;
#42751 = EDGE_LOOP ( 'NONE', ( #19468, #37546, #8947, #37120 ) ) ;
#42752 = CIRCLE ( 'NONE', #12168, 59.00000000000000711 ) ;
#42753 = DIRECTION ( 'NONE',  ( 0.000000000000000000, -0.9407002666710364558, 0.3392388661180213427 ) ) ;
#42754 = CARTESIAN_POINT ( 'NONE',  ( -40.08783408682389648, 31.00000000000000355, 81.04563091337925584 ) ) ;
#42755 = ORIENTED_EDGE ( 'NONE', *, *, #31626, .T. ) ;
#42756 = CARTESIAN_POINT ( 'NONE',  ( 17.99999999999999645, -111.8797445107944100, -8.437727291343872338 ) ) ;
#42757 = VECTOR ( 'NONE', #27264, 1000.000000000000000 ) ;
#42758 = CARTESIAN_POINT ( 'NONE',  ( 0.000000000000000000, 34.74871106919766106, -106.6808302961368327 ) ) ;
#42759 = DIRECTION ( 'NONE',  ( -1.000000000000000000, 0.000000000000000000, -0.000000000000000000 ) ) ;
#42760 = ORIENTED_EDGE ( 'NONE', *, *, #26096, .F. ) ;
#42761 = FACE_OUTER_BOUND ( 'NONE', #41496, .T. ) ;
#42762 = EDGE_CURVE ( 'NONE', #39148, #28176, #21926, .T. ) ;
#42763 = AXIS2_PLACEMENT_3D ( 'NONE', #19002, #19625, #25324 ) ;
#42764 = DIRECTION ( 'NONE',  ( 0.000000000000000000, 0.000000000000000000, 1.000000000000000000 ) ) ;
#42765 = EDGE_CURVE ( 'NONE', #4296, #6476, #26745, .T. ) ;
#42767 = DIRECTION ( 'NONE',  ( -1.000000000000000000, 0.000000000000000000, 0.000000000000000000 ) ) ;
#42766 = CARTESIAN_POINT ( 'NONE',  ( -130.0000000000000000, 1.285559651900030663E-13, 1.999999999999930278 ) ) ;
#42768 = CARTESIAN_POINT ( 'NONE',  ( 17.99999999999999645, -111.2721026680459602, -14.38025178762732104 ) ) ;
#42769 = AXIS2_PLACEMENT_3D ( 'NONE', #13808, #27105, #40372 ) ;
#42770 = ORIENTED_EDGE ( 'NONE', *, *, #42928, .T. ) ;
#42772 = AXIS2_PLACEMENT_3D ( 'NONE', #23640, #30160, #215 ) ;
#42771 =( NAMED_UNIT ( * ) SI_UNIT ( $, .STERADIAN. ) SOLID_ANGLE_UNIT ( ) );
#42773 = CARTESIAN_POINT ( 'NONE',  ( -30.10416666442597844, 31.00000000000000355, -1.963495399902747574 ) ) ;
#42774 = CIRCLE ( 'NONE', #32339, 120.5010000000000190 ) ;
#42775 = ORIENTED_EDGE ( 'NONE', *, *, #10143, .T. ) ;
#42776 = DIRECTION ( 'NONE',  ( -1.000000000000000000, 3.469446951953611107E-17, 0.000000000000000000 ) ) ;
#42777 = FACE_OUTER_BOUND ( 'NONE', #27892, .T. ) ;
#42778 = ORIENTED_EDGE ( 'NONE', *, *, #8666, .T. ) ;
#42779 = CARTESIAN_POINT ( 'NONE',  ( 0.000000000000000000, 0.000000000000000000, 0.000000000000000000 ) ) ;
#42780 = CARTESIAN_POINT ( 'NONE',  ( 34.94781834021004840, 40.00000000000000000, -26.81980329959834108 ) ) ;
#42781 = CIRCLE ( 'NONE', #21964, 120.5010000000000332 ) ;
#42782 = CARTESIAN_POINT ( 'NONE',  ( 19.31996883371318674, 40.00000000000000000, 33.58758284028577634 ) ) ;
#42783 = VECTOR ( 'NONE', #15724, 1000.000000000000000 ) ;
#42784 = ORIENTED_EDGE ( 'NONE', *, *, #38942, .T. ) ;
#42785 = EDGE_CURVE ( 'NONE', #39524, #17179, #18497, .T. ) ;
#42786 = ORIENTED_EDGE ( 'NONE', *, *, #16669, .F. ) ;
#42787 = CARTESIAN_POINT ( 'NONE',  ( 1.039096088315723056E-14, -6.912265343809663812E-14, -26.00000000000000355 ) ) ;
#42788 = AXIS2_PLACEMENT_3D ( 'NONE', #25398, #38654, #16869 ) ;
#42789 = CARTESIAN_POINT ( 'NONE',  ( -10.00000000000000000, 0.000000000000000000, 0.000000000000000000 ) ) ;
#42790 = EDGE_CURVE ( 'NONE', #6132, #24356, #38719, .T. ) ;
#42791 = EDGE_CURVE ( 'NONE', #1326, #40885, #924, .T. ) ;
#42792 = EDGE_CURVE ( 'NONE', #36577, #13563, #31986, .T. ) ;
#42793 = AXIS2_PLACEMENT_3D ( 'NONE', #20468, #13479, #30487 ) ;
#42794 = DIRECTION ( 'NONE',  ( -1.000000000000000000, 0.000000000000000000, 0.000000000000000000 ) ) ;
#42795 = LINE ( 'NONE', #22576, #30141 ) ;
#42796 = DIRECTION ( 'NONE',  ( -1.000000000000000000, -0.000000000000000000, -0.000000000000000000 ) ) ;
#42797 = CIRCLE ( 'NONE', #275, 116.0000000000000000 ) ;
#42798 = ORIENTED_EDGE ( 'NONE', *, *, #10056, .F. ) ;
#42799 = CARTESIAN_POINT ( 'NONE',  ( -10.00000000000000000, 0.000000000000000000, 0.000000000000000000 ) ) ;
#42800 = ORIENTED_EDGE ( 'NONE', *, *, #23857, .T. ) ;
#42801 = CARTESIAN_POINT ( 'NONE',  ( 17.99999999999999645, -119.8996782608629275, -12.02323392193477325 ) ) ;
#42802 = DIRECTION ( 'NONE',  ( 0.000000000000000000, 0.000000000000000000, 1.000000000000000000 ) ) ;
#42803 = DIRECTION ( 'NONE',  ( 0.000000000000000000, 0.000000000000000000, 1.000000000000000000 ) ) ;
#42804 = DIRECTION ( 'NONE',  ( 0.000000000000000000, 0.6783118362696124448, 0.7347741508630706297 ) ) ;
#42805 = ORIENTED_EDGE ( 'NONE', *, *, #23938, .T. ) ;
#42806 = DIRECTION ( 'NONE',  ( -1.000000000000000000, -0.000000000000000000, -0.000000000000000000 ) ) ;
#42807 = ORIENTED_EDGE ( 'NONE', *, *, #20014, .F. ) ;
#42808 = LINE ( 'NONE', #39686, #4757 ) ;
#42809 = CARTESIAN_POINT ( 'NONE',  ( 0.000000000000000000, 59.47573314508867526, -99.59235496188547643 ) ) ;
#42810 = AXIS2_PLACEMENT_3D ( 'NONE', #40633, #10781, #36730 ) ;
#42811 = VERTEX_POINT ( 'NONE', #5572 ) ;
#42813 = VERTEX_POINT ( 'NONE', #11933 ) ;
#42812 = DIRECTION ( 'NONE',  ( -1.000000000000000000, 1.373900992973641868E-15, 3.469446951953632924E-16 ) ) ;
#42814 = CARTESIAN_POINT ( 'NONE',  ( 41.67488199336423804, 31.00000000000000355, 54.49293397273885375 ) ) ;
#42815 = ORIENTED_EDGE ( 'NONE', *, *, #21746, .F. ) ;
#42816 = CARTESIAN_POINT ( 'NONE',  ( 0.000000000000000000, 78.75547124681369837, 91.20343606297029737 ) ) ;
#42817 = VECTOR ( 'NONE', #20560, 1000.000000000000000 ) ;
#42818 = ORIENTED_EDGE ( 'NONE', *, *, #20357, .T. ) ;
#42819 = CARTESIAN_POINT ( 'NONE',  ( 18.00000000000000355, 17.50309955389612426, 43.60271849949370448 ) ) ;
#42820 = AXIS2_PLACEMENT_3D ( 'NONE', #24219, #33773, #20952 ) ;
#42821 = EDGE_CURVE ( 'NONE', #43048, #41169, #5834, .T. ) ;
#42822 = ORIENTED_EDGE ( 'NONE', *, *, #33624, .F. ) ;
#42823 = CARTESIAN_POINT ( 'NONE',  ( 37.87019299813560025, 40.00000000000000000, -76.55254356380190472 ) ) ;
#42825 = CARTESIAN_POINT ( 'NONE',  ( 18.00000000000000355, -24.47917365149913849, -45.87777302070959706 ) ) ;
#42824 = LINE ( 'NONE', #9473, #21068 ) ;
#42826 = CIRCLE ( 'NONE', #31715, 120.5010000000000190 ) ;
#42827 = DIRECTION ( 'NONE',  ( 0.000000000000000000, -0.1253332335643113082, 0.9921147013144769877 ) ) ;
#42828 = VERTEX_POINT ( 'NONE', #21780 ) ;
#42829 = CARTESIAN_POINT ( 'NONE',  ( 9.000000000000001776, 17.77780072541695944, 114.6296200873376563 ) ) ;
#42830 = EDGE_LOOP ( 'NONE', ( #20099, #25728, #19134, #35429 ) ) ;
#42831 = SURFACE_STYLE_FILL_AREA ( #3342 ) ;
#42832 = AXIS2_PLACEMENT_3D ( 'NONE', #12161, #8870, #37183 ) ;
#42833 = DIRECTION ( 'NONE',  ( 0.000000000000000000, 0.000000000000000000, 1.000000000000000000 ) ) ;
#42834 = DIRECTION ( 'NONE',  ( 1.000000000000000000, 0.000000000000000000, 0.000000000000000000 ) ) ;
#42835 = CARTESIAN_POINT ( 'NONE',  ( 32.44529481510334534, 31.00000000000000355, -65.82339768528792945 ) ) ;
#42837 = LINE ( 'NONE', #5776, #9508 ) ;
#42836 = CYLINDRICAL_SURFACE ( 'NONE', #17749, 20.00000000000000355 ) ;
#42838 = ORIENTED_EDGE ( 'NONE', *, *, #32913, .F. ) ;
#42839 = DIRECTION ( 'NONE',  ( 0.000000000000000000, -0.6845471059286791782, -0.7289686274214204342 ) ) ;
#42840 = EDGE_CURVE ( 'NONE', #42205, #8016, #39254, .T. ) ;
#42841 = ORIENTED_EDGE ( 'NONE', *, *, #28768, .T. ) ;
#42842 = CARTESIAN_POINT ( 'NONE',  ( 21.00000000000000355, 2.516649172247811061E-16, -2.055000000000000160 ) ) ;
#42843 = DIRECTION ( 'NONE',  ( 0.000000000000000000, 0.4132121857683728194, 0.9106347728549155640 ) ) ;
#42844 = ADVANCED_FACE ( 'NONE', ( #5775 ), #32397, .T. ) ;
#42846 = CARTESIAN_POINT ( 'NONE',  ( -87.75478321338633236, 31.00000000000000711, -29.92102470462889130 ) ) ;
#42845 = AXIS2_PLACEMENT_3D ( 'NONE', #1854, #12128, #18071 ) ;
#42847 = CARTESIAN_POINT ( 'NONE',  ( 24.72345498302142630, 40.00000000000000000, -91.84610802670698604 ) ) ;
#42848 = EDGE_CURVE ( 'NONE', #821, #36952, #30234, .T. ) ;
#42849 = ADVANCED_FACE ( 'NONE', ( #19345, #25884 ), #39143, .T. ) ;
#42850 = DIRECTION ( 'NONE',  ( 0.000000000000000000, 0.8993121301712172500, 0.4373073204588593388 ) ) ;
#42851 = CIRCLE ( 'NONE', #24097, 120.5010000000000474 ) ;
#42852 = CIRCLE ( 'NONE', #12930, 58.99999999999999289 ) ;
#42853 = ADVANCED_FACE ( 'NONE', ( #35863 ), #32615, .F. ) ;
#42854 = DIRECTION ( 'NONE',  ( -1.000000000000000000, -0.000000000000000000, -0.000000000000000000 ) ) ;
#42855 = VERTEX_POINT ( 'NONE', #21980 ) ;
#42856 = DIRECTION ( 'NONE',  ( 0.000000000000000000, 0.000000000000000000, 1.000000000000000000 ) ) ;
#42857 = ORIENTED_EDGE ( 'NONE', *, *, #34446, .F. ) ;
#42858 = CARTESIAN_POINT ( 'NONE',  ( -101.6738636939643357, 39.99999999999999289, -5.192942712545352890 ) ) ;
#42859 = AXIS2_PLACEMENT_3D ( 'NONE', #38316, #15014, #1879 ) ;
#42860 = AXIS2_PLACEMENT_3D ( 'NONE', #769, #20464, #20911 ) ;
#42861 =( GEOMETRIC_REPRESENTATION_CONTEXT ( 3 ) GLOBAL_UNCERTAINTY_ASSIGNED_CONTEXT ( ( #24378 ) ) GLOBAL_UNIT_ASSIGNED_CONTEXT ( ( #17378, #13438, #27170 ) ) REPRESENTATION_CONTEXT ( 'NONE', 'WORKASPACE' ) );
#42862 = DIRECTION ( 'NONE',  ( -1.000000000000000000, 0.000000000000000000, 0.000000000000000000 ) ) ;
#42863 = ADVANCED_FACE ( 'NONE', ( #15227 ), #8621, .F. ) ;
#42864 = LINE ( 'NONE', #10583, #26148 ) ;
#42865 = ORIENTED_EDGE ( 'NONE', *, *, #10059, .F. ) ;
#42866 = FACE_BOUND ( 'NONE', #14101, .T. ) ;
#42867 = CARTESIAN_POINT ( 'NONE',  ( -2.649999999999776090, -150.5000000000013642, 9.999999999999587885 ) ) ;
#42868 = AXIS2_PLACEMENT_3D ( 'NONE', #22172, #32365, #15813 ) ;
#42869 = CARTESIAN_POINT ( 'NONE',  ( 8.999999999999998224, 74.56001736500738275, -88.86396238368959644 ) ) ;
#42871 = EDGE_LOOP ( 'NONE', ( #31791, #34412, #9869, #25645, #38929, #2046, #42251, #13167, #34597, #40656, #6771, #11981, #346, #26987, #15829, #40078, #21362, #7717, #33950, #24088, #17873, #41332, #27439, #5574, #38737, #41798 ) ) ;
#42870 = DIRECTION ( 'NONE',  ( -1.000000000000000000, -0.000000000000000000, -0.000000000000000000 ) ) ;
#42872 = CARTESIAN_POINT ( 'NONE',  ( -10.52919346384764054, 31.00000000000000355, -21.36894910329525032 ) ) ;
#42873 = CARTESIAN_POINT ( 'NONE',  ( 2.650000000000181988, -150.5000000000013642, 9.999999999999584332 ) ) ;
#42875 = ORIENTED_EDGE ( 'NONE', *, *, #10832, .F. ) ;
#42874 = DIRECTION ( 'NONE',  ( 0.000000000000000000, 0.000000000000000000, 1.000000000000000000 ) ) ;
#42876 = EDGE_LOOP ( 'NONE', ( #9977, #27663, #17166, #23305 ) ) ;
#42877 = CARTESIAN_POINT ( 'NONE',  ( 0.000000000000000000, 104.6166166098452379, -50.11350645393572023 ) ) ;
#42878 = CYLINDRICAL_SURFACE ( 'NONE', #18286, 116.0000000000000000 ) ;
#42879 = CARTESIAN_POINT ( 'NONE',  ( -20.27214883179920690, 40.00000000000000000, 34.96734655410256210 ) ) ;
#42880 = CARTESIAN_POINT ( 'NONE',  ( -81.46080130434573618, -35.35525454449571470, 14.45886780445633946 ) ) ;
#42881 = CIRCLE ( 'NONE', #24124, 2.000000000000000888 ) ;
#42882 = FACE_OUTER_BOUND ( 'NONE', #2921, .T. ) ;
#42883 = AXIS2_PLACEMENT_3D ( 'NONE', #1457, #17886, #1675 ) ;
#42884 = CARTESIAN_POINT ( 'NONE',  ( 17.99999999999999645, -104.2166695095708491, -60.49278301857915352 ) ) ;
#42886 = ORIENTED_EDGE ( 'NONE', *, *, #12665, .F. ) ;
#42885 = AXIS2_PLACEMENT_3D ( 'NONE', #14383, #37483, #1470 ) ;
#42887 = EDGE_CURVE ( 'NONE', #24669, #959, #15429, .T. ) ;
#42888 = DIRECTION ( 'NONE',  ( 0.000000000000000000, 0.000000000000000000, 1.000000000000000000 ) ) ;
#42889 = VERTEX_POINT ( 'NONE', #876 ) ;
#42890 = AXIS2_PLACEMENT_3D ( 'NONE', #18873, #28026, #28466 ) ;
#42891 = CARTESIAN_POINT ( 'NONE',  ( 0.000000000000000000, 0.000000000000000000, 0.000000000000000000 ) ) ;
#42892 = LINE ( 'NONE', #36347, #12936 ) ;
#42893 = AXIS2_PLACEMENT_3D ( 'NONE', #28299, #7978, #21341 ) ;
#42894 = CARTESIAN_POINT ( 'NONE',  ( -3.436116956419240864, 31.00000000000000355, -52.39583333462812931 ) ) ;
#42895 = CARTESIAN_POINT ( 'NONE',  ( 0.000000000000000000, -83.49789599728840983, 86.88263557826738293 ) ) ;
#42897 = ORIENTED_EDGE ( 'NONE', *, *, #12030, .F. ) ;
#42896 = VECTOR ( 'NONE', #41302, 1000.000000000000000 ) ;
#42898 = CIRCLE ( 'NONE', #24135, 59.00000000000000000 ) ;
#42900 = CIRCLE ( 'NONE', #13013, 13.60000000000000320 ) ;
#42899 = CARTESIAN_POINT ( 'NONE',  ( 17.99999999999999645, 0.000000000000000000, 0.000000000000000000 ) ) ;
#42901 = CARTESIAN_POINT ( 'NONE',  ( -89.62817255407412631, 31.00000000000000711, -11.80141054548196422 ) ) ;
#42902 = DIRECTION ( 'NONE',  ( 3.996523416598930318E-16, -2.658563593772947863E-15, -1.000000000000000000 ) ) ;
#42903 = VERTEX_POINT ( 'NONE', #26082 ) ;
#42904 = CARTESIAN_POINT ( 'NONE',  ( -22.66037885604483648, 31.00000000000000355, 66.40833514169634100 ) ) ;
#42905 = CARTESIAN_POINT ( 'NONE',  ( 8.965261019434027645, 40.00000000000000000, 68.85524230650666766 ) ) ;
#42906 = ADVANCED_FACE ( 'NONE', ( #9484 ), #36507, .F. ) ;
#42907 = ADVANCED_FACE ( 'NONE', ( #30005 ), #40804, .F. ) ;
#42908 = DIRECTION ( 'NONE',  ( -0.000000000000000000, -0.000000000000000000, 1.000000000000000000 ) ) ;
#42909 = ADVANCED_FACE ( 'NONE', ( #39348 ), #26506, .F. ) ;
#42910 = EDGE_LOOP ( 'NONE', ( #15737, #37970, #5398, #38860 ) ) ;
#42911 = CARTESIAN_POINT ( 'NONE',  ( 0.1756481739660539498, -4.720212674038995360, -3.469390959564070620 ) ) ;
#42912 = CARTESIAN_POINT ( 'NONE',  ( 17.99999999999999645, -82.63181128086679905, -81.41243003647058174 ) ) ;
#42913 = DIRECTION ( 'NONE',  ( 0.000000000000000000, -6.586068790149233915E-15, 1.000000000000000000 ) ) ;
#42914 = AXIS2_PLACEMENT_3D ( 'NONE', #13105, #38878, #162 ) ;
#42916 = ORIENTED_EDGE ( 'NONE', *, *, #18395, .F. ) ;
#42915 = DIRECTION ( 'NONE',  ( 0.000000000000000000, 0.000000000000000000, 1.000000000000000000 ) ) ;
#42917 = CIRCLE ( 'NONE', #13002, 120.5010000000000332 ) ;
#42918 = FACE_OUTER_BOUND ( 'NONE', #12236, .T. ) ;
#42920 = ORIENTED_EDGE ( 'NONE', *, *, #11109, .F. ) ;
#42919 = VECTOR ( 'NONE', #42667, 1000.000000000000000 ) ;
#42921 = CARTESIAN_POINT ( 'NONE',  ( 6.999999999999985789, 19.60000000000008313, 0.000000000000000000 ) ) ;
#42922 = ADVANCED_FACE ( 'NONE', ( #30801 ), #13426, .T. ) ;
#42923 = CIRCLE ( 'NONE', #21415, 116.0000000000000000 ) ;
#42924 = CARTESIAN_POINT ( 'NONE',  ( -51.96644965832453522, 40.00000000000000711, 59.25555446698126616 ) ) ;
#42925 = LINE ( 'NONE', #3200, #1286 ) ;
#42926 = AXIS2_PLACEMENT_3D ( 'NONE', #18887, #34986, #38896 ) ;
#42927 = ORIENTED_EDGE ( 'NONE', *, *, #12507, .T. ) ;
#42928 = EDGE_CURVE ( 'NONE', #2980, #37365, #3713, .T. ) ;
#42929 = CARTESIAN_POINT ( 'NONE',  ( -139.5000000000000000, 1.517807346132285267E-13, 9.999999999999946709 ) ) ;
#42930 = CARTESIAN_POINT ( 'NONE',  ( 17.99999999999999645, 18.35539002514383711, 110.6858262410710410 ) ) ;
#42931 = VECTOR ( 'NONE', #33332, 1000.000000000000000 ) ;
#42932 = ORIENTED_EDGE ( 'NONE', *, *, #25200, .F. ) ;
#42933 = AXIS2_PLACEMENT_3D ( 'NONE', #14158, #3428, #27447 ) ;
#42934 = ORIENTED_EDGE ( 'NONE', *, *, #28659, .T. ) ;
#42935 = CYLINDRICAL_SURFACE ( 'NONE', #9325, 120.5010000000000190 ) ;
#42936 = EDGE_LOOP ( 'NONE', ( #15941, #7505, #38938, #6292 ) ) ;
#42937 = DIRECTION ( 'NONE',  ( -1.000000000000000000, 0.000000000000000000, -0.000000000000000000 ) ) ;
#42938 = DIRECTION ( 'NONE',  ( -1.000000000000000000, -0.000000000000000000, -0.000000000000000000 ) ) ;
#42939 = CIRCLE ( 'NONE', #21435, 120.5010000000000190 ) ;
#42940 = DIRECTION ( 'NONE',  ( 0.000000000000000000, 0.000000000000000000, 1.000000000000000000 ) ) ;
#42941 = CARTESIAN_POINT ( 'NONE',  ( 0.000000000000000000, 25.46650492921896713, 19.29328419707794495 ) ) ;
#42942 = EDGE_LOOP ( 'NONE', ( #27332, #15202, #21386, #25886 ) ) ;
#42943 = DIRECTION ( 'NONE',  ( -1.000000000000000000, -0.000000000000000000, -0.000000000000000000 ) ) ;
#42944 = ORIENTED_EDGE ( 'NONE', *, *, #1489, .T. ) ;
#42945 = CARTESIAN_POINT ( 'NONE',  ( 17.99999999999999645, 0.000000000000000000, 0.000000000000000000 ) ) ;
#42947 = ORIENTED_EDGE ( 'NONE', *, *, #34598, .T. ) ;
#42946 = AXIS2_PLACEMENT_3D ( 'NONE', #22861, #9723, #42439 ) ;
#42948 = LINE ( 'NONE', #18825, #18353 ) ;
#42949 = DIRECTION ( 'NONE',  ( 0.000000000000000000, 0.000000000000000000, 1.000000000000000000 ) ) ;
#42950 = CIRCLE ( 'NONE', #7432, 58.99999999999999289 ) ;
#42951 = DIRECTION ( 'NONE',  ( -1.000000000000000000, -0.000000000000000000, -0.000000000000000000 ) ) ;
#42952 = CARTESIAN_POINT ( 'NONE',  ( -46.07128526072433772, 31.00000000000000355, -40.40198152342698990 ) ) ;
#42953 = ORIENTED_EDGE ( 'NONE', *, *, #14157, .T. ) ;
#42955 = CARTESIAN_POINT ( 'NONE',  ( -29.39530816626169241, 31.00000000000000355, -14.54745122861254814 ) ) ;
#42954 = AXIS2_PLACEMENT_3D ( 'NONE', #22859, #29172, #2502 ) ;
#42956 = EDGE_CURVE ( 'NONE', #5150, #17494, #27531, .T. ) ;
#42957 = CARTESIAN_POINT ( 'NONE',  ( 40.54457361686378647, 40.00000000000000000, 52.83773991529862712 ) ) ;
#42958 = EDGE_CURVE ( 'NONE', #17989, #20730, #37875, .T. ) ;
#42959 = VECTOR ( 'NONE', #35446, 1000.000000000000000 ) ;
#42960 = DIRECTION ( 'NONE',  ( 0.000000000000000000, 0.6382441836448211614, -0.7698339834299053885 ) ) ;
#42961 = CARTESIAN_POINT ( 'NONE',  ( 17.99999999999999645, 0.000000000000000000, 0.000000000000000000 ) ) ;
#42962 = DIRECTION ( 'NONE',  ( -1.000000000000000000, -0.000000000000000000, -0.000000000000000000 ) ) ;
#42963 = EDGE_CURVE ( 'NONE', #10641, #24221, #11435, .T. ) ;
#42964 = PRODUCT_DEFINITION_SHAPE ( 'NONE', 'NONE',  #43190 ) ;
#42965 = ORIENTED_EDGE ( 'NONE', *, *, #9832, .F. ) ;
#42966 = CARTESIAN_POINT ( 'NONE',  ( -5.542584477697039880, 40.00000000000000000, -42.01772079774592328 ) ) ;
#42967 = DIRECTION ( 'NONE',  ( 0.000000000000000000, 0.000000000000000000, 1.000000000000000000 ) ) ;
#42968 = DIRECTION ( 'NONE',  ( -1.000000000000000000, -0.000000000000000000, -0.000000000000000000 ) ) ;
#42969 = VERTEX_POINT ( 'NONE', #13212 ) ;
#42970 = ADVANCED_FACE ( 'NONE', ( #36734 ), #35767, .T. ) ;
#42971 = AXIS2_PLACEMENT_3D ( 'NONE', #41090, #18467, #1178 ) ;
#42972 = DIRECTION ( 'NONE',  ( 0.000000000000000000, 0.000000000000000000, 1.000000000000000000 ) ) ;
#42973 = DIRECTION ( 'NONE',  ( 0.000000000000000000, 0.000000000000000000, 1.000000000000000000 ) ) ;
#42974 = ADVANCED_FACE ( 'NONE', ( #1099 ), #32820, .F. ) ;
#42975 = VERTEX_POINT ( 'NONE', #4368 ) ;
#42976 = DIRECTION ( 'NONE',  ( -1.000000000000000000, 0.000000000000000000, -0.000000000000000000 ) ) ;
#42977 = EDGE_LOOP ( 'NONE', ( #38918, #11148, #10450, #24806 ) ) ;
#42978 = VECTOR ( 'NONE', #28196, 1000.000000000000000 ) ;
#42979 = CIRCLE ( 'NONE', #502, 36.00000000000000000 ) ;
#42980 = ORIENTED_EDGE ( 'NONE', *, *, #9121, .T. ) ;
#42981 = AXIS2_PLACEMENT_3D ( 'NONE', #25696, #38516, #42003 ) ;
#42982 = DIRECTION ( 'NONE',  ( 0.000000000000000000, 0.000000000000000000, 1.000000000000000000 ) ) ;
#42983 = CARTESIAN_POINT ( 'NONE',  ( -72.38966680861454961, 31.00000000000000711, 55.38960906678870089 ) ) ;
#42984 = ORIENTED_EDGE ( 'NONE', *, *, #22643, .T. ) ;
#42985 = CYLINDRICAL_SURFACE ( 'NONE', #26590, 120.5010000000000190 ) ;
#42986 = CIRCLE ( 'NONE', #18689, 13.59999999999999787 ) ;
#42987 = DIRECTION ( 'NONE',  ( -1.000000000000000000, -0.000000000000000000, -0.000000000000000000 ) ) ;
#42988 = CARTESIAN_POINT ( 'NONE',  ( 0.000000000000000000, -24.47917365149977087, 45.87777302070925600 ) ) ;
#42989 = ORIENTED_EDGE ( 'NONE', *, *, #7898, .T. ) ;
#42990 = EDGE_CURVE ( 'NONE', #37365, #3752, #17740, .T. ) ;
#42991 = DIRECTION ( 'NONE',  ( 0.000000000000000000, 0.000000000000000000, 1.000000000000000000 ) ) ;
#42992 = EDGE_CURVE ( 'NONE', #15086, #32065, #6207, .T. ) ;
#42993 = CARTESIAN_POINT ( 'NONE',  ( -10.00000000000000000, 0.000000000000000000, 0.000000000000000000 ) ) ;
#42994 = ADVANCED_FACE ( 'NONE', ( #16269 ), #42836, .T. ) ;
#42996 = FACE_OUTER_BOUND ( 'NONE', #9823, .T. ) ;
#42995 = FACE_OUTER_BOUND ( 'NONE', #21690, .T. ) ;
#42997 = CARTESIAN_POINT ( 'NONE',  ( 17.99999999999999645, 0.000000000000000000, 0.000000000000000000 ) ) ;
#42998 = ORIENTED_EDGE ( 'NONE', *, *, #21007, .F. ) ;
#42999 = SURFACE_SIDE_STYLE ('',( #33413 ) ) ;
#43000 = CARTESIAN_POINT ( 'NONE',  ( 20.45440555730427690, 31.00000000000000355, -26.67302265141799467 ) ) ;
#43001 = VERTEX_POINT ( 'NONE', #36299 ) ;
#43002 = CARTESIAN_POINT ( 'NONE',  ( 17.99999999999999645, -112.8457601792517124, 26.86697618949339272 ) ) ;
#43003 = CARTESIAN_POINT ( 'NONE',  ( -8.749793197483594298, -2.055254544495723756, 2.972870684497274762 ) ) ;
#43004 = CIRCLE ( 'NONE', #20776, 13.59999999999999964 ) ;
#43005 = ORIENTED_EDGE ( 'NONE', *, *, #1747, .F. ) ;
#43006 = CARTESIAN_POINT ( 'NONE',  ( -22.99999999999998579, -5.613287575611360052E-14, -26.00000000000001421 ) ) ;
#43007 = CARTESIAN_POINT ( 'NONE',  ( 11.12085686420672381, 40.00000000000000000, -41.54537790535560760 ) ) ;
#43008 = AXIS2_PLACEMENT_3D ( 'NONE', #13332, #16173, #33157 ) ;
#43009 = EDGE_CURVE ( 'NONE', #25806, #40745, #26774, .T. ) ;
#43010 = CARTESIAN_POINT ( 'NONE',  ( -38.36856355434107968, 40.00000000000000000, 33.53830235993100217 ) ) ;
#43011 = AXIS2_PLACEMENT_3D ( 'NONE', #35325, #38172, #14860 ) ;
#43012 = AXIS2_PLACEMENT_3D ( 'NONE', #41932, #15158, #15784 ) ;
#43013 = AXIS2_PLACEMENT_3D ( 'NONE', #6224, #3133, #32840 ) ;
#43014 = ORIENTED_EDGE ( 'NONE', *, *, #37167, .F. ) ;
#43015 = ORIENTED_EDGE ( 'NONE', *, *, #26800, .T. ) ;
#43016 = FACE_OUTER_BOUND ( 'NONE', #22436, .T. ) ;
#43017 = DIRECTION ( 'NONE',  ( -0.000000000000000000, -0.000000000000000000, -1.000000000000000000 ) ) ;
#43018 = AXIS2_PLACEMENT_3D ( 'NONE', #41308, #24789, #14527 ) ;
#43019 = FACE_OUTER_BOUND ( 'NONE', #24332, .T. ) ;
#43020 = DIRECTION ( 'NONE',  ( -1.000000000000000000, 0.000000000000000000, 0.000000000000000000 ) ) ;
#43021 = EDGE_CURVE ( 'NONE', #31572, #5899, #16488, .T. ) ;
#43022 = DIRECTION ( 'NONE',  ( 1.000000000000000000, 0.000000000000000000, 0.000000000000000000 ) ) ;
#43023 = ORIENTED_EDGE ( 'NONE', *, *, #43033, .T. ) ;
#43024 = CARTESIAN_POINT ( 'NONE',  ( 18.00000000000000355, -9.744342220503709129, 46.48873837489794880 ) ) ;
#43025 = ORIENTED_EDGE ( 'NONE', *, *, #33213, .T. ) ;
#43026 = LINE ( 'NONE', #39740, #13217 ) ;
#43027 = CARTESIAN_POINT ( 'NONE',  ( 0.000000000000000000, 0.000000000000000000, 3.469446951953614189E-15 ) ) ;
#43028 = AXIS2_PLACEMENT_3D ( 'NONE', #36338, #2943, #42462 ) ;
#43029 = EDGE_LOOP ( 'NONE', ( #2936, #16640, #12145 ) ) ;
#43030 = ADVANCED_FACE ( 'NONE', ( #21233 ), #31658, .F. ) ;
#43031 = DIRECTION ( 'NONE',  ( 1.000000000000000000, -3.336006684570783348E-17, 0.000000000000000000 ) ) ;
#43032 = DIRECTION ( 'NONE',  ( 0.000000000000000000, 0.000000000000000000, 1.000000000000000000 ) ) ;
#43033 = EDGE_CURVE ( 'NONE', #2987, #33446, #36492, .T. ) ;
#43034 = ORIENTED_EDGE ( 'NONE', *, *, #26346, .T. ) ;
#43035 = CARTESIAN_POINT ( 'NONE',  ( 0.000000000000000000, -104.6166166098442147, -50.11350645393781633 ) ) ;
#43036 = EDGE_LOOP ( 'NONE', ( #19409, #12513, #39406, #16856 ) ) ;
#43037 = CARTESIAN_POINT ( 'NONE',  ( 0.000000000000000000, 0.000000000000000000, 0.000000000000000000 ) ) ;
#43038 = ORIENTED_EDGE ( 'NONE', *, *, #38940, .F. ) ;
#43040 = ORIENTED_EDGE ( 'NONE', *, *, #36023, .T. ) ;
#43039 = FACE_BOUND ( 'NONE', #28228, .T. ) ;
#43041 = CARTESIAN_POINT ( 'NONE',  ( 59.60939625460783731, 31.00000000000000000, -29.27517545780145269 ) ) ;
#43042 = ORIENTED_EDGE ( 'NONE', *, *, #792, .F. ) ;
#43043 = DIRECTION ( 'NONE',  ( -1.000000000000000000, 0.000000000000000000, 0.000000000000000000 ) ) ;
#43044 = AXIS2_PLACEMENT_3D ( 'NONE', #29637, #19415, #26576 ) ;
#43045 = ORIENTED_EDGE ( 'NONE', *, *, #2891, .F. ) ;
#43046 = AXIS2_PLACEMENT_3D ( 'NONE', #32197, #28310, #34823 ) ;
#43047 = DIRECTION ( 'NONE',  ( 0.000000000000000000, -0.6736956436465636466, 0.7390089172206532053 ) ) ;
#43048 = VERTEX_POINT ( 'NONE', #31883 ) ;
#43049 = AXIS2_PLACEMENT_3D ( 'NONE', #23043, #16921, #6848 ) ;
#43050 = CARTESIAN_POINT ( 'NONE',  ( 10.26812810425290579, 40.00000000000000000, 78.79123036454033979 ) ) ;
#43051 = EDGE_CURVE ( 'NONE', #6792, #3236, #41391, .T. ) ;
#43052 = VECTOR ( 'NONE', #9386, 1000.000000000000000 ) ;
#43054 = DIRECTION ( 'NONE',  ( 0.000000000000000000, 0.000000000000000000, -1.000000000000000000 ) ) ;
#43053 = DIRECTION ( 'NONE',  ( -1.000000000000000000, 0.000000000000000000, -0.000000000000000000 ) ) ;
#43055 = EDGE_CURVE ( 'NONE', #2738, #40340, #3746, .T. ) ;
#43056 = CARTESIAN_POINT ( 'NONE',  ( 9.000000000000001776, -114.1157422997281969, -20.82300072953048442 ) ) ;
#43057 = ORIENTED_EDGE ( 'NONE', *, *, #11020, .T. ) ;
#43058 = DIRECTION ( 'NONE',  ( -1.000000000000000000, -0.000000000000000000, -0.000000000000000000 ) ) ;
#43059 = EDGE_LOOP ( 'NONE', ( #41739, #29361, #13017, #40899 ) ) ;
#43060 = DIRECTION ( 'NONE',  ( 0.000000000000000000, 0.000000000000000000, 1.000000000000000000 ) ) ;
#43061 = CARTESIAN_POINT ( 'NONE',  ( 55.63593431947571588, 31.00000000000000000, -48.80962981700470493 ) ) ;
#43063 = DIRECTION ( 'NONE',  ( 0.000000000000000000, 0.4999999999999990008, -0.8660254037844391517 ) ) ;
#43062 = CARTESIAN_POINT ( 'NONE',  ( -10.00000000000000000, 0.000000000000000000, 0.000000000000000000 ) ) ;
#43064 = EDGE_CURVE ( 'NONE', #41100, #16577, #40694, .T. ) ;
#43065 = ORIENTED_EDGE ( 'NONE', *, *, #9955, .F. ) ;
#43066 = ADVANCED_FACE ( 'NONE', ( #25152 ), #14454, .T. ) ;
#43067 = DIRECTION ( 'NONE',  ( -1.000000000000000000, 0.000000000000000000, 0.000000000000000000 ) ) ;
#43068 = ORIENTED_EDGE ( 'NONE', *, *, #33562, .F. ) ;
#43069 = DIRECTION ( 'NONE',  ( 0.000000000000000000, 0.000000000000000000, 1.000000000000000000 ) ) ;
#43070 = CARTESIAN_POINT ( 'NONE',  ( 18.00000000000000355, 37.91532898920961969, -28.61088654061597936 ) ) ;
#43071 = AXIS2_PLACEMENT_3D ( 'NONE', #15082, #2720, #23078 ) ;
#43072 = CARTESIAN_POINT ( 'NONE',  ( -70.09526419939506070, 31.00000000000000711, -61.63891210113990837 ) ) ;
#43073 = AXIS2_PLACEMENT_3D ( 'NONE', #5008, #5439, #5215 ) ;
#43074 = DIRECTION ( 'NONE',  ( 0.000000000000000000, -0.2486898871648622611, 0.9685831611286290777 ) ) ;
#43075 = CIRCLE ( 'NONE', #14567, 58.99999999999999289 ) ;
#43076 = EDGE_CURVE ( 'NONE', #22654, #21903, #8314, .T. ) ;
#43077 = CARTESIAN_POINT ( 'NONE',  ( 2.250206802516407034, 117.9447454555042754, 2.972870684497274762 ) ) ;
#43078 = EDGE_LOOP ( 'NONE', ( #39838, #15095, #14871, #20165, #2387 ) ) ;
#43079 = DIRECTION ( 'NONE',  ( 1.000000000000000000, 1.836909530733573776E-16, 0.000000000000000000 ) ) ;
#43080 = VERTEX_POINT ( 'NONE', #34925 ) ;
#43081 = VECTOR ( 'NONE', #38222, 1000.000000000000000 ) ;
#43082 = CARTESIAN_POINT ( 'NONE',  ( 17.99999999999999645, 117.9424311864589185, 24.69967462999075281 ) ) ;
#43083 = EDGE_CURVE ( 'NONE', #19640, #14319, #10768, .T. ) ;
#43084 = LINE ( 'NONE', #33696, #41588 ) ;
#43085 = DIRECTION ( 'NONE',  ( -1.000000000000000000, -0.000000000000000000, -0.000000000000000000 ) ) ;
#43086 = ORIENTED_EDGE ( 'NONE', *, *, #32188, .T. ) ;
#43087 = CARTESIAN_POINT ( 'NONE',  ( 8.999999999999998224, 115.0622509503832589, 14.72000021165183803 ) ) ;
#43088 = DIRECTION ( 'NONE',  ( -1.000000000000000000, -0.000000000000000000, -0.000000000000000000 ) ) ;
#43089 = CARTESIAN_POINT ( 'NONE',  ( 0.000000000000000000, 30.01658535635412406, -108.1077105353194838 ) ) ;
#43091 = ORIENTED_EDGE ( 'NONE', *, *, #18569, .T. ) ;
#43090 = FACE_OUTER_BOUND ( 'NONE', #5836, .T. ) ;
#43092 = CARTESIAN_POINT ( 'NONE',  ( 28.69597684714336339, 31.00000000000000355, 25.25520295781697655 ) ) ;
#43093 = DIRECTION ( 'NONE',  ( -1.000000000000000000, -0.000000000000000000, -0.000000000000000000 ) ) ;
#43094 = EDGE_CURVE ( 'NONE', #22222, #3675, #33047, .T. ) ;
#43096 = ORIENTED_EDGE ( 'NONE', *, *, #11522, .F. ) ;
#43095 = CARTESIAN_POINT ( 'NONE',  ( -0.2999999999999999889, -14.69693845669906906, 0.000000000000000000 ) ) ;
#43097 = ORIENTED_EDGE ( 'NONE', *, *, #30677, .F. ) ;
#43098 = DIRECTION ( 'NONE',  ( -1.000000000000000000, 0.000000000000000000, 0.000000000000000000 ) ) ;
#43099 = CARTESIAN_POINT ( 'NONE',  ( 9.000000000000001776, -111.2559044912522950, -32.83479428644788811 ) ) ;
#43100 = CARTESIAN_POINT ( 'NONE',  ( -35.18788409414197815, 40.00000000000000000, -40.25400722681193599 ) ) ;
#43101 = CARTESIAN_POINT ( 'NONE',  ( 0.000000000000000000, 28.57802095670086828, 14.28532136906683370 ) ) ;
#43102 = EDGE_CURVE ( 'NONE', #4953, #31904, #18392, .T. ) ;
#43104 = EDGE_CURVE ( 'NONE', #6927, #35878, #42774, .T. ) ;
#43103 = CIRCLE ( 'NONE', #41014, 59.00000000000000000 ) ;
#43105 = CIRCLE ( 'NONE', #30616, 19.99999999999999645 ) ;
#43106 = CARTESIAN_POINT ( 'NONE',  ( 0.000000000000000000, -42.03146605346801579, 22.12489237027304512 ) ) ;
#43107 = ADVANCED_FACE ( 'NONE', ( #24714 ), #24506, .F. ) ;
#43108 = EDGE_CURVE ( 'NONE', #20315, #553, #25435, .T. ) ;
#43109 = LINE ( 'NONE', #19392, #4624 ) ;
#43110 = ORIENTED_EDGE ( 'NONE', *, *, #15778, .T. ) ;
#43111 = CIRCLE ( 'NONE', #39646, 13.59999999999999964 ) ;
#43112 = CARTESIAN_POINT ( 'NONE',  ( 17.99999999999999645, -13.57797752207901532, -33.34124362422488730 ) ) ;
#43113 = VERTEX_POINT ( 'NONE', #37971 ) ;
#43114 = CARTESIAN_POINT ( 'NONE',  ( 0.000000000000000000, -111.7974656912330715, 9.465682155095141326 ) ) ;
#43115 = DIRECTION ( 'NONE',  ( 1.000000000000000000, -1.373900992973641671E-15, -3.895519384649692070E-16 ) ) ;
#43116 = CARTESIAN_POINT ( 'NONE',  ( 43.96541952717798551, 31.00000000000000355, 11.76906328551413239 ) ) ;
#43117 = CARTESIAN_POINT ( 'NONE',  ( 17.99999999999999645, -66.49630760163542220, -90.36876423296052963 ) ) ;
#43118 = ORIENTED_EDGE ( 'NONE', *, *, #32483, .T. ) ;
#43119 = CARTESIAN_POINT ( 'NONE',  ( 0.000000000000000000, 9.484061862024356415, -30.03730300138970932 ) ) ;
#43120 = ORIENTED_EDGE ( 'NONE', *, *, #7254, .T. ) ;
#43121 = CARTESIAN_POINT ( 'NONE',  ( -12.78314611188302052, 31.00000000000000355, 97.07982689498881257 ) ) ;
#43122 = ORIENTED_EDGE ( 'NONE', *, *, #6434, .T. ) ;
#43123 = DIRECTION ( 'NONE',  ( 1.000000000000000000, 0.000000000000000000, 0.000000000000000000 ) ) ;
#43124 = VERTEX_POINT ( 'NONE', #31240 ) ;
#43125 = CARTESIAN_POINT ( 'NONE',  ( 43.45541166190962912, 31.00000000000000355, -49.38773770141698805 ) ) ;
#43126 = CARTESIAN_POINT ( 'NONE',  ( 21.04585062969761822, 40.00000000000000000, -61.66509230325024760 ) ) ;
#43127 = CARTESIAN_POINT ( 'NONE',  ( 76.36724925129128394, 39.99999999999999289, 58.57876755120444301 ) ) ;
#43128 = EDGE_LOOP ( 'NONE', ( #9553, #15702, #15001, #15903 ) ) ;
#43129 = EDGE_LOOP ( 'NONE', ( #22814, #15761 ) ) ;
#43130 = CARTESIAN_POINT ( 'NONE',  ( 17.99999999999999645, -99.97660604679919061, -67.26937820704989690 ) ) ;
#43131 = CARTESIAN_POINT ( 'NONE',  ( -23.00000000000000000, 0.000000000000000000, -6.000000000000000000 ) ) ;
#43132 = CYLINDRICAL_SURFACE ( 'NONE', #31710, 13.59999999999999964 ) ;
#43133 = ADVANCED_FACE ( 'NONE', ( #21462 ), #34710, .T. ) ;
#43134 = CIRCLE ( 'NONE', #6916, 52.00000000000000000 ) ;
#43135 = AXIS2_PLACEMENT_3D ( 'NONE', #30879, #30456, #536 ) ;
#43137 = ORIENTED_EDGE ( 'NONE', *, *, #42015, .F. ) ;
#43136 = CARTESIAN_POINT ( 'NONE',  ( 17.99999999999999645, -97.19627249181141337, 71.22763238166453448 ) ) ;
#43138 = FACE_OUTER_BOUND ( 'NONE', #13334, .T. ) ;
#43139 = VERTEX_POINT ( 'NONE', #27902 ) ;
#43140 = DIRECTION ( 'NONE',  ( -1.000000000000000000, -0.000000000000000000, -0.000000000000000000 ) ) ;
#43141 = CIRCLE ( 'NONE', #24386, 120.5010000000000332 ) ;
#43142 = CARTESIAN_POINT ( 'NONE',  ( -39.09256291070916944, 40.00000000000000000, 79.30589209199378331 ) ) ;
#43143 = CARTESIAN_POINT ( 'NONE',  ( -10.00000000000000000, 0.000000000000000000, 0.000000000000000000 ) ) ;
#43144 = ORIENTED_EDGE ( 'NONE', *, *, #15539, .T. ) ;
#43145 = CARTESIAN_POINT ( 'NONE',  ( 17.99999999999999645, -35.72777019205738469, 106.3569410558016273 ) ) ;
#43146 = DIRECTION ( 'NONE',  ( 0.000000000000000000, 0.9048270524660205760, -0.4257792915650704391 ) ) ;
#43147 = ORIENTED_EDGE ( 'NONE', *, *, #32703, .F. ) ;
#43148 = ORIENTED_EDGE ( 'NONE', *, *, #27314, .T. ) ;
#43149 = LINE ( 'NONE', #16802, #33024 ) ;
#43150 = VERTEX_POINT ( 'NONE', #10649 ) ;
#43151 = DIRECTION ( 'NONE',  ( 0.000000000000000000, 0.000000000000000000, 1.000000000000000000 ) ) ;
#43152 = DIRECTION ( 'NONE',  ( 0.000000000000000000, -0.9048270524660235736, 0.4257792915650641663 ) ) ;
#43153 = CARTESIAN_POINT ( 'NONE',  ( 0.000000000000000000, 44.25018368420781911, -27.31155879685132959 ) ) ;
#43154 = DIRECTION ( 'NONE',  ( 1.000000000000000000, 0.000000000000000000, 0.000000000000000000 ) ) ;
#43155 = EDGE_CURVE ( 'NONE', #19720, #35521, #1691, .T. ) ;
#43156 = ADVANCED_FACE ( 'NONE', ( #36827 ), #27452, .F. ) ;
#43157 = CARTESIAN_POINT ( 'NONE',  ( 3.999999999999999112, -1.539600717839012978, -3.300726591567080703 ) ) ;
#43158 = ORIENTED_EDGE ( 'NONE', *, *, #13536, .F. ) ;
#43159 = DIRECTION ( 'NONE',  ( -1.000000000000000000, -0.000000000000000000, -0.000000000000000000 ) ) ;
#43160 = EDGE_CURVE ( 'NONE', #18913, #37390, #9349, .T. ) ;
#43161 = ORIENTED_EDGE ( 'NONE', *, *, #6928, .F. ) ;
#43162 = CARTESIAN_POINT ( 'NONE',  ( 2.000000000000005329, -3.464101615137751722, 0.000000000000000000 ) ) ;
#43164 = CARTESIAN_POINT ( 'NONE',  ( 2.650000000000182876, -150.5000000000013642, 6.999999999999585221 ) ) ;
#43163 = AXIS2_PLACEMENT_3D ( 'NONE', #7906, #27563, #10991 ) ;
#43165 = ORIENTED_EDGE ( 'NONE', *, *, #2425, .F. ) ;
#43166 = CARTESIAN_POINT ( 'NONE',  ( 18.00000000000000355, -7.162210897276081845, 51.50439529848825515 ) ) ;
#43167 = CARTESIAN_POINT ( 'NONE',  ( 3.239593890920906993, -13.56862304811759223, 0.000000000000000000 ) ) ;
#43168 = SHAPE_DEFINITION_REPRESENTATION ( #15828, #15194 ) ;
#43169 = DIRECTION ( 'NONE',  ( -1.000000000000000000, 0.000000000000000000, 0.000000000000000000 ) ) ;
#43170 = CARTESIAN_POINT ( 'NONE',  ( -3.763366191185464782, 31.00000000000000355, 57.60416666550938203 ) ) ;
#43171 = ADVANCED_FACE ( 'NONE', ( #34199 ), #40514, .F. ) ;
#43172 = ORIENTED_EDGE ( 'NONE', *, *, #17310, .T. ) ;
#43173 = CARTESIAN_POINT ( 'NONE',  ( 36.95980244579787666, 31.00000000000000355, 4.931273285801173856 ) ) ;
#43174 = CARTESIAN_POINT ( 'NONE',  ( 17.40022565512299479, 40.00000000000000000, 64.93645345284011228 ) ) ;
#43175 = SURFACE_STYLE_FILL_AREA ( #29914 ) ;
#43176 = DIRECTION ( 'NONE',  ( 3.996523416598930318E-16, -2.658563593772947863E-15, -1.000000000000000000 ) ) ;
#43177 = ORIENTED_EDGE ( 'NONE', *, *, #564, .T. ) ;
#43178 = CARTESIAN_POINT ( 'NONE',  ( 9.000000000000001776, -39.64889472655755753, 33.64468972902493960 ) ) ;
#43179 = DIRECTION ( 'NONE',  ( 1.000000000000000000, 0.000000000000000000, 0.000000000000000000 ) ) ;
#43180 = ORIENTED_EDGE ( 'NONE', *, *, #30693, .T. ) ;
#43181 = CARTESIAN_POINT ( 'NONE',  ( -27.33276042269523387, 40.00000000000000000, -31.15086293565511966 ) ) ;
#43182 = CARTESIAN_POINT ( 'NONE',  ( -91.96080130434580724, -35.35525454449571470, 14.45886780445738218 ) ) ;
#43183 = NEXT_ASSEMBLY_USAGE_OCCURRENCE ( 'NAUO1', ' ', ' ', #10820, #2408, $ ) ;
#43184 = NEXT_ASSEMBLY_USAGE_OCCURRENCE ( 'NAUO2', ' ', ' ', #10820, #32055, $ ) ;
#43185 = NEXT_ASSEMBLY_USAGE_OCCURRENCE ( 'NAUO3', ' ', ' ', #10820, #10989, $ ) ;
#43186 = NEXT_ASSEMBLY_USAGE_OCCURRENCE ( 'NAUO4', ' ', ' ', #10820, #15380, $ ) ;
#43187 = NEXT_ASSEMBLY_USAGE_OCCURRENCE ( 'NAUO5', ' ', ' ', #10820, #3027, $ ) ;
#43188 = NEXT_ASSEMBLY_USAGE_OCCURRENCE ( 'NAUO6', ' ', ' ', #10820, #3027, $ ) ;
#43189 = NEXT_ASSEMBLY_USAGE_OCCURRENCE ( 'NAUO7', ' ', ' ', #10820, #3027, $ ) ;
#43190 = NEXT_ASSEMBLY_USAGE_OCCURRENCE ( 'NAUO8', ' ', ' ', #10820, #27627, $ ) ;
#43191 = NEXT_ASSEMBLY_USAGE_OCCURRENCE ( 'NAUO9', ' ', ' ', #10820, #27627, $ ) ;
#43192 = NEXT_ASSEMBLY_USAGE_OCCURRENCE ( 'NAUO10', ' ', ' ', #10820, #27627, $ ) ;
#43193 = NEXT_ASSEMBLY_USAGE_OCCURRENCE ( 'NAUO11', ' ', ' ', #10820, #37893, $ ) ;
#43194 = NEXT_ASSEMBLY_USAGE_OCCURRENCE ( 'NAUO12', ' ', ' ', #10820, #37893, $ ) ;
#43195 = NEXT_ASSEMBLY_USAGE_OCCURRENCE ( 'NAUO13', ' ', ' ', #10820, #37893, $ ) ;
#43196 = NEXT_ASSEMBLY_USAGE_OCCURRENCE ( 'NAUO14', ' ', ' ', #10820, #35852, $ ) ;
#43197 = NEXT_ASSEMBLY_USAGE_OCCURRENCE ( 'NAUO15', ' ', ' ', #10820, #8157, $ ) ;
#43198 = NEXT_ASSEMBLY_USAGE_OCCURRENCE ( 'NAUO16', ' ', ' ', #10820, #23650, $ ) ;
#43199 = NEXT_ASSEMBLY_USAGE_OCCURRENCE ( 'NAUO17', ' ', ' ', #10820, #8157, $ ) ;
#43200 = NEXT_ASSEMBLY_USAGE_OCCURRENCE ( 'NAUO18', ' ', ' ', #10820, #4380, $ ) ;
#43201 = NEXT_ASSEMBLY_USAGE_OCCURRENCE ( 'NAUO19', ' ', ' ', #10820, #4380, $ ) ;
#43202 = NEXT_ASSEMBLY_USAGE_OCCURRENCE ( 'NAUO20', ' ', ' ', #10820, #4380, $ ) ;
#43203 = NEXT_ASSEMBLY_USAGE_OCCURRENCE ( 'NAUO21', ' ', ' ', #10820, #4380, $ ) ;
#43204 = NEXT_ASSEMBLY_USAGE_OCCURRENCE ( 'NAUO22', ' ', ' ', #10820, #4380, $ ) ;
#43205 = NEXT_ASSEMBLY_USAGE_OCCURRENCE ( 'NAUO23', ' ', ' ', #10820, #4380, $ ) ;
#43206 = NEXT_ASSEMBLY_USAGE_OCCURRENCE ( 'NAUO24', ' ', ' ', #10820, #4380, $ ) ;
#43207 = NEXT_ASSEMBLY_USAGE_OCCURRENCE ( 'NAUO25', ' ', ' ', #10820, #4380, $ ) ;
#43208 = NEXT_ASSEMBLY_USAGE_OCCURRENCE ( 'NAUO26', ' ', ' ', #10820, #20446, $ ) ;
#43209 = NEXT_ASSEMBLY_USAGE_OCCURRENCE ( 'NAUO27', ' ', ' ', #10820, #20446, $ ) ;
#43210 = NEXT_ASSEMBLY_USAGE_OCCURRENCE ( 'NAUO28', ' ', ' ', #10820, #20446, $ ) ;
#43211 = NEXT_ASSEMBLY_USAGE_OCCURRENCE ( 'NAUO29', ' ', ' ', #10820, #20446, $ ) ;
#43212 = NEXT_ASSEMBLY_USAGE_OCCURRENCE ( 'NAUO30', ' ', ' ', #10820, #20446, $ ) ;
#43213 = NEXT_ASSEMBLY_USAGE_OCCURRENCE ( 'NAUO31', ' ', ' ', #10820, #20446, $ ) ;
#43214 = NEXT_ASSEMBLY_USAGE_OCCURRENCE ( 'NAUO32', ' ', ' ', #10820, #20446, $ ) ;
#43215 = NEXT_ASSEMBLY_USAGE_OCCURRENCE ( 'NAUO33', ' ', ' ', #10820, #20446, $ ) ;
ENDSEC;
END-ISO-10303-21;
